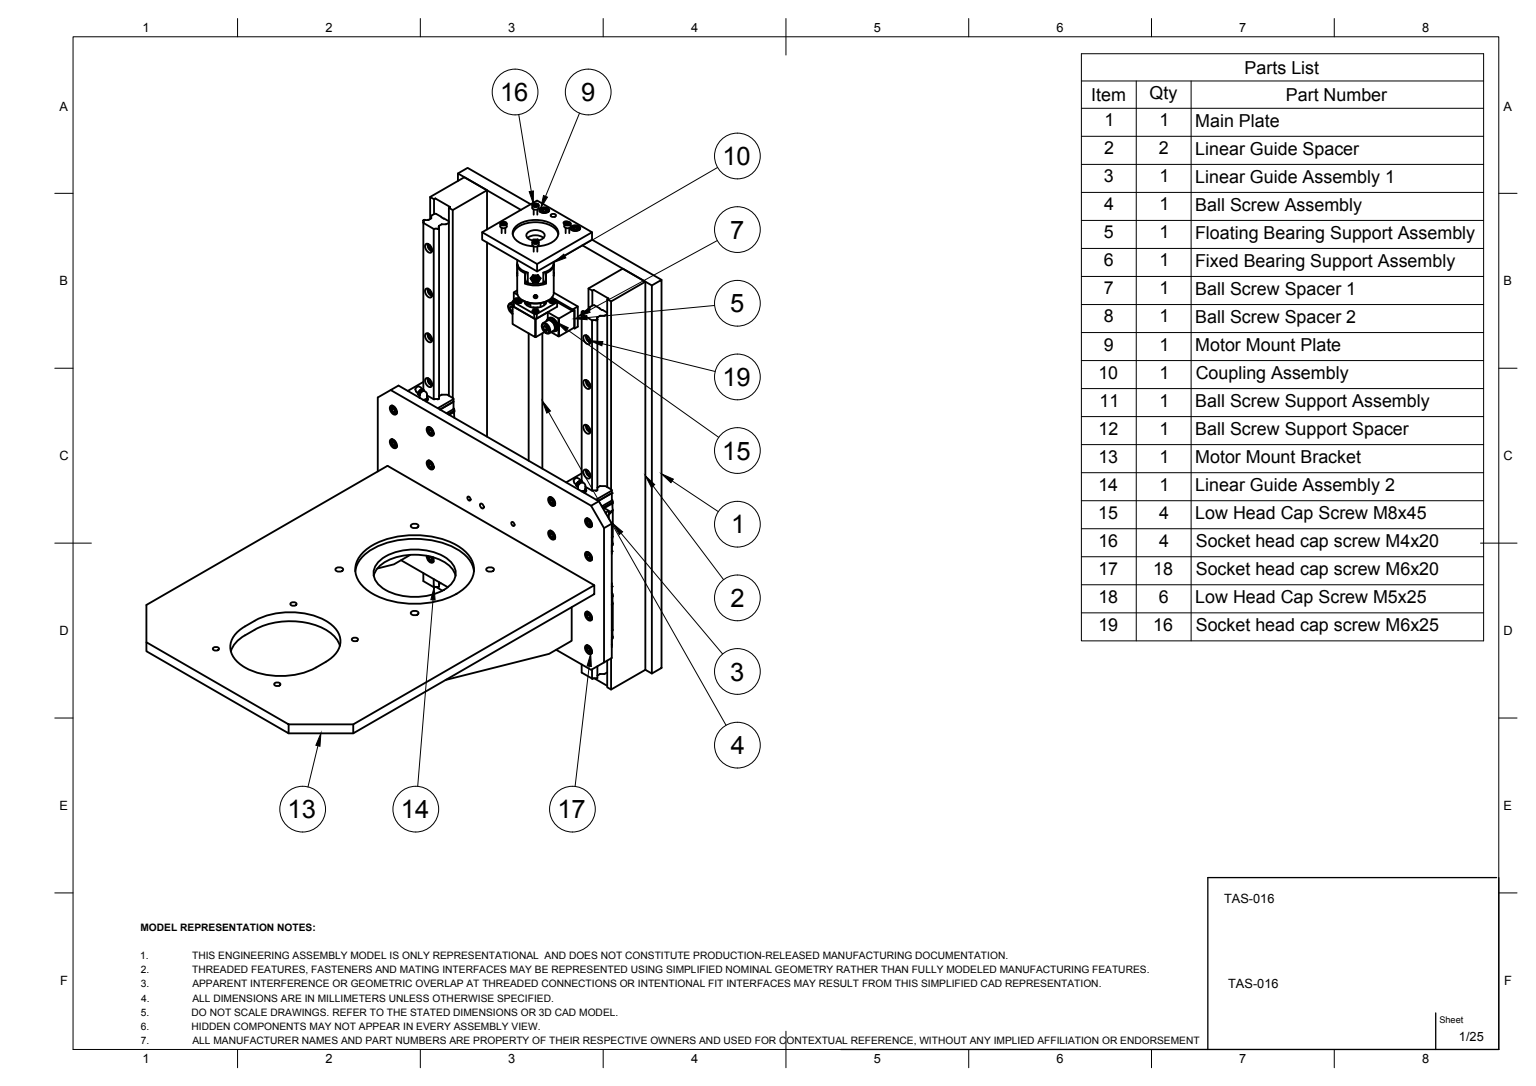
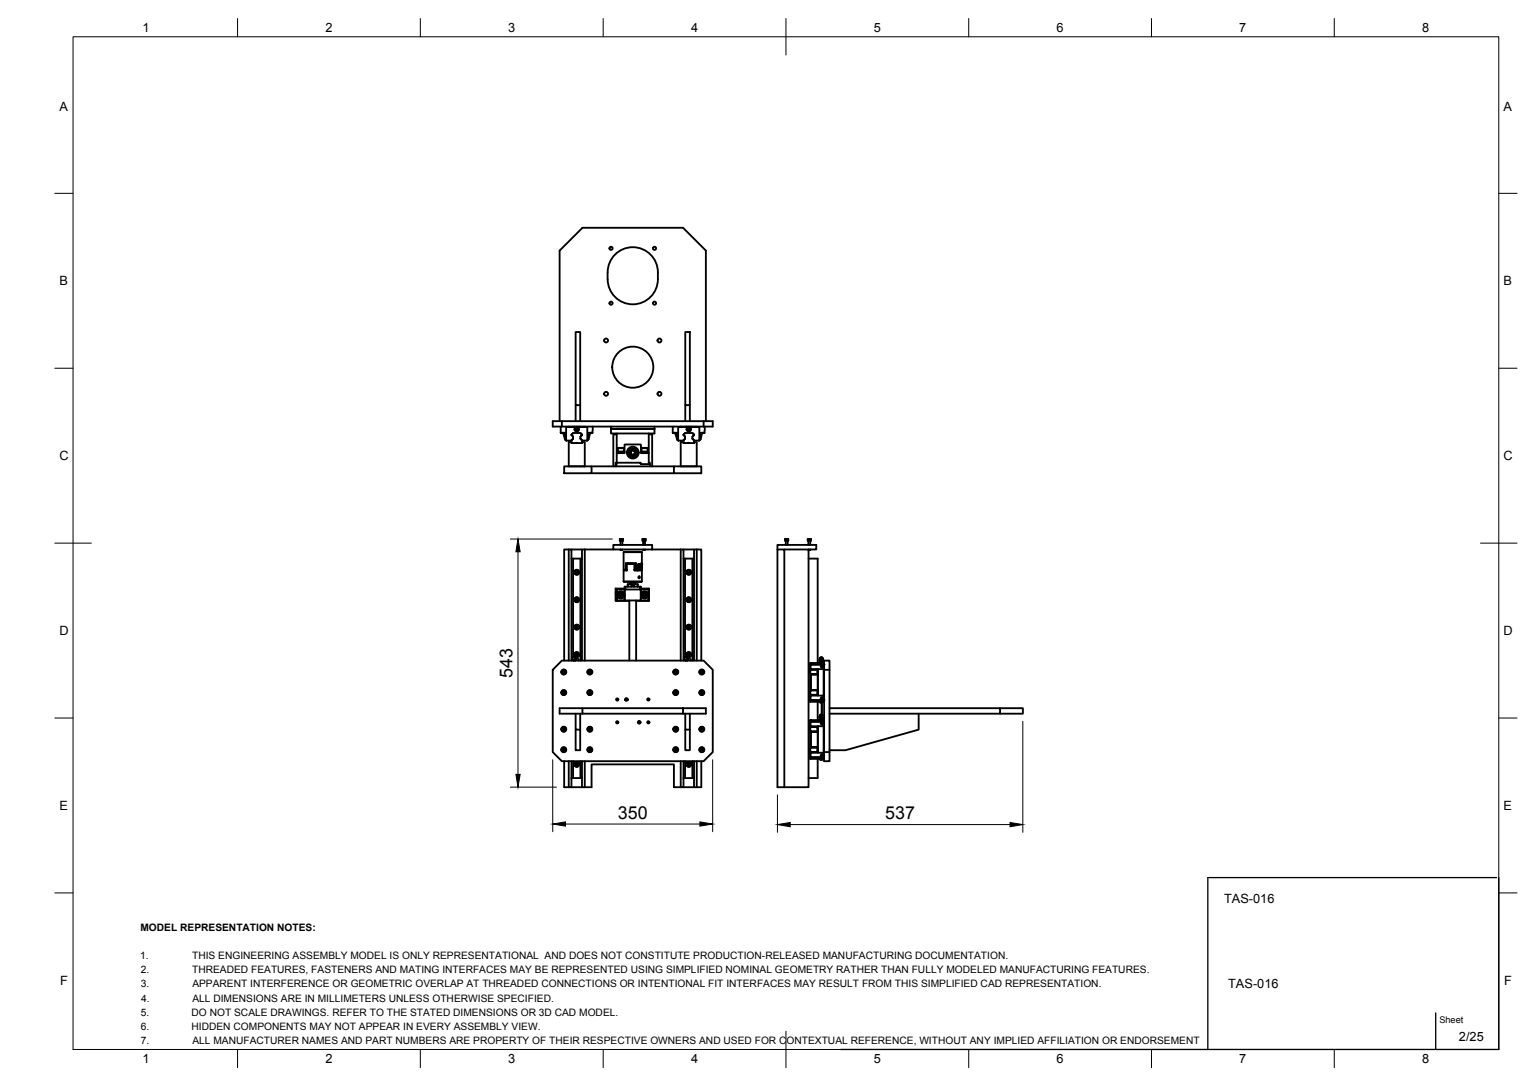
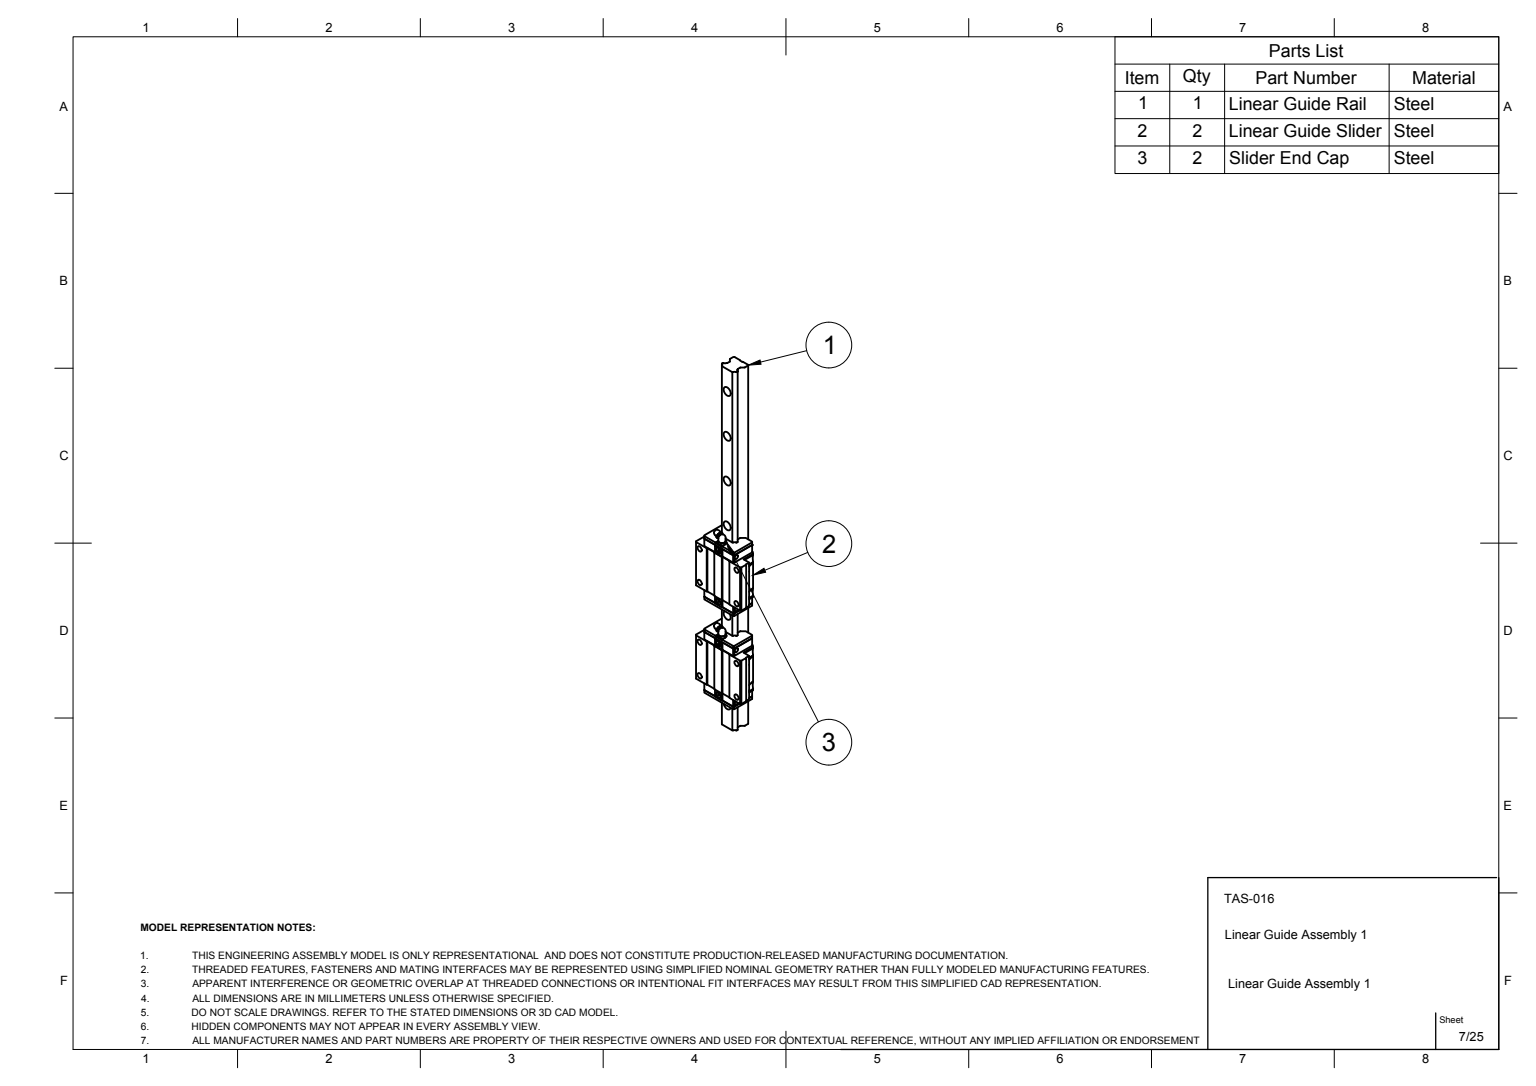
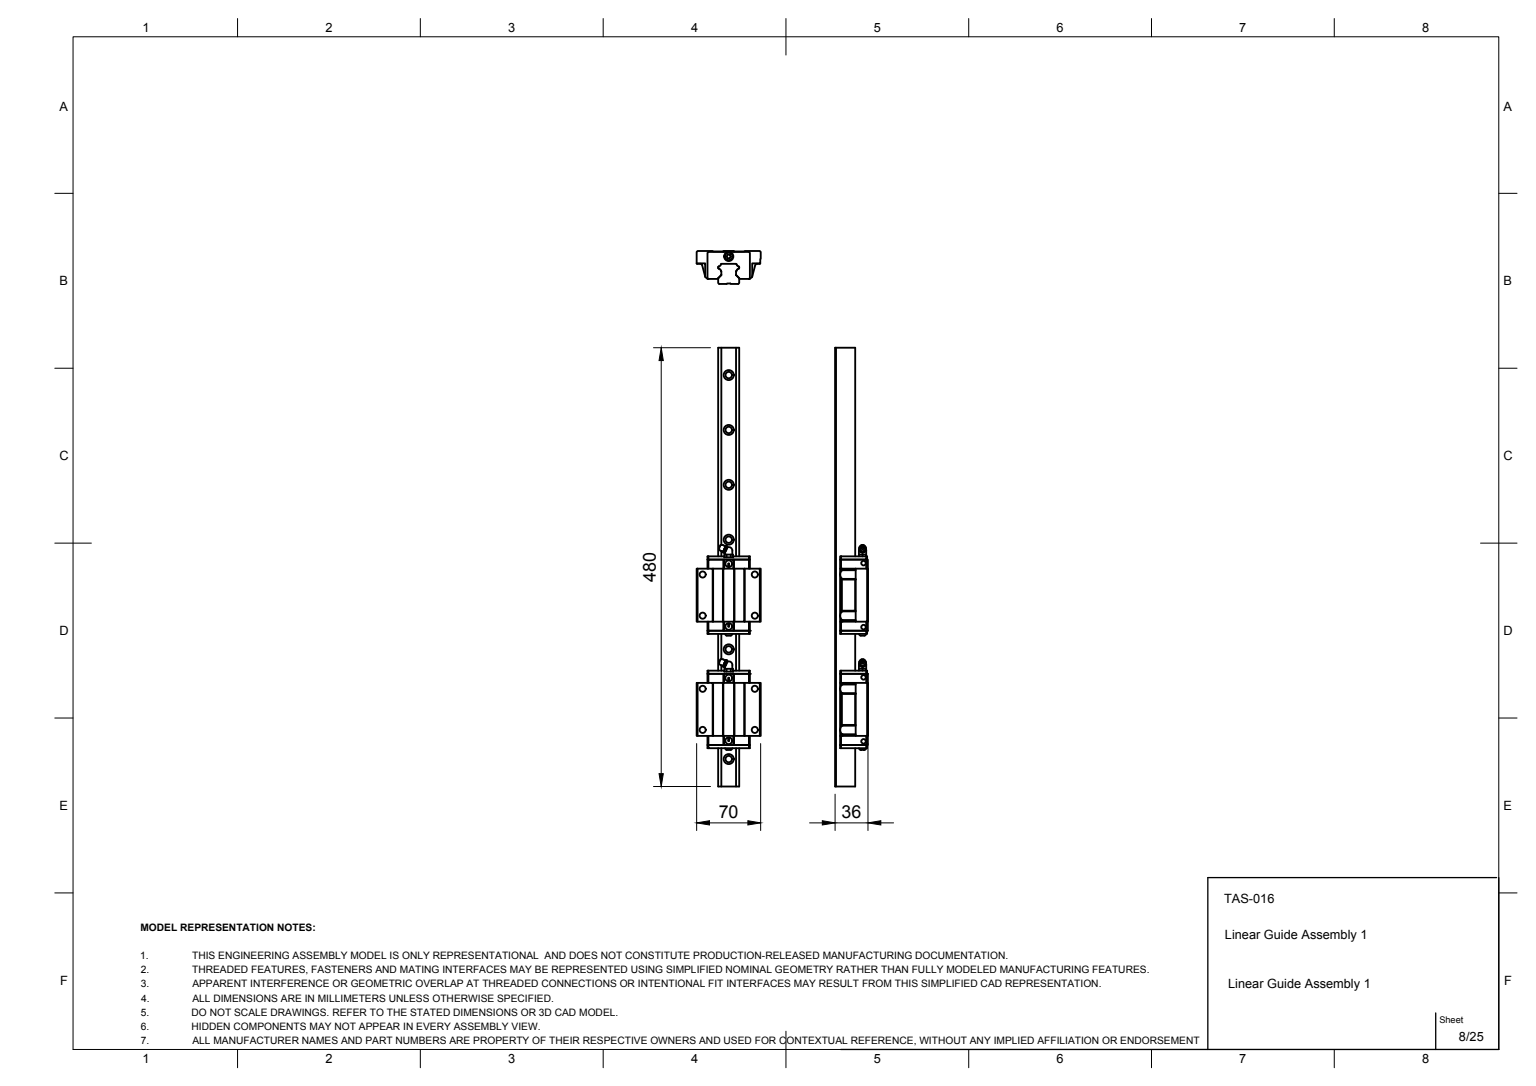
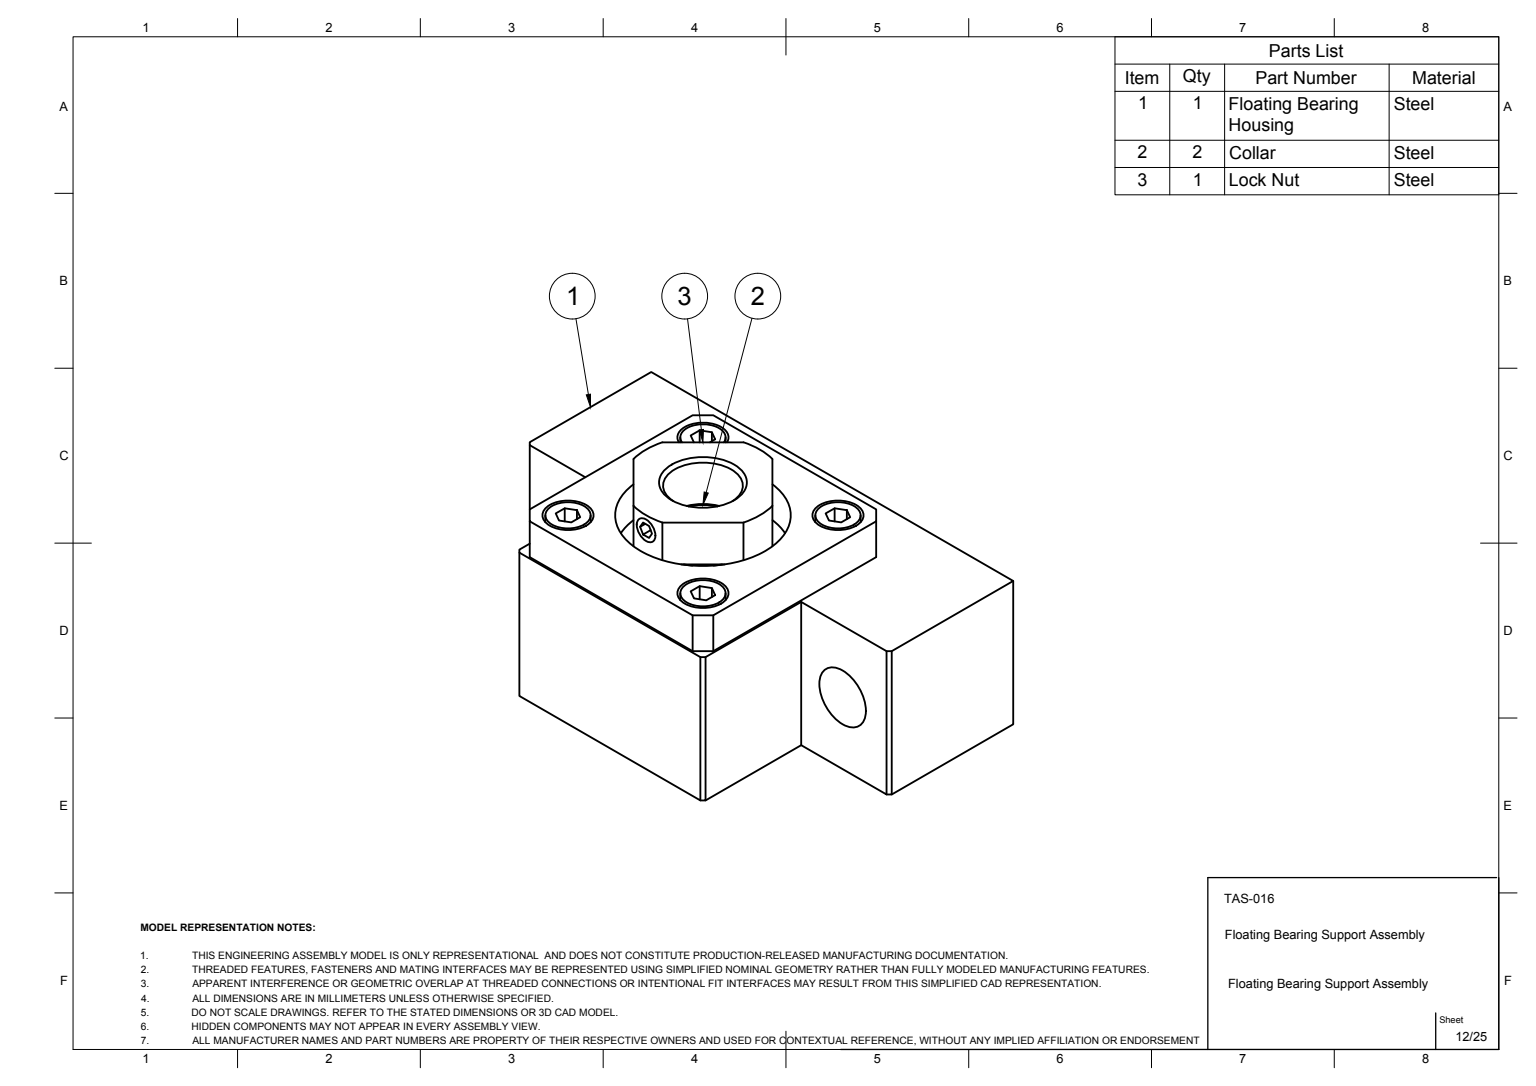
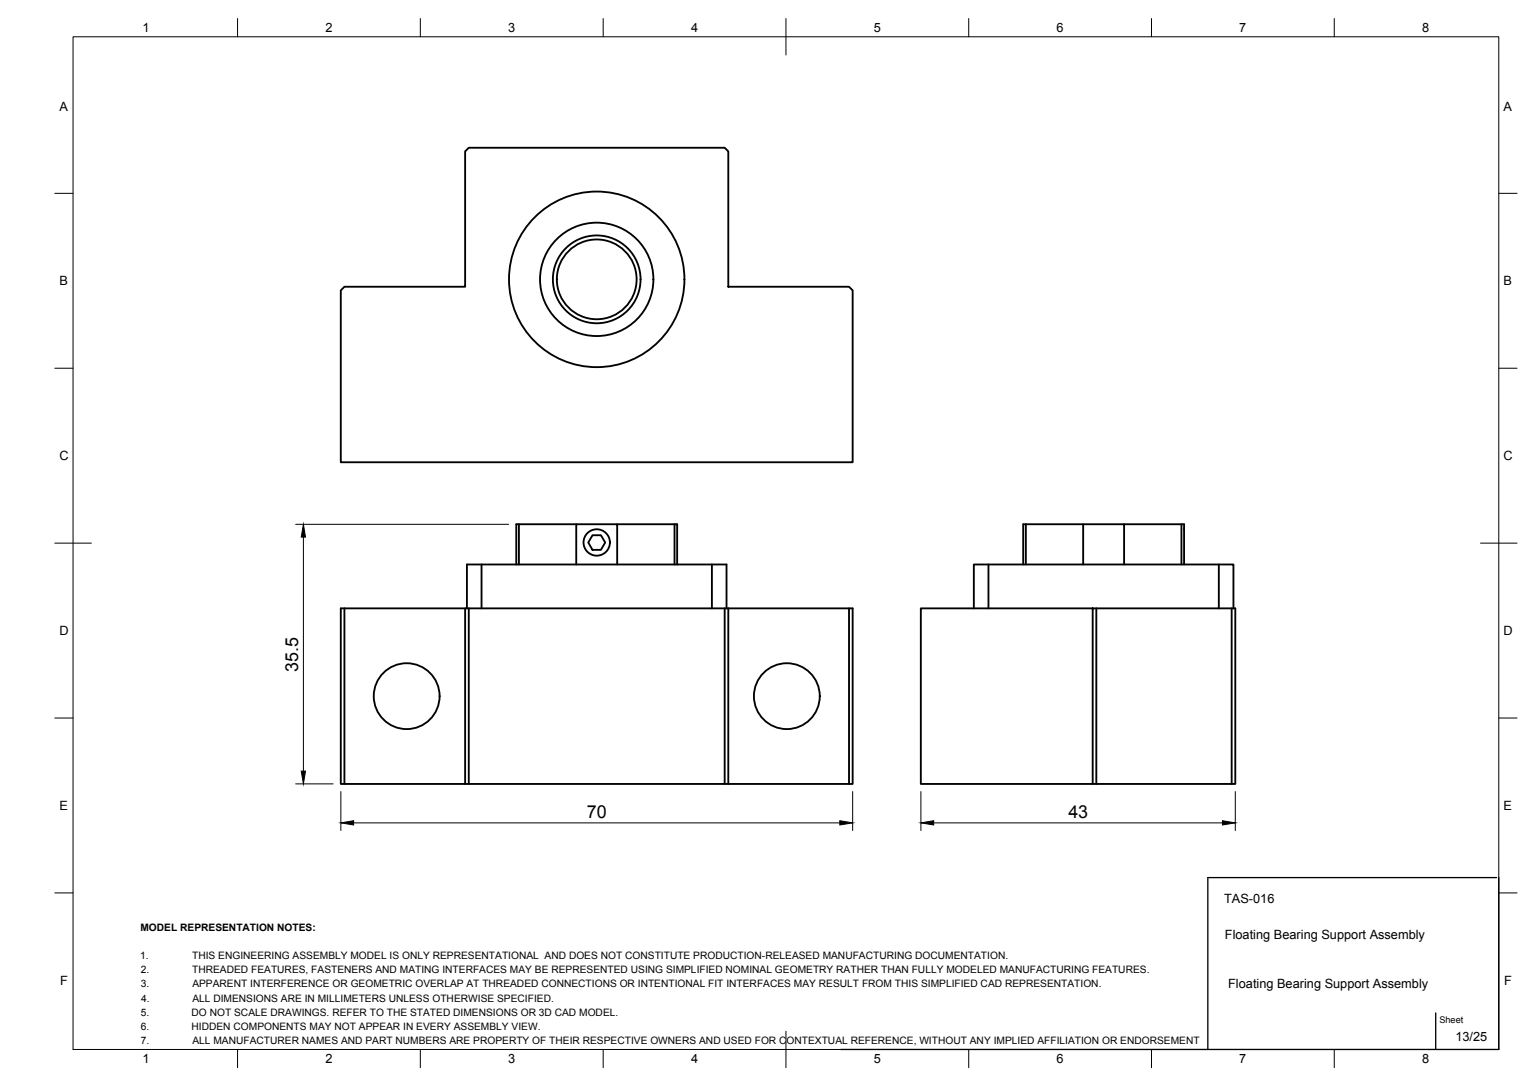
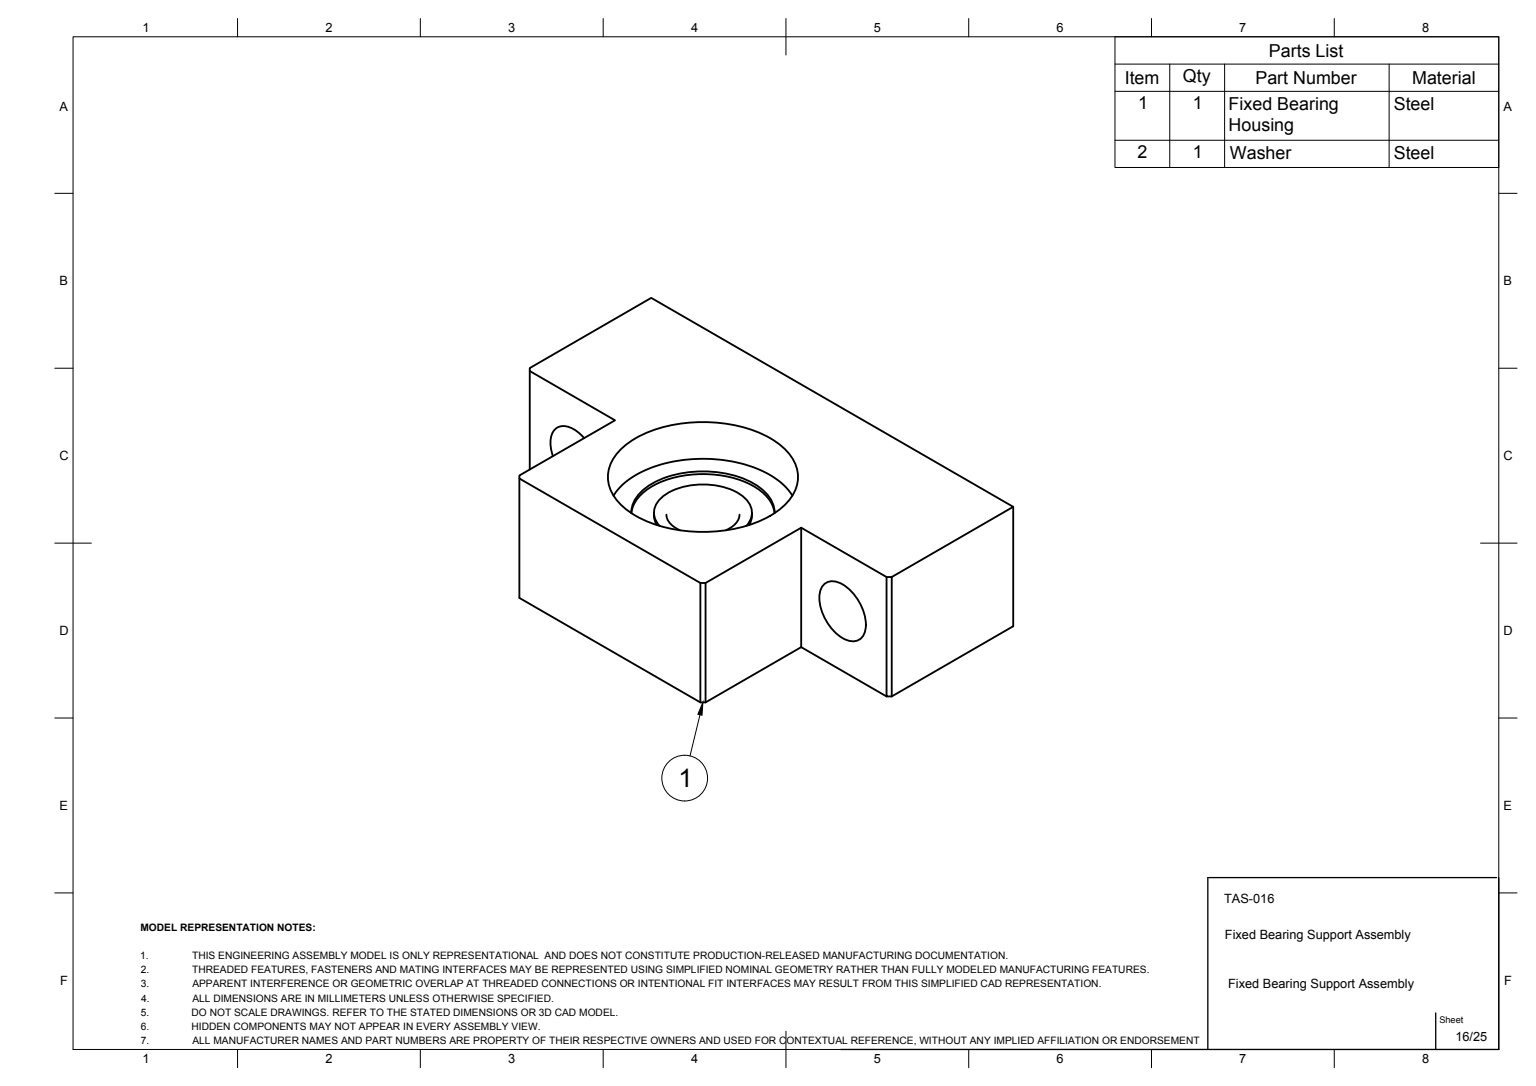
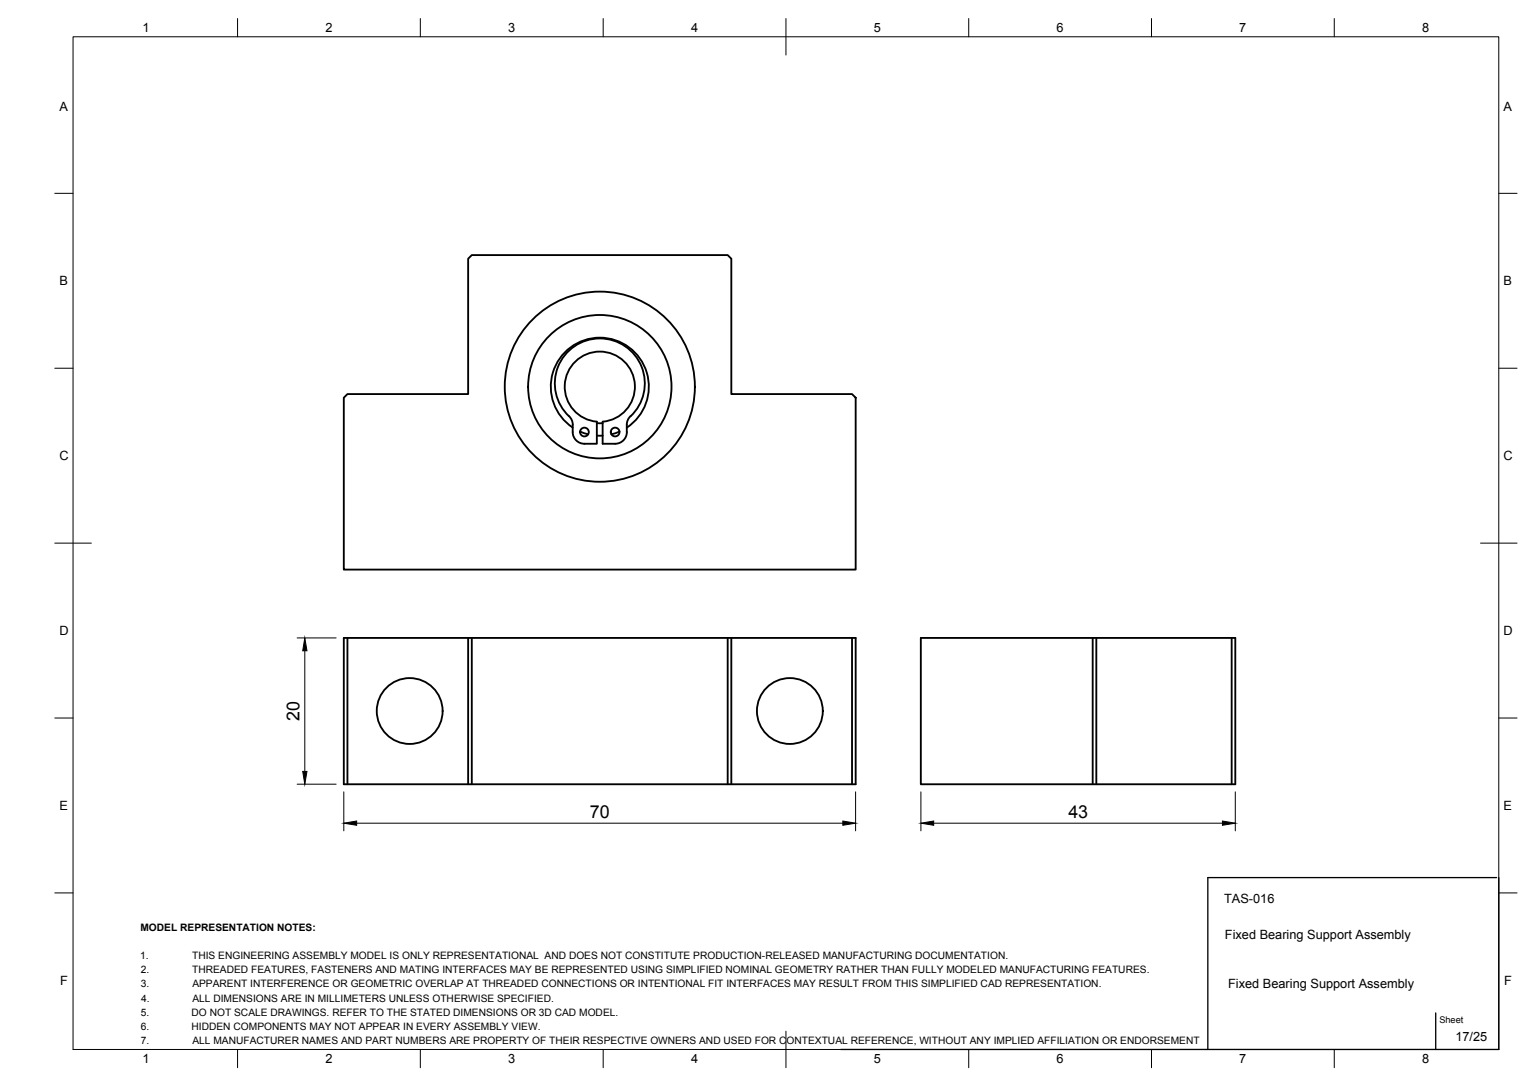
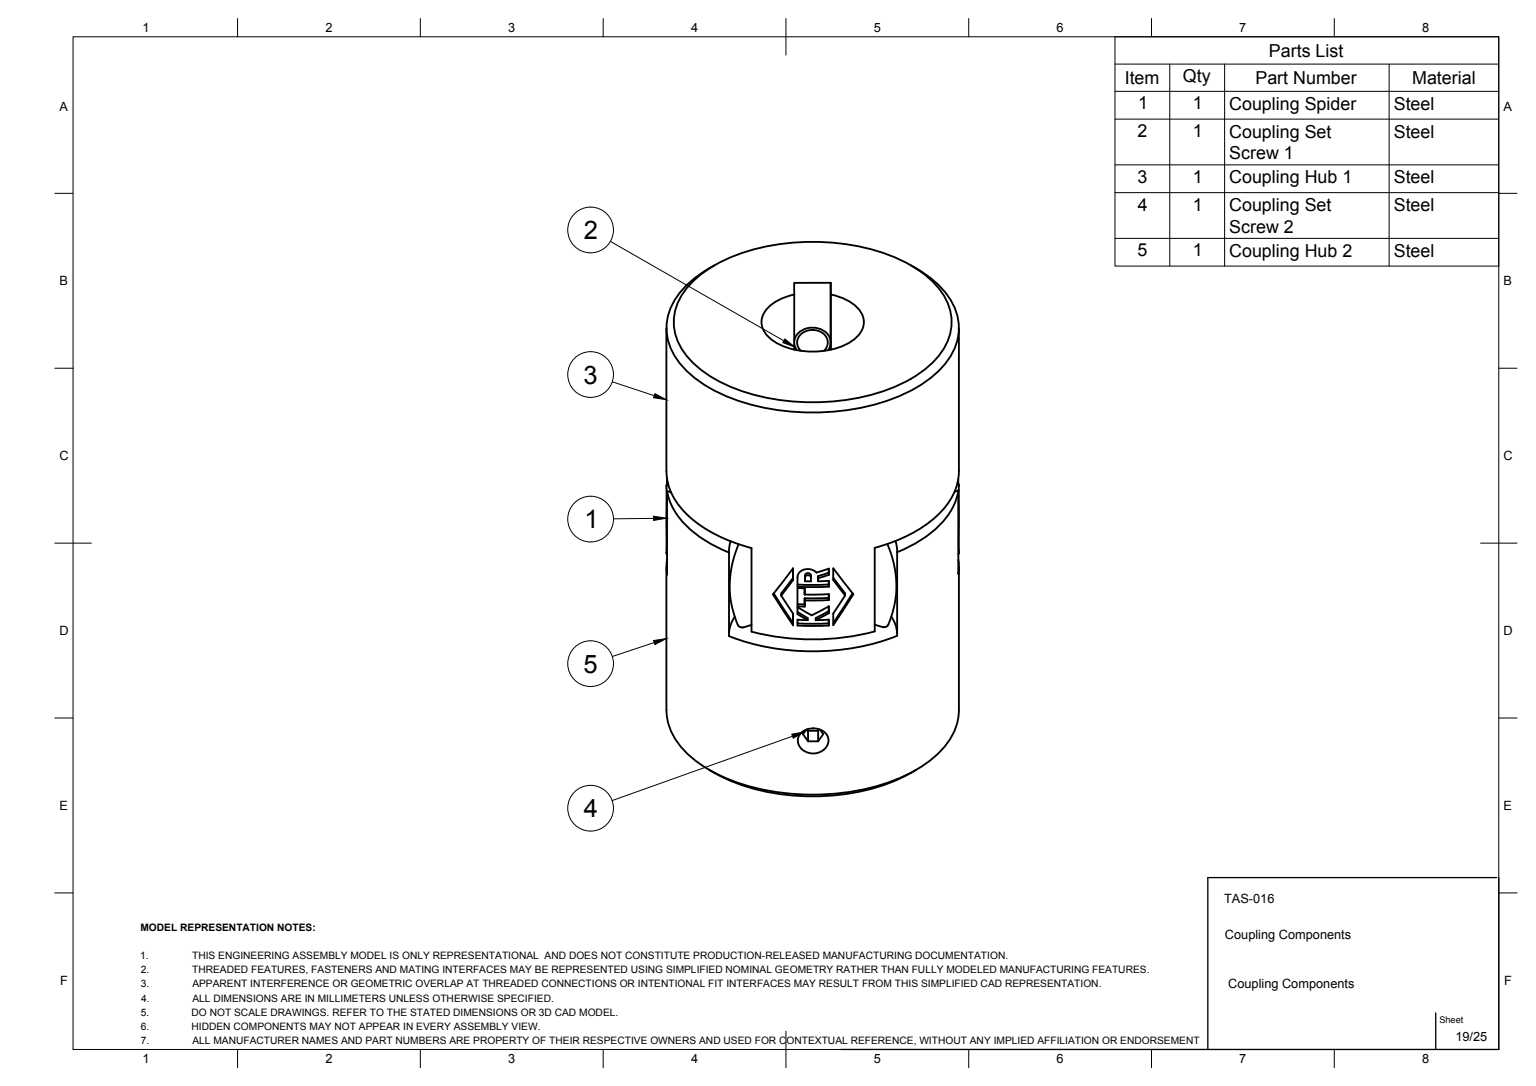
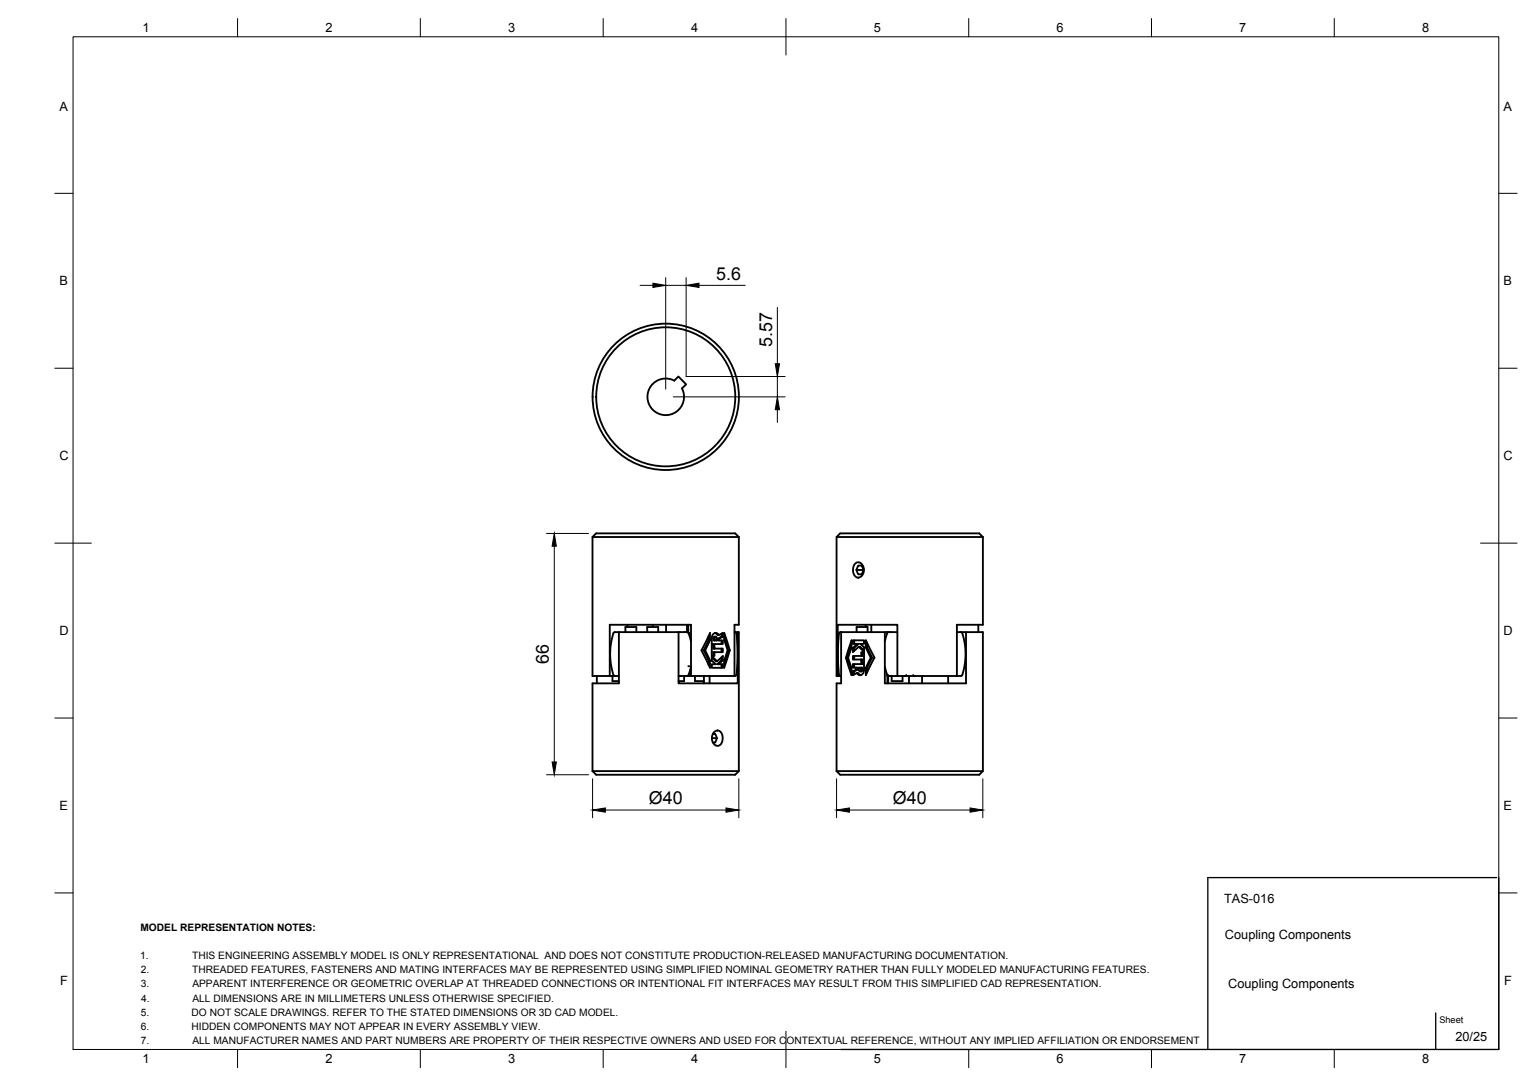
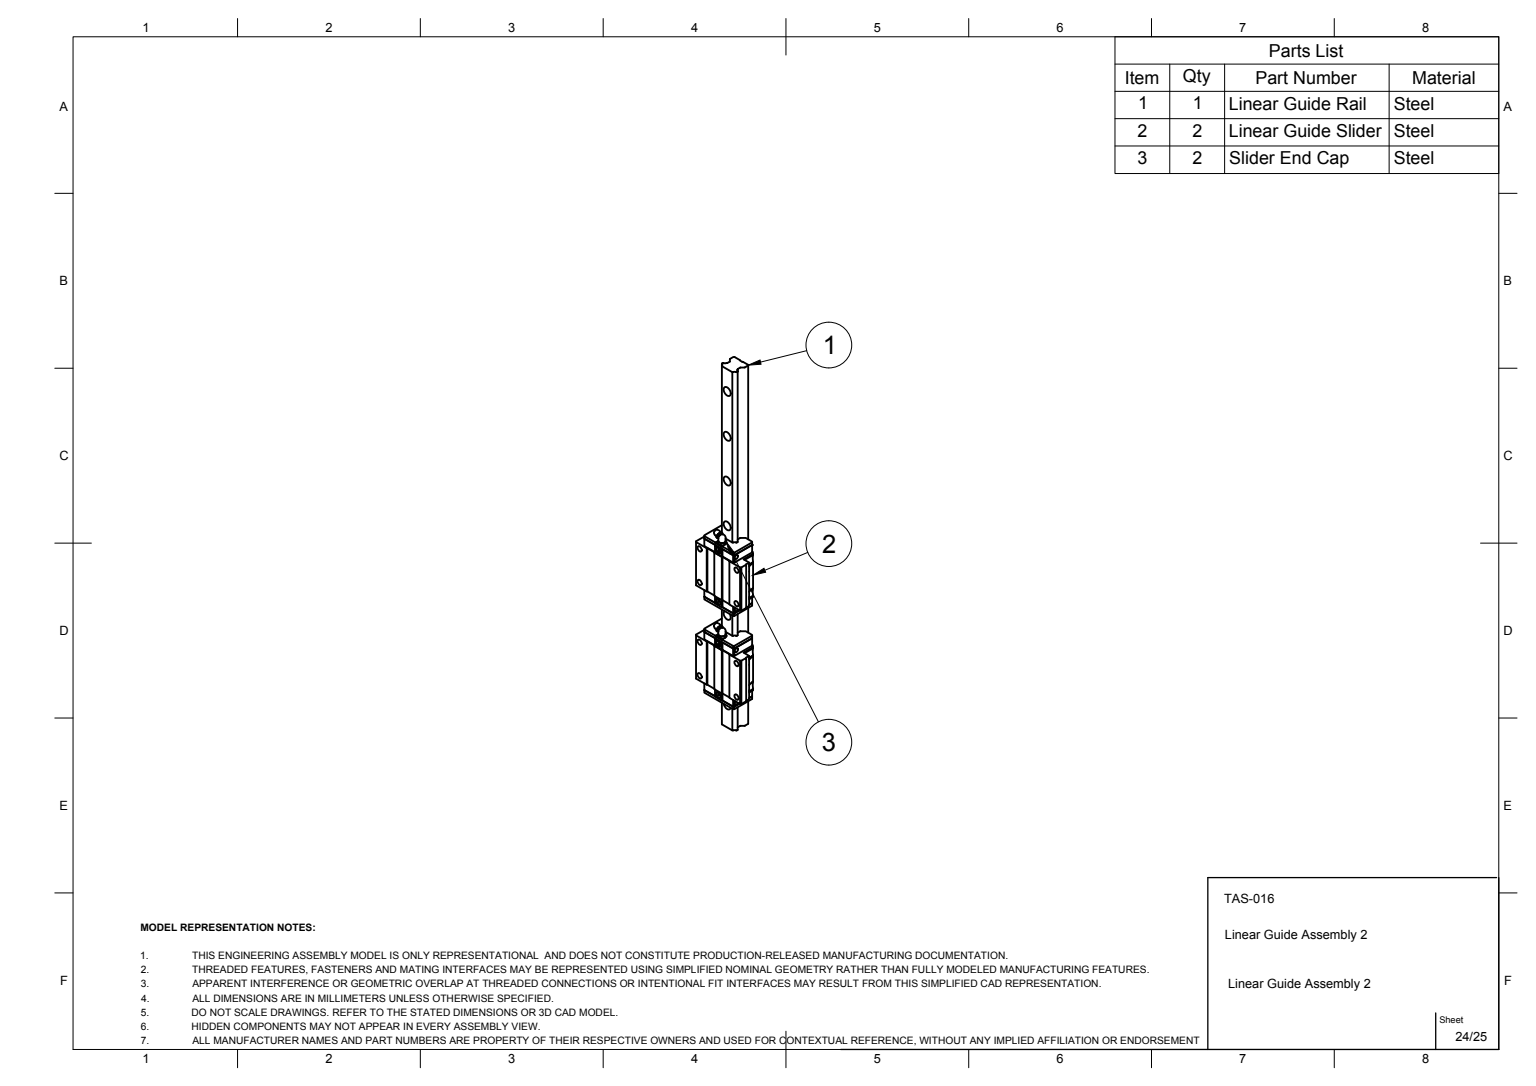
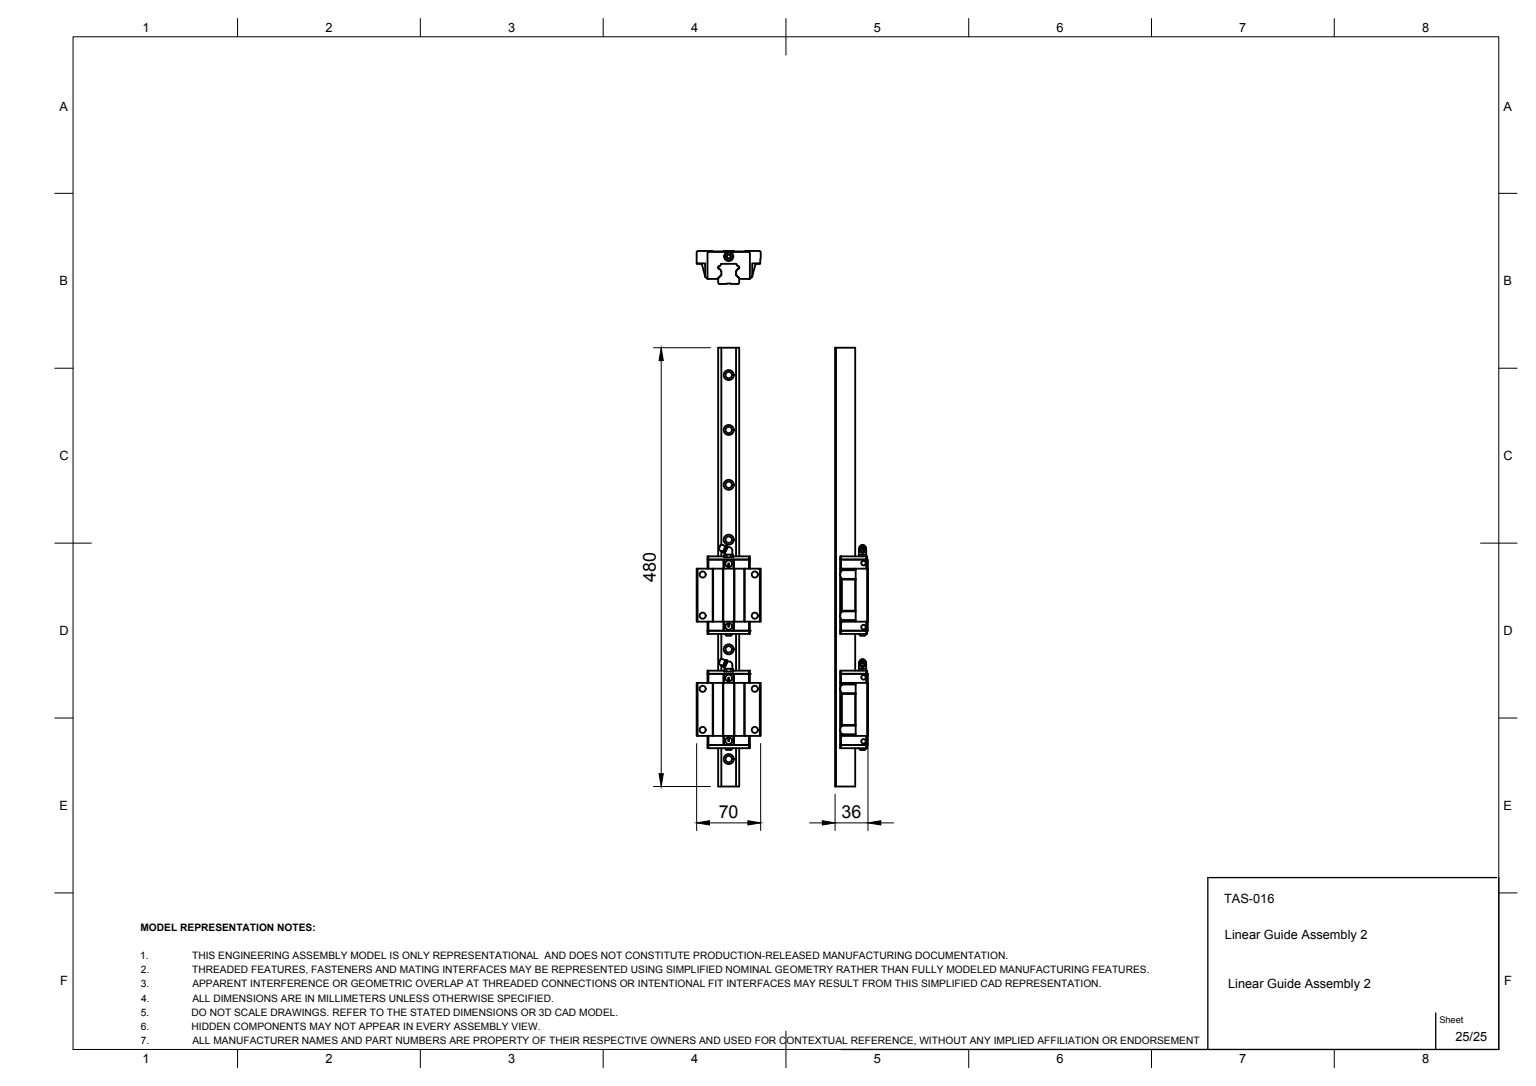
ISO-10303-21;
HEADER;
/* Generated by software containing ST-Developer
 * from STEP Tools, Inc. (www.steptools.com) 
 */

FILE_DESCRIPTION(
/* description */ ('STEP AP214'),
/* implementation_level */ '2;1');

FILE_NAME(
/* name */ 'TAS-016.step',
/* time_stamp */ '2026-11-15T14:55:55-08:00',
/* author */ (''),
/* organization */ (''),
/* preprocessor_version */ 'ST-DEVELOPER v20.2',
/* originating_system */ 'Autodesk Translation Framework v15.17.0.0',
/* authorisation */ '');

FILE_SCHEMA (('AUTOMOTIVE_DESIGN { 1 0 10303 214 3 1 1 }'));
ENDSEC;

DATA;
#10=MECHANICAL_DESIGN_GEOMETRIC_PRESENTATION_REPRESENTATION('',(#926,#927,
#928,#929,#930,#931,#932,#933,#934,#935,#936,#937,#938,#939,#940,#941,#942,
#943,#944,#945,#946,#947,#948,#949,#950,#951,#952,#953,#954,#955,#956,#957,
#958,#959,#960,#961,#962),#57079);
#11=(
BOUNDED_CURVE()
B_SPLINE_CURVE(2,(#54195,#54196,#54197),.UNSPECIFIED.,.F.,.F.)
B_SPLINE_CURVE_WITH_KNOTS((3,3),(-1.29356557390797,0.),.UNSPECIFIED.)
CURVE()
GEOMETRIC_REPRESENTATION_ITEM()
RATIONAL_B_SPLINE_CURVE((0.954658532851732,0.77704632554749,1.))
REPRESENTATION_ITEM('')
);
#12=(
BOUNDED_CURVE()
B_SPLINE_CURVE(2,(#56108,#56109,#56110),.UNSPECIFIED.,.F.,.F.)
B_SPLINE_CURVE_WITH_KNOTS((3,3),(-1.38994780338837,-1.00314154055664),
 .UNSPECIFIED.)
CURVE()
GEOMETRIC_REPRESENTATION_ITEM()
RATIONAL_B_SPLINE_CURVE((1.79495951130746,1.93380011269289,1.93380011269289))
REPRESENTATION_ITEM('')
);
#13=(
BOUNDED_CURVE()
B_SPLINE_CURVE(2,(#56111,#56112,#56113),.UNSPECIFIED.,.F.,.F.)
B_SPLINE_CURVE_WITH_KNOTS((3,3),(-1.00619430729118,-0.618602381117838),
 .UNSPECIFIED.)
CURVE()
GEOMETRIC_REPRESENTATION_ITEM()
RATIONAL_B_SPLINE_CURVE((1.93745653739061,1.93745653739061,1.7983534165231))
REPRESENTATION_ITEM('')
);
#14=(
BOUNDED_CURVE()
B_SPLINE_CURVE(2,(#56119,#56120,#56121),.UNSPECIFIED.,.F.,.F.)
B_SPLINE_CURVE_WITH_KNOTS((3,3),(-1.38994780338837,-1.00314154055664),
 .UNSPECIFIED.)
CURVE()
GEOMETRIC_REPRESENTATION_ITEM()
RATIONAL_B_SPLINE_CURVE((1.79495951130745,1.93380011269288,1.93380011269288))
REPRESENTATION_ITEM('')
);
#15=(
BOUNDED_CURVE()
B_SPLINE_CURVE(2,(#56122,#56123,#56124),.UNSPECIFIED.,.F.,.F.)
B_SPLINE_CURVE_WITH_KNOTS((3,3),(-1.00619430729117,-0.618602381117832),
 .UNSPECIFIED.)
CURVE()
GEOMETRIC_REPRESENTATION_ITEM()
RATIONAL_B_SPLINE_CURVE((1.9374565373906,1.9374565373906,1.79835341652309))
REPRESENTATION_ITEM('')
);
#16=(
BOUNDED_CURVE()
B_SPLINE_CURVE(2,(#56246,#56247,#56248),.UNSPECIFIED.,.F.,.F.)
B_SPLINE_CURVE_WITH_KNOTS((3,3),(-1.14357963809553,-0.720457873954785),
 .UNSPECIFIED.)
CURVE()
GEOMETRIC_REPRESENTATION_ITEM()
RATIONAL_B_SPLINE_CURVE((2.10284386262275,2.10284386262275,1.95186646604709))
REPRESENTATION_ITEM('')
);
#17=(
BOUNDED_CURVE()
B_SPLINE_CURVE(2,(#56249,#56250,#56251),.UNSPECIFIED.,.F.,.F.)
B_SPLINE_CURVE_WITH_KNOTS((3,3),(-1.51402948258723,-1.10175646251728),
 .UNSPECIFIED.)
CURVE()
GEOMETRIC_REPRESENTATION_ITEM()
RATIONAL_B_SPLINE_CURVE((1.90498640166842,2.0523376126434,2.0523376126434))
REPRESENTATION_ITEM('')
);
#18=(
BOUNDED_CURVE()
B_SPLINE_CURVE(2,(#56254,#56255,#56256),.UNSPECIFIED.,.F.,.F.)
B_SPLINE_CURVE_WITH_KNOTS((3,3),(-1.00619430729147,-0.618602381118052),
 .UNSPECIFIED.)
CURVE()
GEOMETRIC_REPRESENTATION_ITEM()
RATIONAL_B_SPLINE_CURVE((1.93745653739095,1.93745653739095,1.79835341652342))
REPRESENTATION_ITEM('')
);
#19=(
BOUNDED_CURVE()
B_SPLINE_CURVE(2,(#56257,#56258,#56259),.UNSPECIFIED.,.F.,.F.)
B_SPLINE_CURVE_WITH_KNOTS((3,3),(-1.59428966155348,-1.16547770853232),
 .UNSPECIFIED.)
CURVE()
GEOMETRIC_REPRESENTATION_ITEM()
RATIONAL_B_SPLINE_CURVE((1.97645710138757,2.12933659022722,2.12933659022723))
REPRESENTATION_ITEM('')
);
#20=(
BOUNDED_CURVE()
B_SPLINE_CURVE(2,(#56262,#56263,#56264),.UNSPECIFIED.,.F.,.F.)
B_SPLINE_CURVE_WITH_KNOTS((3,3),(-1.39378623346489,-1.00619430729147),
 .UNSPECIFIED.)
CURVE()
GEOMETRIC_REPRESENTATION_ITEM()
RATIONAL_B_SPLINE_CURVE((1.79835341652342,1.93745653739095,1.93745653739095))
REPRESENTATION_ITEM('')
);
#21=(
BOUNDED_CURVE()
B_SPLINE_CURVE(2,(#56265,#56266,#56267),.UNSPECIFIED.,.F.,.F.)
B_SPLINE_CURVE_WITH_KNOTS((3,3),(-1.00314154055692,-0.616335277725119),
 .UNSPECIFIED.)
CURVE()
GEOMETRIC_REPRESENTATION_ITEM()
RATIONAL_B_SPLINE_CURVE((1.93380011269323,1.93380011269323,1.79495951130777))
REPRESENTATION_ITEM('')
);
#22=(
BOUNDED_CURVE()
B_SPLINE_CURVE(2,(#56270,#56271,#56272),.UNSPECIFIED.,.F.,.F.)
B_SPLINE_CURVE_WITH_KNOTS((3,3),(-1.38994780338873,-1.00314154055692),
 .UNSPECIFIED.)
CURVE()
GEOMETRIC_REPRESENTATION_ITEM()
RATIONAL_B_SPLINE_CURVE((1.79495951130777,1.93380011269323,1.93380011269323))
REPRESENTATION_ITEM('')
);
#23=(
BOUNDED_CURVE()
B_SPLINE_CURVE(2,(#56273,#56274,#56275),.UNSPECIFIED.,.F.,.F.)
B_SPLINE_CURVE_WITH_KNOTS((3,3),(-1.16547770853232,-0.73666575551116),
 .UNSPECIFIED.)
CURVE()
GEOMETRIC_REPRESENTATION_ITEM()
RATIONAL_B_SPLINE_CURVE((2.12933659022723,2.12933659022723,1.97645710138758))
REPRESENTATION_ITEM('')
);
#24=(
BOUNDED_CURVE()
B_SPLINE_CURVE(2,(#56278,#56279,#56280),.UNSPECIFIED.,.F.,.F.)
B_SPLINE_CURVE_WITH_KNOTS((3,3),(-1.56670140223628,-1.14357963809553),
 .UNSPECIFIED.)
CURVE()
GEOMETRIC_REPRESENTATION_ITEM()
RATIONAL_B_SPLINE_CURVE((1.95186646604709,2.10284386262275,2.10284386262275))
REPRESENTATION_ITEM('')
);
#25=(
BOUNDED_CURVE()
B_SPLINE_CURVE(2,(#56281,#56282,#56283),.UNSPECIFIED.,.F.,.F.)
B_SPLINE_CURVE_WITH_KNOTS((3,3),(-1.09872453323964,-0.687236958819027),
 .UNSPECIFIED.)
CURVE()
GEOMETRIC_REPRESENTATION_ITEM()
RATIONAL_B_SPLINE_CURVE((2.04868118794568,2.04868118794568,1.90159249645282))
REPRESENTATION_ITEM('')
);
#26=(
BOUNDED_CURVE()
B_SPLINE_CURVE(2,(#56286,#56287,#56288),.UNSPECIFIED.,.F.,.F.)
B_SPLINE_CURVE_WITH_KNOTS((3,3),(-1.56670140224009,-1.14357963809856),
 .UNSPECIFIED.)
CURVE()
GEOMETRIC_REPRESENTATION_ITEM()
RATIONAL_B_SPLINE_CURVE((1.9518664660505,2.10284386262641,2.10284386262641))
REPRESENTATION_ITEM('')
);
#27=(
BOUNDED_CURVE()
B_SPLINE_CURVE(2,(#56289,#56290,#56291),.UNSPECIFIED.,.F.,.F.)
B_SPLINE_CURVE_WITH_KNOTS((3,3),(-1.10777980342349,-0.69394596557458),
 .UNSPECIFIED.)
CURVE()
GEOMETRIC_REPRESENTATION_ITEM()
RATIONAL_B_SPLINE_CURVE((2.05960365436383,2.05960365436383,1.91173076506448))
REPRESENTATION_ITEM('')
);
#28=(
BOUNDED_CURVE()
B_SPLINE_CURVE(2,(#56294,#56295,#56296),.UNSPECIFIED.,.F.,.F.)
B_SPLINE_CURVE_WITH_KNOTS((3,3),(-1.40141169651805,-1.01225852375907),
 .UNSPECIFIED.)
CURVE()
GEOMETRIC_REPRESENTATION_ITEM()
RATIONAL_B_SPLINE_CURVE((1.80509777991977,1.94472257911162,1.94472257911162))
REPRESENTATION_ITEM('')
);
#29=(
BOUNDED_CURVE()
B_SPLINE_CURVE(2,(#56297,#56298,#56299),.UNSPECIFIED.,.F.,.F.)
B_SPLINE_CURVE_WITH_KNOTS((3,3),(-1.16547770853319,-0.736665755511809),
 .UNSPECIFIED.)
CURVE()
GEOMETRIC_REPRESENTATION_ITEM()
RATIONAL_B_SPLINE_CURVE((2.12933659022829,2.12933659022829,1.97645710138856))
REPRESENTATION_ITEM('')
);
#30=(
BOUNDED_CURVE()
B_SPLINE_CURVE(2,(#56302,#56303,#56304),.UNSPECIFIED.,.F.,.F.)
B_SPLINE_CURVE_WITH_KNOTS((3,3),(-1.40141169651807,-1.01225852375909),
 .UNSPECIFIED.)
CURVE()
GEOMETRIC_REPRESENTATION_ITEM()
RATIONAL_B_SPLINE_CURVE((1.80509777991979,1.94472257911164,1.94472257911164))
REPRESENTATION_ITEM('')
);
#31=(
BOUNDED_CURVE()
B_SPLINE_CURVE(2,(#56305,#56306,#56307),.UNSPECIFIED.,.F.,.F.)
B_SPLINE_CURVE_WITH_KNOTS((3,3),(-1.01225852375907,-0.623105351000092),
 .UNSPECIFIED.)
CURVE()
GEOMETRIC_REPRESENTATION_ITEM()
RATIONAL_B_SPLINE_CURVE((1.94472257911162,1.94472257911162,1.80509777991977))
REPRESENTATION_ITEM('')
);
#32=(
BOUNDED_CURVE()
B_SPLINE_CURVE(2,(#56310,#56311,#56312),.UNSPECIFIED.,.F.,.F.)
B_SPLINE_CURVE_WITH_KNOTS((3,3),(-1.59428966155458,-1.16547770853319),
 .UNSPECIFIED.)
CURVE()
GEOMETRIC_REPRESENTATION_ITEM()
RATIONAL_B_SPLINE_CURVE((1.97645710138856,2.12933659022828,2.12933659022828))
REPRESENTATION_ITEM('')
);
#33=(
BOUNDED_CURVE()
B_SPLINE_CURVE(2,(#56313,#56314,#56315),.UNSPECIFIED.,.F.,.F.)
B_SPLINE_CURVE_WITH_KNOTS((3,3),(-1.01225852375909,-0.623105351000104),
 .UNSPECIFIED.)
CURVE()
GEOMETRIC_REPRESENTATION_ITEM()
RATIONAL_B_SPLINE_CURVE((1.94472257911164,1.94472257911164,1.80509777991979))
REPRESENTATION_ITEM('')
);
#34=(
BOUNDED_CURVE()
B_SPLINE_CURVE(2,(#56318,#56319,#56320),.UNSPECIFIED.,.F.,.F.)
B_SPLINE_CURVE_WITH_KNOTS((3,3),(-1.52161364127241,-1.1077798034235),
 .UNSPECIFIED.)
CURVE()
GEOMETRIC_REPRESENTATION_ITEM()
RATIONAL_B_SPLINE_CURVE((1.91173076506449,2.05960365436384,2.05960365436384))
REPRESENTATION_ITEM('')
);
#35=(
BOUNDED_CURVE()
B_SPLINE_CURVE(2,(#56321,#56322,#56323),.UNSPECIFIED.,.F.,.F.)
B_SPLINE_CURVE_WITH_KNOTS((3,3),(-1.14357963809856,-0.720457873957025),
 .UNSPECIFIED.)
CURVE()
GEOMETRIC_REPRESENTATION_ITEM()
RATIONAL_B_SPLINE_CURVE((2.10284386262641,2.10284386262641,1.95186646605049))
REPRESENTATION_ITEM('')
);
#36=B_SPLINE_SURFACE_WITH_KNOTS('',3,3,((#37392,#37393,#37394,#37395,#37396),
(#37397,#37398,#37399,#37400,#37401),(#37402,#37403,#37404,#37405,#37406),
(#37407,#37408,#37409,#37410,#37411),(#37412,#37413,#37414,#37415,#37416),
(#37417,#37418,#37419,#37420,#37421),(#37422,#37423,#37424,#37425,#37426)),
 .UNSPECIFIED.,.F.,.F.,.F.,(4,1,1,1,4),(4,1,4),(0.002628442342492,0.25,
0.5,0.75,0.9693574094799),(0.1621510896547,6.217857289747,12.27407139219),
 .UNSPECIFIED.);
#37=B_SPLINE_SURFACE_WITH_KNOTS('',3,3,((#38122,#38123,#38124,#38125,#38126),
(#38127,#38128,#38129,#38130,#38131),(#38132,#38133,#38134,#38135,#38136),
(#38137,#38138,#38139,#38140,#38141)),.UNSPECIFIED.,.F.,.F.,.F.,(4,4),(4,
1,4),(-0.024990257354348,0.982485330053312),(0.334063910607008,6.217857289747,
12.1016506682418),.UNSPECIFIED.);
#38=B_SPLINE_SURFACE_WITH_KNOTS('',3,3,((#38952,#38953,#38954,#38955,#38956),
(#38957,#38958,#38959,#38960,#38961),(#38962,#38963,#38964,#38965,#38966),
(#38967,#38968,#38969,#38970,#38971),(#38972,#38973,#38974,#38975,#38976),
(#38977,#38978,#38979,#38980,#38981),(#38982,#38983,#38984,#38985,#38986)),
 .UNSPECIFIED.,.F.,.F.,.F.,(4,1,1,1,4),(4,1,4),(0.0306420330999,0.25,0.5,
0.75,0.9973715693979),(0.1621509986241,6.217857289747,12.27408153313),
 .UNSPECIFIED.);
#39=B_SPLINE_SURFACE_WITH_KNOTS('',3,3,((#39922,#39923,#39924,#39925,#39926),
(#39927,#39928,#39929,#39930,#39931),(#39932,#39933,#39934,#39935,#39936),
(#39937,#39938,#39939,#39940,#39941),(#39942,#39943,#39944,#39945,#39946),
(#39947,#39948,#39949,#39950,#39951),(#39952,#39953,#39954,#39955,#39956)),
 .UNSPECIFIED.,.F.,.F.,.F.,(4,1,1,1,4),(4,1,4),(0.002628433572892,0.25,
0.5,0.75,0.9693578567347),(0.1621510896604,6.217857289747,12.27407139218),
 .UNSPECIFIED.);
#40=B_SPLINE_SURFACE_WITH_KNOTS('',3,3,((#40661,#40662,#40663,#40664,#40665),
(#40666,#40667,#40668,#40669,#40670),(#40671,#40672,#40673,#40674,#40675),
(#40676,#40677,#40678,#40679,#40680)),.UNSPECIFIED.,.F.,.F.,.F.,(4,4),(4,
1,4),(-0.0250566951233491,0.98252386483041),(0.33399816619982,6.217857289747,
12.1017164126489),.UNSPECIFIED.);
#41=B_SPLINE_SURFACE_WITH_KNOTS('',3,3,((#41491,#41492,#41493,#41494,#41495),
(#41496,#41497,#41498,#41499,#41500),(#41501,#41502,#41503,#41504,#41505),
(#41506,#41507,#41508,#41509,#41510),(#41511,#41512,#41513,#41514,#41515),
(#41516,#41517,#41518,#41519,#41520),(#41521,#41522,#41523,#41524,#41525)),
 .UNSPECIFIED.,.F.,.F.,.F.,(4,1,1,1,4),(4,1,4),(0.03064262133498,0.25,0.5,
0.75,0.9973715578641),(0.1621509986155,6.217857289747,12.27408153314),
 .UNSPECIFIED.);
#42=B_SPLINE_SURFACE_WITH_KNOTS('',3,3,((#42483,#42484,#42485,#42486,#42487),
(#42488,#42489,#42490,#42491,#42492),(#42493,#42494,#42495,#42496,#42497),
(#42498,#42499,#42500,#42501,#42502),(#42503,#42504,#42505,#42506,#42507),
(#42508,#42509,#42510,#42511,#42512),(#42513,#42514,#42515,#42516,#42517)),
 .UNSPECIFIED.,.F.,.F.,.F.,(4,1,1,1,4),(4,1,4),(0.002628427667201,0.25,
0.5,0.75,0.9693581579284),(0.1621510896466,6.217857289747,12.2740713922),
 .UNSPECIFIED.);
#43=B_SPLINE_SURFACE_WITH_KNOTS('',3,3,((#43199,#43200,#43201,#43202,#43203),
(#43204,#43205,#43206,#43207,#43208),(#43209,#43210,#43211,#43212,#43213),
(#43214,#43215,#43216,#43217,#43218)),.UNSPECIFIED.,.F.,.F.,.F.,(4,4),(4,
1,4),(-0.025111513161759,0.982555658087823),(0.333943919417255,6.217857289747,
12.1017706594305),.UNSPECIFIED.);
#44=B_SPLINE_SURFACE_WITH_KNOTS('',3,3,((#44029,#44030,#44031,#44032,#44033),
(#44034,#44035,#44036,#44037,#44038),(#44039,#44040,#44041,#44042,#44043),
(#44044,#44045,#44046,#44047,#44048),(#44049,#44050,#44051,#44052,#44053),
(#44054,#44055,#44056,#44057,#44058),(#44059,#44060,#44061,#44062,#44063)),
 .UNSPECIFIED.,.F.,.F.,.F.,(4,1,1,1,4),(4,1,4),(0.0306416740573,0.25,0.5,
0.75,0.9973715764379),(0.1621509986173,6.217857289747,12.27408153313),
 .UNSPECIFIED.);
#45=B_SPLINE_SURFACE_WITH_KNOTS('',3,3,((#45013,#45014,#45015,#45016,#45017),
(#45018,#45019,#45020,#45021,#45022),(#45023,#45024,#45025,#45026,#45027),
(#45028,#45029,#45030,#45031,#45032),(#45033,#45034,#45035,#45036,#45037),
(#45038,#45039,#45040,#45041,#45042),(#45043,#45044,#45045,#45046,#45047)),
 .UNSPECIFIED.,.F.,.F.,.F.,(4,1,1,1,4),(4,1,4),(0.002628398063673,0.25,
0.5,0.75,0.9693596677257),(0.1621510897017,6.217857289747,12.27407139231),
 .UNSPECIFIED.);
#46=B_SPLINE_SURFACE_WITH_KNOTS('',3,3,((#45733,#45734,#45735,#45736,#45737),
(#45738,#45739,#45740,#45741,#45742),(#45743,#45744,#45745,#45746,#45747),
(#45748,#45749,#45750,#45751,#45752)),.UNSPECIFIED.,.F.,.F.,.F.,(4,4),(4,
1,4),(-0.0251115131966662,0.982555658077179),(0.3339439193833,6.217857289747,
12.1017706594645),.UNSPECIFIED.);
#47=B_SPLINE_SURFACE_WITH_KNOTS('',3,3,((#46556,#46557,#46558,#46559,#46560),
(#46561,#46562,#46563,#46564,#46565),(#46566,#46567,#46568,#46569,#46570),
(#46571,#46572,#46573,#46574,#46575),(#46576,#46577,#46578,#46579,#46580),
(#46581,#46582,#46583,#46584,#46585),(#46586,#46587,#46588,#46589,#46590)),
 .UNSPECIFIED.,.F.,.F.,.F.,(4,1,1,1,4),(4,1,4),(0.03064220512297,0.25,0.5,
0.75,0.997371566025),(0.1621509986341,6.217857289747,12.27408153327),
 .UNSPECIFIED.);
#48=B_SPLINE_SURFACE_WITH_KNOTS('',3,3,((#47286,#47287,#47288,#47289,#47290),
(#47291,#47292,#47293,#47294,#47295),(#47296,#47297,#47298,#47299,#47300),
(#47301,#47302,#47303,#47304,#47305),(#47306,#47307,#47308,#47309,#47310),
(#47311,#47312,#47313,#47314,#47315),(#47316,#47317,#47318,#47319,#47320)),
 .UNSPECIFIED.,.F.,.F.,.F.,(4,1,1,1,4),(4,1,4),(0.002628430752027,0.25,
0.5,0.75,0.9693580006005),(0.1621510896555,6.217857289747,12.27407139218),
 .UNSPECIFIED.);
#49=B_SPLINE_SURFACE_WITH_KNOTS('',3,3,((#48651,#48652,#48653,#48654,#48655),
(#48656,#48657,#48658,#48659,#48660),(#48661,#48662,#48663,#48664,#48665),
(#48666,#48667,#48668,#48669,#48670),(#48671,#48672,#48673,#48674,#48675),
(#48676,#48677,#48678,#48679,#48680),(#48681,#48682,#48683,#48684,#48685)),
 .UNSPECIFIED.,.F.,.F.,.F.,(4,1,1,1,4),(4,1,4),(0.002629007110398,0.25,
0.5,0.75,0.9693286059854),(0.162151089685,6.217857289747,12.27407139234),
 .UNSPECIFIED.);
#50=B_SPLINE_SURFACE_WITH_KNOTS('',3,3,((#49402,#49403,#49404,#49405,#49406),
(#49407,#49408,#49409,#49410,#49411),(#49412,#49413,#49414,#49415,#49416),
(#49417,#49418,#49419,#49420,#49421)),.UNSPECIFIED.,.F.,.F.,.F.,(4,4),(4,
1,4),(-0.025177674866951,0.982594028216162),(0.333878446168046,6.217857289747,
12.1018361326796),.UNSPECIFIED.);
#51=B_SPLINE_SURFACE_WITH_KNOTS('',3,3,((#50226,#50227,#50228,#50229,#50230),
(#50231,#50232,#50233,#50234,#50235),(#50236,#50237,#50238,#50239,#50240),
(#50241,#50242,#50243,#50244,#50245),(#50246,#50247,#50248,#50249,#50250),
(#50251,#50252,#50253,#50254,#50255),(#50256,#50257,#50258,#50259,#50260)),
 .UNSPECIFIED.,.F.,.F.,.F.,(4,1,1,1,4),(4,1,4),(0.03067153885244,0.25,0.5,
0.75,0.9973709908605),(0.1621509986464,6.217857289747,12.27408153326),
 .UNSPECIFIED.);
#52=B_SPLINE_SURFACE_WITH_KNOTS('',3,3,((#50705,#50706,#50707,#50708,#50709),
(#50710,#50711,#50712,#50713,#50714),(#50715,#50716,#50717,#50718,#50719),
(#50720,#50721,#50722,#50723,#50724)),.UNSPECIFIED.,.F.,.F.,.F.,(4,4),(4,
1,4),(-0.0249902573400751,0.982485330102956),(0.334063910620545,6.217857289747,
12.1016506682281),.UNSPECIFIED.);
#53=B_SPLINE_SURFACE_WITH_KNOTS('',3,3,((#51211,#51212,#51213,#51214,#51215),
(#51216,#51217,#51218,#51219,#51220),(#51221,#51222,#51223,#51224,#51225),
(#51226,#51227,#51228,#51229,#51230),(#51231,#51232,#51233,#51234,#51235),
(#51236,#51237,#51238,#51239,#51240),(#51241,#51242,#51243,#51244,#51245)),
 .UNSPECIFIED.,.F.,.F.,.F.,(4,1,1,1,4),(4,1,4),(0.03064179013217,0.25,0.5,
0.75,0.997371574162),(0.1621509986021,6.217857289747,12.27408153315),
 .UNSPECIFIED.);
#54=ELLIPSE('',#25490,14.1459545202442,4.90175276915756);
#55=ELLIPSE('',#25504,38.974702057433,37.2141854840257);
#56=ELLIPSE('',#25512,14.1454026092901,4.90137019917901);
#57=ELLIPSE('',#25526,38.9778279365771,37.2201555784017);
#58=ELLIPSE('',#25534,14.1449420010391,4.90105113596068);
#59=ELLIPSE('',#25548,38.975599782719,37.215899615947);
#60=ELLIPSE('',#25556,14.1449570638359,4.90106151145033);
#61=ELLIPSE('',#25570,38.9740482939914,37.2129370257381);
#62=ELLIPSE('',#25579,14.14611930392,4.90186695347628);
#63=ELLIPSE('',#25593,14.1445653378396,4.90078996091196);
#64=ELLIPSE('',#25607,38.9767662731696,37.2181280215083);
#65=ELLIPSE('',#25633,38.97568443858,37.2160612851944);
#66=ELLIPSE('',#25719,40.0000000130718,20.0000000134373);
#67=ELLIPSE('',#25720,39.9999999264935,19.999999930827);
#68=ELLIPSE('',#25721,39.9999999974836,19.9999999977429);
#69=ELLIPSE('',#25722,40.0000000047116,20.0000000045204);
#70=ELLIPSE('',#25723,23.3867968076182,20.);
#71=ELLIPSE('',#25724,23.386796807644,20.);
#72=ELLIPSE('',#25728,24.1243589702644,20.);
#73=ELLIPSE('',#25729,24.124358970134,20.);
#74=ELLIPSE('',#25730,39.999999976902,19.9999999789991);
#75=ELLIPSE('',#25731,40.0000000049323,20.0000000047275);
#76=ELLIPSE('',#25732,39.9999999975502,19.999999997805);
#77=ELLIPSE('',#25733,39.9999999389236,19.9999999427079);
#78=ELLIPSE('',#25748,22.8021268874529,19.5);
#79=ELLIPSE('',#25751,22.8021268874277,19.5);
#80=ELLIPSE('',#25754,23.5212499960078,19.5);
#81=ELLIPSE('',#25764,23.5212499958807,19.5);
#82=ELLIPSE('',#25767,39.0000000024375,19.500000002367);
#83=ELLIPSE('',#25768,39.0000000667235,19.500000064201);
#84=ELLIPSE('',#25769,38.9999999995571,19.5000000004649);
#85=ELLIPSE('',#25770,38.999999996593,19.4999999968888);
#86=ELLIPSE('',#25779,38.9999999955418,19.4999999959037);
#87=ELLIPSE('',#25781,38.999999997527,19.4999999977637);
#88=ELLIPSE('',#25784,39.0000000253793,19.5000000249782);
#89=ELLIPSE('',#25786,39.0000000418424,19.5000000405918);
#90=ELLIPSE('',#25887,40.0000000130718,20.0000000134373);
#91=ELLIPSE('',#25888,39.9999999264935,19.999999930827);
#92=ELLIPSE('',#25889,39.9999999974836,19.9999999977429);
#93=ELLIPSE('',#25890,40.0000000047116,20.0000000045204);
#94=ELLIPSE('',#25891,23.3867968076182,20.);
#95=ELLIPSE('',#25892,23.386796807644,20.);
#96=ELLIPSE('',#25896,24.1243589702644,20.);
#97=ELLIPSE('',#25897,24.124358970134,20.);
#98=ELLIPSE('',#25898,39.999999976902,19.9999999789991);
#99=ELLIPSE('',#25899,40.0000000049323,20.0000000047275);
#100=ELLIPSE('',#25900,39.9999999975502,19.999999997805);
#101=ELLIPSE('',#25901,39.9999999389236,19.9999999427079);
#102=ELLIPSE('',#25916,22.8021268874529,19.5);
#103=ELLIPSE('',#25919,22.8021268874277,19.5);
#104=ELLIPSE('',#25922,23.5212499960078,19.5);
#105=ELLIPSE('',#25932,23.5212499958807,19.5);
#106=ELLIPSE('',#25935,39.0000000024375,19.500000002367);
#107=ELLIPSE('',#25936,39.0000000667235,19.500000064201);
#108=ELLIPSE('',#25937,38.9999999995571,19.5000000004649);
#109=ELLIPSE('',#25938,38.999999996593,19.4999999968888);
#110=ELLIPSE('',#25947,38.9999999955418,19.4999999959037);
#111=ELLIPSE('',#25949,38.999999997527,19.4999999977637);
#112=ELLIPSE('',#25952,39.0000000253793,19.5000000249782);
#113=ELLIPSE('',#25954,39.0000000418424,19.5000000405918);
#114=ELLIPSE('',#26276,4.9497474883957,3.50000001766466);
#115=ELLIPSE('',#26278,4.94974741758553,3.49999995496242);
#116=ELLIPSE('',#26282,4.94974750818554,3.50000003555096);
#117=ELLIPSE('',#26284,4.94974744933131,3.49999998268176);
#118=ELLIPSE('',#26290,4.94974743847195,3.49999997330407);
#119=ELLIPSE('',#26292,4.94974746764793,3.49999999946363);
#120=ELLIPSE('',#26296,4.94974747154346,3.5000000033075);
#121=ELLIPSE('',#26298,4.94974753359465,3.50000005774664);
#122=ELLIPSE('',#26304,4.94974746728535,3.49999999928767);
#123=ELLIPSE('',#26306,4.94974746000982,3.49999999272862);
#124=ELLIPSE('',#26310,4.94974744948699,3.49999998336686);
#125=ELLIPSE('',#26312,4.9497474011199,3.49999994011925);
#126=ELLIPSE('',#26318,4.94974750261449,3.50000003056212);
#127=ELLIPSE('',#26320,4.94974746233448,3.49999999488305);
#128=ELLIPSE('',#26324,4.94974747444535,3.50000000488897);
#129=ELLIPSE('',#26326,4.94974745285853,3.49999998629991);
#130=ELLIPSE('',#26332,4.94974749221039,3.50000002143459);
#131=ELLIPSE('',#26334,4.9497474654289,3.49999999744574);
#132=ELLIPSE('',#26338,4.94974747038,3.50000000169763);
#133=ELLIPSE('',#26340,4.94974743335947,3.49999996885897);
#134=ELLIPSE('',#26346,4.94974746422059,3.499999996325);
#135=ELLIPSE('',#26348,4.94974747922217,3.50000000966916);
#136=ELLIPSE('',#26352,4.94974747015525,3.50000000157014);
#137=ELLIPSE('',#26354,4.94974745455791,3.49999998774097);
#138=ELLIPSE('',#26360,4.94974745967519,3.49999999228821);
#139=ELLIPSE('',#26362,4.94974747586437,3.5000000067607);
#140=ELLIPSE('',#26366,4.94974746928504,3.50000000078832);
#141=ELLIPSE('',#26368,4.94974746799383,3.4999999996985);
#142=ELLIPSE('',#26374,4.94974746841778,3.50000000010074);
#143=ELLIPSE('',#26376,4.94974746853704,3.50000000020677);
#144=ELLIPSE('',#26380,4.94974746848257,3.50000000010871);
#145=ELLIPSE('',#26382,4.94974746829098,3.50000000002092);
#146=ELLIPSE('',#26558,6.97960018289555,5.49999999999817);
#147=ELLIPSE('',#26560,6.97960018289945,5.50000000000025);
#148=ELLIPSE('',#26561,6.97960018289465,5.49999999999756);
#149=ELLIPSE('',#26563,6.97960018289959,5.50000000000032);
#150=ELLIPSE('',#26564,6.97960018289765,5.49999999999922);
#151=ELLIPSE('',#26566,6.9796001828989,5.49999999999987);
#152=ELLIPSE('',#26887,21.2503681783598,5.50000000000001);
#153=ELLIPSE('',#26888,21.2503681783597,5.5);
#154=ELLIPSE('',#26893,21.2503681783597,5.5);
#155=ELLIPSE('',#26898,21.2503681783597,5.5);
#156=ELLIPSE('',#26900,21.2503681783597,5.49999999999999);
#157=ELLIPSE('',#26901,21.2503681783597,5.5);
#158=ELLIPSE('',#26994,21.2503681783598,5.50000000000001);
#159=ELLIPSE('',#26996,21.2503681783597,5.49999999999999);
#160=ELLIPSE('',#27001,6.97960018290351,5.50000000000224);
#161=ELLIPSE('',#27006,6.97960018290198,5.50000000000146);
#162=(
BOUNDED_SURFACE()
B_SPLINE_SURFACE(3,3,((#36423,#36424,#36425,#36426,#36427,#36428,#36429,
#36430,#36431,#36432),(#36433,#36434,#36435,#36436,#36437,#36438,#36439,
#36440,#36441,#36442),(#36443,#36444,#36445,#36446,#36447,#36448,#36449,
#36450,#36451,#36452),(#36453,#36454,#36455,#36456,#36457,#36458,#36459,
#36460,#36461,#36462)),.UNSPECIFIED.,.F.,.F.,.F.)
B_SPLINE_SURFACE_WITH_KNOTS((4,4),(4,1,1,1,1,1,1,4),(0.0902477597713112,
0.904395368827396),(0.02358777781772,0.1427066556452,0.2856868894759,0.4285070295258,
0.571316470583,0.7141880571253,0.8571205016359,0.9886565450754),
 .UNSPECIFIED.)
GEOMETRIC_REPRESENTATION_ITEM()
RATIONAL_B_SPLINE_SURFACE(((1.11546174586943,1.11546174586943,1.11546174586943,
1.11546174586943,1.11546174586943,1.11546174586943,1.11546174586943,1.11546174586943,
1.11546174586943,1.11546174586943),(0.962519072862034,0.962519072862034,
0.962519072862034,0.962519072862034,0.962519072862034,0.962519072862034,
0.962519072862034,0.962519072862034,0.962519072862034,0.962519072862034),
(0.96151932941876,0.96151932941876,0.96151932941876,0.96151932941876,0.96151932941876,
0.96151932941876,0.96151932941876,0.96151932941876,0.96151932941876,0.96151932941876),
(1.1124625155396,1.1124625155396,1.1124625155396,1.1124625155396,1.1124625155396,
1.1124625155396,1.1124625155396,1.1124625155396,1.1124625155396,1.1124625155396)))
REPRESENTATION_ITEM('')
SURFACE()
);
#163=(
BOUNDED_SURFACE()
B_SPLINE_SURFACE(3,3,((#36555,#36556,#36557,#36558,#36559,#36560,#36561,
#36562,#36563),(#36564,#36565,#36566,#36567,#36568,#36569,#36570,#36571,
#36572),(#36573,#36574,#36575,#36576,#36577,#36578,#36579,#36580,#36581),
(#36582,#36583,#36584,#36585,#36586,#36587,#36588,#36589,#36590)),
 .UNSPECIFIED.,.F.,.F.,.F.)
B_SPLINE_SURFACE_WITH_KNOTS((4,4),(4,1,1,1,1,1,4),(0.0546212561079652,0.945380228523745),
(0.228750194394892,0.3042889925712,0.4133392424319,0.5264696341084,0.6424947869233,
0.7601009691825,0.774320140471063),.UNSPECIFIED.)
GEOMETRIC_REPRESENTATION_ITEM()
RATIONAL_B_SPLINE_SURFACE(((1.19596662858113,1.19596662858113,1.19596662858113,
1.19596662858113,1.19596662858113,1.19596662858113,1.19596662858113,1.19596662858113,
1.19596662858113),(0.934677354980995,0.934677354980995,0.934677354980995,
0.934677354980995,0.934677354980995,0.934677354980995,0.934677354980995,
0.934677354980995,0.934677354980995),(0.934677790473648,0.934677790473648,
0.934677790473648,0.934677790473648,0.934677790473648,0.934677790473648,
0.934677790473648,0.934677790473648,0.934677790473648),(1.19596793505909,
1.19596793505909,1.19596793505909,1.19596793505909,1.19596793505909,1.19596793505909,
1.19596793505909,1.19596793505909,1.19596793505909)))
REPRESENTATION_ITEM('')
SURFACE()
);
#164=(
BOUNDED_SURFACE()
B_SPLINE_SURFACE(3,3,((#36641,#36642,#36643,#36644,#36645,#36646,#36647,
#36648,#36649),(#36650,#36651,#36652,#36653,#36654,#36655,#36656,#36657,
#36658),(#36659,#36660,#36661,#36662,#36663,#36664,#36665,#36666,#36667),
(#36668,#36669,#36670,#36671,#36672,#36673,#36674,#36675,#36676)),
 .UNSPECIFIED.,.F.,.F.,.F.)
B_SPLINE_SURFACE_WITH_KNOTS((4,4),(4,1,1,1,1,1,4),(0.0545959214790058,0.945405071292651),
(0.226579922118566,0.3006458185639,0.4098657082077,0.5233967602133,0.640305105005,
0.7591301880899,0.772969164981535),.UNSPECIFIED.)
GEOMETRIC_REPRESENTATION_ITEM()
RATIONAL_B_SPLINE_SURFACE(((1.19598782351354,1.19598782351354,1.19598782351354,
1.19598782351354,1.19598782351354,1.19598782351354,1.19598782351354,1.19598782351354,
1.19598782351354),(0.934670434267463,0.934670434267463,0.934670434267463,
0.934670434267463,0.934670434267463,0.934670434267463,0.934670434267463,
0.934670434267463,0.934670434267463),(0.93467072549571,0.93467072549571,
0.93467072549571,0.93467072549571,0.93467072549571,0.93467072549571,0.93467072549571,
0.93467072549571,0.93467072549571),(1.19598869719828,1.19598869719828,1.19598869719828,
1.19598869719828,1.19598869719828,1.19598869719828,1.19598869719828,1.19598869719828,
1.19598869719828)))
REPRESENTATION_ITEM('')
SURFACE()
);
#165=(
BOUNDED_SURFACE()
B_SPLINE_SURFACE(3,3,((#36787,#36788,#36789,#36790,#36791,#36792,#36793,
#36794,#36795,#36796,#36797),(#36798,#36799,#36800,#36801,#36802,#36803,
#36804,#36805,#36806,#36807,#36808),(#36809,#36810,#36811,#36812,#36813,
#36814,#36815,#36816,#36817,#36818,#36819),(#36820,#36821,#36822,#36823,
#36824,#36825,#36826,#36827,#36828,#36829,#36830)),.UNSPECIFIED.,.F.,.F.,
 .F.)
B_SPLINE_SURFACE_WITH_KNOTS((4,4),(4,1,1,1,1,1,1,1,4),(0.0753633924341077,
0.903558847349357),(-0.009670337421386,0.,0.1430991485311,0.2858285059199,
0.4284781713031,0.5715215149008,0.7145472299923,0.8573672624017,0.9759160460961),
 .UNSPECIFIED.)
GEOMETRIC_REPRESENTATION_ITEM()
RATIONAL_B_SPLINE_SURFACE(((1.12354604895393,1.12354604895393,1.12354604895393,
1.12354604895393,1.12354604895393,1.12354604895393,1.12354604895393,1.12354604895393,
1.12354604895393,1.12354604895393,1.12354604895393),(0.962906301315212,
0.962906301315212,0.962906301315212,0.962906301315212,0.962906301315212,
0.962906301315212,0.962906301315212,0.962906301315212,0.962906301315212,
0.962906301315212,0.962906301315212),(0.958919449944363,0.958919449944363,
0.958919449944363,0.958919449944363,0.958919449944363,0.958919449944363,
0.958919449944363,0.958919449944363,0.958919449944363,0.958919449944363,
0.958919449944363),(1.11158549484138,1.11158549484138,1.11158549484138,
1.11158549484138,1.11158549484138,1.11158549484138,1.11158549484138,1.11158549484138,
1.11158549484138,1.11158549484138,1.11158549484138)))
REPRESENTATION_ITEM('')
SURFACE()
);
#166=(
BOUNDED_SURFACE()
B_SPLINE_SURFACE(3,3,((#36947,#36948,#36949,#36950),(#36951,#36952,#36953,
#36954),(#36955,#36956,#36957,#36958),(#36959,#36960,#36961,#36962)),
 .UNSPECIFIED.,.F.,.F.,.F.)
B_SPLINE_SURFACE_WITH_KNOTS((4,4),(4,4),(0.0986320320063612,0.901362552769513),
(-0.975145040413366,-0.0991746183846591),.UNSPECIFIED.)
GEOMETRIC_REPRESENTATION_ITEM()
RATIONAL_B_SPLINE_SURFACE(((1.17563600435392,1.17563600435392,1.17563600435392,
1.17563600435392),(0.941456244993259,0.941456244993259,0.941456244993259,
0.941456244993259),(0.941454665226083,0.941454665226083,0.941454665226083,
0.941454665226083),(1.17563126505239,1.17563126505239,1.17563126505239,
1.17563126505239)))
REPRESENTATION_ITEM('')
SURFACE()
);
#167=(
BOUNDED_SURFACE()
B_SPLINE_SURFACE(3,3,((#36981,#36982,#36983,#36984,#36985,#36986,#36987,
#36988,#36989,#36990,#36991,#36992,#36993,#36994,#36995,#36996,#36997,#36998,
#36999,#37000,#37001,#37002,#37003,#37004,#37005,#37006,#37007,#37008,#37009,
#37010,#37011,#37012,#37013),(#37014,#37015,#37016,#37017,#37018,#37019,
#37020,#37021,#37022,#37023,#37024,#37025,#37026,#37027,#37028,#37029,#37030,
#37031,#37032,#37033,#37034,#37035,#37036,#37037,#37038,#37039,#37040,#37041,
#37042,#37043,#37044,#37045,#37046),(#37047,#37048,#37049,#37050,#37051,
#37052,#37053,#37054,#37055,#37056,#37057,#37058,#37059,#37060,#37061,#37062,
#37063,#37064,#37065,#37066,#37067,#37068,#37069,#37070,#37071,#37072,#37073,
#37074,#37075,#37076,#37077,#37078,#37079),(#37080,#37081,#37082,#37083,
#37084,#37085,#37086,#37087,#37088,#37089,#37090,#37091,#37092,#37093,#37094,
#37095,#37096,#37097,#37098,#37099,#37100,#37101,#37102,#37103,#37104,#37105,
#37106,#37107,#37108,#37109,#37110,#37111,#37112)),.UNSPECIFIED.,.F.,.F.,
 .F.)
B_SPLINE_SURFACE_WITH_KNOTS((4,4),(4,1,1,1,1,1,1,1,1,1,1,1,1,1,1,1,1,1,
1,1,1,1,1,1,1,1,1,1,1,1,4),(0.10838765227344,0.903585982727356),(-0.009736901738826,
0.,0.02218340749156,0.04656850383685,0.07320121634793,0.1023238311649,0.1343066238742,
0.1695984990871,0.2086121558937,0.2515303853623,0.2985746389689,0.3503366286804,
0.4076785718738,0.4682255700465,0.5282360307704,0.5849839255388,0.6367806003914,
0.6825368401892,0.7235074075059,0.7605068126506,0.7940285468273,0.8241776680761,
0.851065051828,0.8750212083666,0.8964625051056,0.9157946807006,0.9333731860455,
0.9493575699015,0.9638584550806,0.977054470158,0.9857155005173),
 .UNSPECIFIED.)
GEOMETRIC_REPRESENTATION_ITEM()
RATIONAL_B_SPLINE_SURFACE(((1.07414161106601,1.07414161106601,1.07414161106601,
1.07414161106601,1.07414161106601,1.07414161106601,1.07414161106601,1.07414161106601,
1.07414161106601,1.07414161106601,1.07414161106601,1.07414161106601,1.07414161106601,
1.07414161106601,1.07414161106601,1.07414161106601,1.07414161106601,1.07414161106601,
1.07414161106601,1.07414161106601,1.07414161106601,1.07414161106601,1.07414161106601,
1.07414161106601,1.07414161106601,1.07414161106601,1.07414161106601,1.07414161106601,
1.07414161106601,1.07414161106601,1.07414161106601,1.07414161106601,1.07414161106601),
(0.973774865432272,0.973774865432272,0.973774865432272,0.973774865432272,
0.973774865432272,0.973774865432272,0.973774865432272,0.973774865432272,
0.973774865432272,0.973774865432272,0.973774865432272,0.973774865432272,
0.973774865432272,0.973774865432272,0.973774865432272,0.973774865432272,
0.973774865432272,0.973774865432272,0.973774865432272,0.973774865432272,
0.973774865432272,0.973774865432272,0.973774865432272,0.973774865432272,
0.973774865432272,0.973774865432272,0.973774865432272,0.973774865432272,
0.973774865432272,0.973774865432272,0.973774865432272,0.973774865432272,
0.973774865432272),(0.975309233264917,0.975309233264917,0.975309233264917,
0.975309233264917,0.975309233264917,0.975309233264917,0.975309233264917,
0.975309233264917,0.975309233264917,0.975309233264917,0.975309233264917,
0.975309233264917,0.975309233264917,0.975309233264917,0.975309233264917,
0.975309233264917,0.975309233264917,0.975309233264917,0.975309233264917,
0.975309233264917,0.975309233264917,0.975309233264917,0.975309233264917,
0.975309233264917,0.975309233264917,0.975309233264917,0.975309233264917,
0.975309233264917,0.975309233264917,0.975309233264917,0.975309233264917,
0.975309233264917,0.975309233264917),(1.07874471456394,1.07874471456394,
1.07874471456394,1.07874471456394,1.07874471456394,1.07874471456394,1.07874471456394,
1.07874471456394,1.07874471456394,1.07874471456394,1.07874471456394,1.07874471456394,
1.07874471456394,1.07874471456394,1.07874471456394,1.07874471456394,1.07874471456394,
1.07874471456394,1.07874471456394,1.07874471456394,1.07874471456394,1.07874471456394,
1.07874471456394,1.07874471456394,1.07874471456394,1.07874471456394,1.07874471456394,
1.07874471456394,1.07874471456394,1.07874471456394,1.07874471456394,1.07874471456394,
1.07874471456394)))
REPRESENTATION_ITEM('')
SURFACE()
);
#168=(
BOUNDED_SURFACE()
B_SPLINE_SURFACE(3,3,((#37499,#37500,#37501,#37502,#37503,#37504,#37505,
#37506,#37507,#37508),(#37509,#37510,#37511,#37512,#37513,#37514,#37515,
#37516,#37517,#37518),(#37519,#37520,#37521,#37522,#37523,#37524,#37525,
#37526,#37527,#37528),(#37529,#37530,#37531,#37532,#37533,#37534,#37535,
#37536,#37537,#37538)),.UNSPECIFIED.,.F.,.F.,.F.)
B_SPLINE_SURFACE_WITH_KNOTS((4,4),(4,1,1,1,1,1,1,4),(0.0573940888734465,
0.942594572239928),(0.2949017622243,0.3477745082592,0.410039088065,0.4702670303195,
0.5296668592001,0.589892029113,0.6521532381952,0.7051388515263),
 .UNSPECIFIED.)
GEOMETRIC_REPRESENTATION_ITEM()
RATIONAL_B_SPLINE_SURFACE(((1.19352947582456,1.19352947582456,1.19352947582456,
1.19352947582456,1.19352947582456,1.19352947582456,1.19352947582456,1.19352947582456,
1.19352947582456,1.19352947582456),(0.935493480011236,0.935493480011236,
0.935493480011236,0.935493480011236,0.935493480011236,0.935493480011236,
0.935493480011236,0.935493480011236,0.935493480011236,0.935493480011236),
(0.935490174767419,0.935490174767419,0.935490174767419,0.935490174767419,
0.935490174767419,0.935490174767419,0.935490174767419,0.935490174767419,
0.935490174767419,0.935490174767419),(1.19351956009311,1.19351956009311,
1.19351956009311,1.19351956009311,1.19351956009311,1.19351956009311,1.19351956009311,
1.19351956009311,1.19351956009311,1.19351956009311)))
REPRESENTATION_ITEM('')
SURFACE()
);
#169=(
BOUNDED_SURFACE()
B_SPLINE_SURFACE(3,3,((#37638,#37639,#37640,#37641,#37642,#37643,#37644,
#37645,#37646),(#37647,#37648,#37649,#37650,#37651,#37652,#37653,#37654,
#37655),(#37656,#37657,#37658,#37659,#37660,#37661,#37662,#37663,#37664),
(#37665,#37666,#37667,#37668,#37669,#37670,#37671,#37672,#37673)),
 .UNSPECIFIED.,.F.,.F.,.F.)
B_SPLINE_SURFACE_WITH_KNOTS((4,4),(4,1,1,1,1,1,4),(0.0546805339304302,0.945320968231971),
(0.225741042054691,0.2411747389776,0.3599582619163,0.4768206617319,0.5903023688695,
0.6994747309877,0.773101800008629),.UNSPECIFIED.)
GEOMETRIC_REPRESENTATION_ITEM()
RATIONAL_B_SPLINE_SURFACE(((1.19591424064832,1.19591424064832,1.19591424064832,
1.19591424064832,1.19591424064832,1.19591424064832,1.19591424064832,1.19591424064832,
1.19591424064832),(0.934694812542253,0.934694812542253,0.934694812542253,
0.934694812542253,0.934694812542253,0.934694812542253,0.934694812542253,
0.934694812542253,0.934694812542253),(0.934695253118102,0.934695253118102,
0.934695253118102,0.934695253118102,0.934695253118102,0.934695253118102,
0.934695253118102,0.934695253118102,0.934695253118102),(1.19591556237587,
1.19591556237587,1.19591556237587,1.19591556237587,1.19591556237587,1.19591556237587,
1.19591556237587,1.19591556237587,1.19591556237587)))
REPRESENTATION_ITEM('')
SURFACE()
);
#170=(
BOUNDED_SURFACE()
B_SPLINE_SURFACE(3,3,((#37790,#37791,#37792,#37793,#37794,#37795,#37796,
#37797,#37798,#37799),(#37800,#37801,#37802,#37803,#37804,#37805,#37806,
#37807,#37808,#37809),(#37810,#37811,#37812,#37813,#37814,#37815,#37816,
#37817,#37818,#37819),(#37820,#37821,#37822,#37823,#37824,#37825,#37826,
#37827,#37828,#37829)),.UNSPECIFIED.,.F.,.F.,.F.)
B_SPLINE_SURFACE_WITH_KNOTS((4,4),(4,1,1,1,1,1,1,4),(0.0902148383069544,
0.903852967096121),(0.01134228752749,0.1428795013597,0.2858119516079,0.4286835332756,
0.5714929665995,0.7143131101565,0.8572933444563,0.9764111906646),
 .UNSPECIFIED.)
GEOMETRIC_REPRESENTATION_ITEM()
RATIONAL_B_SPLINE_SURFACE(((1.11548029903383,1.11548029903383,1.11548029903383,
1.11548029903383,1.11548029903383,1.11548029903383,1.11548029903383,1.11548029903383,
1.11548029903383,1.11548029903383),(0.962621056026685,0.962621056026685,
0.962621056026685,0.962621056026685,0.962621056026685,0.962621056026685,
0.962621056026685,0.962621056026685,0.962621056026685,0.962621056026685),
(0.961514633856943,0.961514633856943,0.961514633856943,0.961514633856943,
0.961514633856943,0.961514633856943,0.961514633856943,0.961514633856943,
0.961514633856943,0.961514633856943),(1.1121610325246,1.1121610325246,1.1121610325246,
1.1121610325246,1.1121610325246,1.1121610325246,1.1121610325246,1.1121610325246,
1.1121610325246,1.1121610325246)))
REPRESENTATION_ITEM('')
SURFACE()
);
#171=(
BOUNDED_SURFACE()
B_SPLINE_SURFACE(3,3,((#37856,#37857,#37858,#37859,#37860,#37861,#37862,
#37863,#37864),(#37865,#37866,#37867,#37868,#37869,#37870,#37871,#37872,
#37873),(#37874,#37875,#37876,#37877,#37878,#37879,#37880,#37881,#37882),
(#37883,#37884,#37885,#37886,#37887,#37888,#37889,#37890,#37891)),
 .UNSPECIFIED.,.F.,.F.,.F.)
B_SPLINE_SURFACE_WITH_KNOTS((4,4),(4,1,1,1,1,1,4),(0.0546950340476835,0.945306466434247),
(0.226871363787984,0.3005222549961,0.4096933649143,0.5231718563143,0.6400288266084,
0.7588043312261,0.774243594722914),.UNSPECIFIED.)
GEOMETRIC_REPRESENTATION_ITEM()
RATIONAL_B_SPLINE_SURFACE(((1.19590147953157,1.19590147953157,1.19590147953157,
1.19590147953157,1.19590147953157,1.19590147953157,1.19590147953157,1.19590147953157,
1.19590147953157),(0.934699066754979,0.934699066754979,0.934699066754979,
0.934699066754979,0.934699066754979,0.934699066754979,0.934699066754979,
0.934699066754979,0.934699066754979),(0.934699506823618,0.934699506823618,
0.934699506823618,0.934699506823618,0.934699506823618,0.934699506823618,
0.934699506823618,0.934699506823618,0.934699506823618),(1.19590279973749,
1.19590279973749,1.19590279973749,1.19590279973749,1.19590279973749,1.19590279973749,
1.19590279973749,1.19590279973749,1.19590279973749)))
REPRESENTATION_ITEM('')
SURFACE()
);
#172=(
BOUNDED_SURFACE()
B_SPLINE_SURFACE(3,3,((#38005,#38006,#38007,#38008,#38009,#38010,#38011,
#38012,#38013,#38014),(#38015,#38016,#38017,#38018,#38019,#38020,#38021,
#38022,#38023,#38024),(#38025,#38026,#38027,#38028,#38029,#38030,#38031,
#38032,#38033,#38034),(#38035,#38036,#38037,#38038,#38039,#38040,#38041,
#38042,#38043,#38044)),.UNSPECIFIED.,.F.,.F.,.F.)
B_SPLINE_SURFACE_WITH_KNOTS((4,4),(4,1,1,1,1,1,1,4),(0.0902464241409013,
0.90385943340213),(0.02358777781733,0.1427066555246,0.2856868899129,0.4285070341315,
0.5713164659964,0.7141880467444,0.8571204980751,0.9886565450756),
 .UNSPECIFIED.)
GEOMETRIC_REPRESENTATION_ITEM()
RATIONAL_B_SPLINE_SURFACE(((1.115462498594,1.115462498594,1.115462498594,
1.115462498594,1.115462498594,1.115462498594,1.115462498594,1.115462498594,
1.115462498594,1.115462498594),(0.962619755259846,0.962619755259846,0.962619755259846,
0.962619755259846,0.962619755259846,0.962619755259846,0.962619755259846,
0.962619755259846,0.962619755259846,0.962619755259846),(0.961520464178815,
0.961520464178815,0.961520464178815,0.961520464178815,0.961520464178815,
0.961520464178815,0.961520464178815,0.961520464178815,0.961520464178815,
0.961520464178815),(1.11216462535091,1.11216462535091,1.11216462535091,
1.11216462535091,1.11216462535091,1.11216462535091,1.11216462535091,1.11216462535091,
1.11216462535091,1.11216462535091)))
REPRESENTATION_ITEM('')
SURFACE()
);
#173=(
BOUNDED_SURFACE()
B_SPLINE_SURFACE(3,3,((#38084,#38085,#38086,#38087,#38088,#38089),(#38090,
#38091,#38092,#38093,#38094,#38095),(#38096,#38097,#38098,#38099,#38100,
#38101),(#38102,#38103,#38104,#38105,#38106,#38107)),.UNSPECIFIED.,.F.,
 .F.,.F.)
B_SPLINE_SURFACE_WITH_KNOTS((4,4),(4,1,1,4),(0.098634219138839,0.901369959992847),
(0.317543733196422,0.3333147448851,0.6666852551146,0.682456266811579),
 .UNSPECIFIED.)
GEOMETRIC_REPRESENTATION_ITEM()
RATIONAL_B_SPLINE_SURFACE(((1.17563408853202,1.17563408853202,1.17563408853202,
1.17563408853202,1.17563408853202,1.17563408853202),(0.941454084655573,
0.941454084655573,0.941454084655573,0.941454084655573,0.941454084655573,
0.941454084655573),(0.941455303829106,0.941455303829106,0.941455303829106,
0.941455303829106,0.941455303829106,0.941455303829106),(1.17563774605262,
1.17563774605262,1.17563774605262,1.17563774605262,1.17563774605262,1.17563774605262)))
REPRESENTATION_ITEM('')
SURFACE()
);
#174=(
BOUNDED_SURFACE()
B_SPLINE_SURFACE(3,3,((#38347,#38348,#38349,#38350,#38351,#38352,#38353,
#38354,#38355,#38356,#38357,#38358,#38359,#38360,#38361,#38362,#38363,#38364,
#38365,#38366,#38367,#38368,#38369,#38370,#38371,#38372,#38373,#38374,#38375,
#38376,#38377,#38378,#38379,#38380,#38381,#38382,#38383,#38384,#38385,#38386),
(#38387,#38388,#38389,#38390,#38391,#38392,#38393,#38394,#38395,#38396,
#38397,#38398,#38399,#38400,#38401,#38402,#38403,#38404,#38405,#38406,#38407,
#38408,#38409,#38410,#38411,#38412,#38413,#38414,#38415,#38416,#38417,#38418,
#38419,#38420,#38421,#38422,#38423,#38424,#38425,#38426),(#38427,#38428,
#38429,#38430,#38431,#38432,#38433,#38434,#38435,#38436,#38437,#38438,#38439,
#38440,#38441,#38442,#38443,#38444,#38445,#38446,#38447,#38448,#38449,#38450,
#38451,#38452,#38453,#38454,#38455,#38456,#38457,#38458,#38459,#38460,#38461,
#38462,#38463,#38464,#38465,#38466),(#38467,#38468,#38469,#38470,#38471,
#38472,#38473,#38474,#38475,#38476,#38477,#38478,#38479,#38480,#38481,#38482,
#38483,#38484,#38485,#38486,#38487,#38488,#38489,#38490,#38491,#38492,#38493,
#38494,#38495,#38496,#38497,#38498,#38499,#38500,#38501,#38502,#38503,#38504,
#38505,#38506)),.UNSPECIFIED.,.F.,.F.,.F.)
B_SPLINE_SURFACE_WITH_KNOTS((4,4),(4,1,1,1,1,1,1,1,1,1,1,1,1,1,1,1,1,1,
1,1,1,1,1,1,1,1,1,1,1,1,1,1,1,1,1,1,1,4),(0.109557825387019,0.885251264327289),
(-0.009601789265351,0.,0.02232759876063,0.04690438428766,0.07379256313496,
0.1032821525101,0.1358145488914,0.1719130282251,0.2120212567552,0.2562571680377,
0.3048298949267,0.3584023231075,0.4161460884584,0.4734208057337,0.5265860543835,
0.5739192804757,0.6155188222739,0.652989783064,0.6871354795262,0.7180181889022,
0.7460302867732,0.7715243416789,0.7947371788944,0.8158355553748,0.8349846338442,
0.8523571535156,0.8681359777146,0.8825006466305,0.8956281837459,0.9076945427556,
0.918845104806,0.9291452127897,0.9386434680723,0.9473863882152,0.9554261628486,
0.9628162067307,0.9696068473728,0.972066289545),.UNSPECIFIED.)
GEOMETRIC_REPRESENTATION_ITEM()
RATIONAL_B_SPLINE_SURFACE(((1.07369782396742,1.07369782396742,1.07369782396742,
1.07369782396742,1.07369782396742,1.07369782396742,1.07369782396742,1.07369782396742,
1.07369782396742,1.07369782396742,1.07369782396742,1.07369782396742,1.07369782396742,
1.07369782396742,1.07369782396742,1.07369782396742,1.07369782396742,1.07369782396742,
1.07369782396742,1.07369782396742,1.07369782396742,1.07369782396742,1.07369782396742,
1.07369782396742,1.07369782396742,1.07369782396742,1.07369782396742,1.07369782396742,
1.07369782396742,1.07369782396742,1.07369782396742,1.07369782396742,1.07369782396742,
1.07369782396742,1.07369782396742,1.07369782396742,1.07369782396742,1.07369782396742,
1.07369782396742,1.07369782396742),(0.976087264738623,0.976087264738623,
0.976087264738623,0.976087264738623,0.976087264738623,0.976087264738623,
0.976087264738623,0.976087264738623,0.976087264738623,0.976087264738623,
0.976087264738623,0.976087264738623,0.976087264738623,0.976087264738623,
0.976087264738623,0.976087264738623,0.976087264738623,0.976087264738623,
0.976087264738623,0.976087264738623,0.976087264738623,0.976087264738623,
0.976087264738623,0.976087264738623,0.976087264738623,0.976087264738623,
0.976087264738623,0.976087264738623,0.976087264738623,0.976087264738623,
0.976087264738623,0.976087264738623,0.976087264738623,0.976087264738623,
0.976087264738623,0.976087264738623,0.976087264738623,0.976087264738623,
0.976087264738623,0.976087264738623),(0.975438400849373,0.975438400849373,
0.975438400849373,0.975438400849373,0.975438400849373,0.975438400849373,
0.975438400849373,0.975438400849373,0.975438400849373,0.975438400849373,
0.975438400849373,0.975438400849373,0.975438400849373,0.975438400849373,
0.975438400849373,0.975438400849373,0.975438400849373,0.975438400849373,
0.975438400849373,0.975438400849373,0.975438400849373,0.975438400849373,
0.975438400849373,0.975438400849373,0.975438400849373,0.975438400849373,
0.975438400849373,0.975438400849373,0.975438400849373,0.975438400849373,
0.975438400849373,0.975438400849373,0.975438400849373,0.975438400849373,
0.975438400849373,0.975438400849373,0.975438400849373,0.975438400849373,
0.975438400849373,0.975438400849373),(1.07175123229967,1.07175123229967,
1.07175123229967,1.07175123229967,1.07175123229967,1.07175123229967,1.07175123229967,
1.07175123229967,1.07175123229967,1.07175123229967,1.07175123229967,1.07175123229967,
1.07175123229967,1.07175123229967,1.07175123229967,1.07175123229967,1.07175123229967,
1.07175123229967,1.07175123229967,1.07175123229967,1.07175123229967,1.07175123229967,
1.07175123229967,1.07175123229967,1.07175123229967,1.07175123229967,1.07175123229967,
1.07175123229967,1.07175123229967,1.07175123229967,1.07175123229967,1.07175123229967,
1.07175123229967,1.07175123229967,1.07175123229967,1.07175123229967,1.07175123229967,
1.07175123229967,1.07175123229967,1.07175123229967)))
REPRESENTATION_ITEM('')
SURFACE()
);
#175=(
BOUNDED_SURFACE()
B_SPLINE_SURFACE(3,3,((#38632,#38633,#38634,#38635,#38636,#38637,#38638,
#38639,#38640),(#38641,#38642,#38643,#38644,#38645,#38646,#38647,#38648,
#38649),(#38650,#38651,#38652,#38653,#38654,#38655,#38656,#38657,#38658),
(#38659,#38660,#38661,#38662,#38663,#38664,#38665,#38666,#38667)),
 .UNSPECIFIED.,.F.,.F.,.F.)
B_SPLINE_SURFACE_WITH_KNOTS((4,4),(4,1,1,1,1,1,4),(0.0545575351232763,0.945444284135705),
(0.226990618484223,0.2408830109944,0.3597029788422,0.4766081773209,0.5901375306023,
0.6993568121791,0.773423227451189),.UNSPECIFIED.)
GEOMETRIC_REPRESENTATION_ITEM()
RATIONAL_B_SPLINE_SURFACE(((1.1960229215533,1.1960229215533,1.1960229215533,
1.1960229215533,1.1960229215533,1.1960229215533,1.1960229215533,1.1960229215533,
1.1960229215533),(0.934658492422782,0.934658492422782,0.934658492422782,
0.934658492422782,0.934658492422782,0.934658492422782,0.934658492422782,
0.934658492422782,0.934658492422782),(0.934659026150056,0.934659026150056,
0.934659026150056,0.934659026150056,0.934659026150056,0.934659026150056,
0.934659026150056,0.934659026150056,0.934659026150056),(1.19602452273512,
1.19602452273512,1.19602452273512,1.19602452273512,1.19602452273512,1.19602452273512,
1.19602452273512,1.19602452273512,1.19602452273512)))
REPRESENTATION_ITEM('')
SURFACE()
);
#176=(
BOUNDED_SURFACE()
B_SPLINE_SURFACE(3,3,((#38790,#38791,#38792,#38793,#38794,#38795,#38796,
#38797,#38798,#38799),(#38800,#38801,#38802,#38803,#38804,#38805,#38806,
#38807,#38808,#38809),(#38810,#38811,#38812,#38813,#38814,#38815,#38816,
#38817,#38818,#38819),(#38820,#38821,#38822,#38823,#38824,#38825,#38826,
#38827,#38828,#38829)),.UNSPECIFIED.,.F.,.F.,.F.)
B_SPLINE_SURFACE_WITH_KNOTS((4,4),(4,1,1,1,1,1,1,4),(0.089702696705292,
0.903562227825136),(0.02295305876099,0.1427319370604,0.2857219203474,0.4285792797614,
0.5713515650105,0.7142098207389,0.8572808214069,0.9622634165798),
 .UNSPECIFIED.)
GEOMETRIC_REPRESENTATION_ITEM()
RATIONAL_B_SPLINE_SURFACE(((1.11534309462385,1.11534309462385,1.11534309462385,
1.11534309462385,1.11534309462385,1.11534309462385,1.11534309462385,1.11534309462385,
1.11534309462385,1.11534309462385),(0.96281454820187,0.96281454820187,0.96281454820187,
0.96281454820187,0.96281454820187,0.96281454820187,0.96281454820187,0.96281454820187,
0.96281454820187,0.96281454820187),(0.961562661748843,0.961562661748843,
0.961562661748843,0.961562661748843,0.961562661748843,0.961562661748843,
0.961562661748843,0.961562661748843,0.961562661748843,0.961562661748843),
(1.11158743526477,1.11158743526477,1.11158743526477,1.11158743526477,1.11158743526477,
1.11158743526477,1.11158743526477,1.11158743526477,1.11158743526477,1.11158743526477)))
REPRESENTATION_ITEM('')
SURFACE()
);
#177=(
BOUNDED_SURFACE()
B_SPLINE_SURFACE(3,3,((#39048,#39049,#39050,#39051,#39052,#39053,#39054,
#39055,#39056,#39057),(#39058,#39059,#39060,#39061,#39062,#39063,#39064,
#39065,#39066,#39067),(#39068,#39069,#39070,#39071,#39072,#39073,#39074,
#39075,#39076,#39077),(#39078,#39079,#39080,#39081,#39082,#39083,#39084,
#39085,#39086,#39087)),.UNSPECIFIED.,.F.,.F.,.F.)
B_SPLINE_SURFACE_WITH_KNOTS((4,4),(4,1,1,1,1,1,1,4),(0.057320173478123,
0.942665361817278),(0.2948675792044,0.3465037559324,0.4092144664244,0.4700480650883,
0.529946403199,0.5907794942564,0.6534941325732,0.7051005237738),
 .UNSPECIFIED.)
GEOMETRIC_REPRESENTATION_ITEM()
RATIONAL_B_SPLINE_SURFACE(((1.19359440570704,1.19359440570704,1.19359440570704,
1.19359440570704,1.19359440570704,1.19359440570704,1.19359440570704,1.19359440570704,
1.19359440570704,1.19359440570704),(0.935472748603642,0.935472748603642,
0.935472748603642,0.935472748603642,0.935472748603642,0.935472748603642,
0.935472748603642,0.935472748603642,0.935472748603642,0.935472748603642),
(0.935468531499884,0.935468531499884,0.935468531499884,0.935468531499884,
0.935468531499884,0.935468531499884,0.935468531499884,0.935468531499884,
0.935468531499884,0.935468531499884),(1.19358175439577,1.19358175439577,
1.19358175439577,1.19358175439577,1.19358175439577,1.19358175439577,1.19358175439577,
1.19358175439577,1.19358175439577,1.19358175439577)))
REPRESENTATION_ITEM('')
SURFACE()
);
#178=(
BOUNDED_SURFACE()
B_SPLINE_SURFACE(3,3,((#39173,#39174,#39175,#39176,#39177,#39178,#39179,
#39180,#39181),(#39182,#39183,#39184,#39185,#39186,#39187,#39188,#39189,
#39190),(#39191,#39192,#39193,#39194,#39195,#39196,#39197,#39198,#39199),
(#39200,#39201,#39202,#39203,#39204,#39205,#39206,#39207,#39208)),
 .UNSPECIFIED.,.F.,.F.,.F.)
B_SPLINE_SURFACE_WITH_KNOTS((4,4),(4,1,1,1,1,1,4),(0.0545718989489667,0.945429093825032),
(0.226579922118891,0.300645818564,0.4098657082078,0.5233967602134,0.6403051050052,
0.7591301880902,0.77299234439195),.UNSPECIFIED.)
GEOMETRIC_REPRESENTATION_ITEM()
RATIONAL_B_SPLINE_SURFACE(((1.19600896499511,1.19600896499511,1.19600896499511,
1.19600896499511,1.19600896499511,1.19600896499511,1.19600896499511,1.19600896499511,
1.19600896499511),(0.934663387090781,0.934663387090781,0.934663387090781,
0.934663387090781,0.934663387090781,0.934663387090781,0.934663387090781,
0.934663387090781,0.934663387090781),(0.934663678335422,0.934663678335422,
0.934663678335422,0.934663678335422,0.934663678335422,0.934663678335422,
0.934663678335422,0.934663678335422,0.934663678335422),(1.19600983872903,
1.19600983872903,1.19600983872903,1.19600983872903,1.19600983872903,1.19600983872903,
1.19600983872903,1.19600983872903,1.19600983872903)))
REPRESENTATION_ITEM('')
SURFACE()
);
#179=(
BOUNDED_SURFACE()
B_SPLINE_SURFACE(3,3,((#39319,#39320,#39321,#39322,#39323,#39324,#39325,
#39326,#39327,#39328,#39329),(#39330,#39331,#39332,#39333,#39334,#39335,
#39336,#39337,#39338,#39339,#39340),(#39341,#39342,#39343,#39344,#39345,
#39346,#39347,#39348,#39349,#39350,#39351),(#39352,#39353,#39354,#39355,
#39356,#39357,#39358,#39359,#39360,#39361,#39362)),.UNSPECIFIED.,.F.,.F.,
 .F.)
B_SPLINE_SURFACE_WITH_KNOTS((4,4),(4,1,1,1,1,1,1,1,4),(0.0753633923116561,
0.903558734772718),(-0.009670337421385,0.,0.1430991485311,0.2858285059199,
0.4284781713031,0.5715215149008,0.7145472299923,0.8573672624017,0.9759160460961),
 .UNSPECIFIED.)
GEOMETRIC_REPRESENTATION_ITEM()
RATIONAL_B_SPLINE_SURFACE(((1.12354604900567,1.12354604900567,1.12354604900567,
1.12354604900567,1.12354604900567,1.12354604900567,1.12354604900567,1.12354604900567,
1.12354604900567,1.12354604900567,1.12354604900567),(0.962906323157822,
0.962906323157822,0.962906323157822,0.962906323157822,0.962906323157822,
0.962906323157822,0.962906323157822,0.962906323157822,0.962906323157822,
0.962906323157822,0.962906323157822),(0.958919451011949,0.958919451011949,
0.958919451011949,0.958919451011949,0.958919451011949,0.958919451011949,
0.958919451011949,0.958919451011949,0.958919451011949,0.958919451011949,
0.958919451011949),(1.11158543256805,1.11158543256805,1.11158543256805,
1.11158543256805,1.11158543256805,1.11158543256805,1.11158543256805,1.11158543256805,
1.11158543256805,1.11158543256805,1.11158543256805)))
REPRESENTATION_ITEM('')
SURFACE()
);
#180=(
BOUNDED_SURFACE()
B_SPLINE_SURFACE(3,3,((#39479,#39480,#39481,#39482),(#39483,#39484,#39485,
#39486),(#39487,#39488,#39489,#39490),(#39491,#39492,#39493,#39494)),
 .UNSPECIFIED.,.F.,.F.,.F.)
B_SPLINE_SURFACE_WITH_KNOTS((4,4),(4,4),(0.0986320319987802,0.901362552767005),
(-0.975145040400083,-0.0991746183717141),.UNSPECIFIED.)
GEOMETRIC_REPRESENTATION_ITEM()
RATIONAL_B_SPLINE_SURFACE(((1.17563600436181,1.17563600436181,1.17563600436181,
1.17563600436181),(0.94145624499344,0.94145624499344,0.94145624499344,0.94145624499344),
(0.94145466522332,0.941454665223321,0.941454665223321,0.941454665223321),
(1.17563126505145,1.17563126505145,1.17563126505145,1.17563126505145)))
REPRESENTATION_ITEM('')
SURFACE()
);
#181=(
BOUNDED_SURFACE()
B_SPLINE_SURFACE(3,3,((#39513,#39514,#39515,#39516,#39517,#39518,#39519,
#39520,#39521,#39522,#39523,#39524,#39525,#39526,#39527,#39528,#39529,#39530,
#39531,#39532,#39533,#39534,#39535,#39536,#39537,#39538,#39539,#39540,#39541,
#39542,#39543,#39544,#39545),(#39546,#39547,#39548,#39549,#39550,#39551,
#39552,#39553,#39554,#39555,#39556,#39557,#39558,#39559,#39560,#39561,#39562,
#39563,#39564,#39565,#39566,#39567,#39568,#39569,#39570,#39571,#39572,#39573,
#39574,#39575,#39576,#39577,#39578),(#39579,#39580,#39581,#39582,#39583,
#39584,#39585,#39586,#39587,#39588,#39589,#39590,#39591,#39592,#39593,#39594,
#39595,#39596,#39597,#39598,#39599,#39600,#39601,#39602,#39603,#39604,#39605,
#39606,#39607,#39608,#39609,#39610,#39611),(#39612,#39613,#39614,#39615,
#39616,#39617,#39618,#39619,#39620,#39621,#39622,#39623,#39624,#39625,#39626,
#39627,#39628,#39629,#39630,#39631,#39632,#39633,#39634,#39635,#39636,#39637,
#39638,#39639,#39640,#39641,#39642,#39643,#39644)),.UNSPECIFIED.,.F.,.F.,
 .F.)
B_SPLINE_SURFACE_WITH_KNOTS((4,4),(4,1,1,1,1,1,1,1,1,1,1,1,1,1,1,1,1,1,
1,1,1,1,1,1,1,1,1,1,1,1,4),(0.108382715709703,0.903586121555296),(-0.009736901741271,
0.,0.02218380445754,0.04656911069387,0.07320179425856,0.1023242565949,0.134306834044,
0.1695984355629,0.2086117112192,0.2515292087379,0.2985721062314,0.3503319196398,
0.4076720811719,0.4682188084844,0.5282303398,0.5849800412443,0.6367784970474,
0.6825358730223,0.7235071660675,0.760507022248,0.7940289957981,0.8241782115926,
0.8510656102853,0.8750217369476,0.8964629740695,0.915795075343,0.9333734980491,
0.949357773524,0.9638585157197,0.9770543997027,0.9857155005215),
 .UNSPECIFIED.)
GEOMETRIC_REPRESENTATION_ITEM()
RATIONAL_B_SPLINE_SURFACE(((1.07414347861564,1.07414347861564,1.07414347861564,
1.07414347861564,1.07414347861564,1.07414347861564,1.07414347861564,1.07414347861564,
1.07414347861564,1.07414347861564,1.07414347861564,1.07414347861564,1.07414347861564,
1.07414347861564,1.07414347861564,1.07414347861564,1.07414347861564,1.07414347861564,
1.07414347861564,1.07414347861564,1.07414347861564,1.07414347861564,1.07414347861564,
1.07414347861564,1.07414347861564,1.07414347861564,1.07414347861564,1.07414347861564,
1.07414347861564,1.07414347861564,1.07414347861564,1.07414347861564,1.07414347861564),
(0.973774829458314,0.973774829458314,0.973774829458314,0.973774829458314,
0.973774829458314,0.973774829458314,0.973774829458314,0.973774829458314,
0.973774829458314,0.973774829458314,0.973774829458314,0.973774829458314,
0.973774829458314,0.973774829458314,0.973774829458314,0.973774829458314,
0.973774829458314,0.973774829458314,0.973774829458314,0.973774829458314,
0.973774829458314,0.973774829458314,0.973774829458314,0.973774829458314,
0.973774829458314,0.973774829458314,0.973774829458314,0.973774829458314,
0.973774829458314,0.973774829458314,0.973774829458314,0.973774829458314,
0.973774829458314),(0.975308592237003,0.975308592237003,0.975308592237003,
0.975308592237003,0.975308592237003,0.975308592237003,0.975308592237003,
0.975308592237003,0.975308592237003,0.975308592237003,0.975308592237003,
0.975308592237003,0.975308592237003,0.975308592237003,0.975308592237003,
0.975308592237003,0.975308592237003,0.975308592237003,0.975308592237003,
0.975308592237003,0.975308592237003,0.975308592237003,0.975308592237003,
0.975308592237003,0.975308592237003,0.975308592237003,0.975308592237003,
0.975308592237003,0.975308592237003,0.975308592237003,0.975308592237003,
0.975308592237003,0.975308592237003),(1.07874476695171,1.07874476695171,
1.07874476695171,1.07874476695171,1.07874476695171,1.07874476695171,1.07874476695171,
1.07874476695171,1.07874476695171,1.07874476695171,1.07874476695171,1.07874476695171,
1.07874476695171,1.07874476695171,1.07874476695171,1.07874476695171,1.07874476695171,
1.07874476695171,1.07874476695171,1.07874476695171,1.07874476695171,1.07874476695171,
1.07874476695171,1.07874476695171,1.07874476695171,1.07874476695171,1.07874476695171,
1.07874476695171,1.07874476695171,1.07874476695171,1.07874476695171,1.07874476695171,
1.07874476695171)))
REPRESENTATION_ITEM('')
SURFACE()
);
#182=(
BOUNDED_SURFACE()
B_SPLINE_SURFACE(3,3,((#40029,#40030,#40031,#40032,#40033,#40034,#40035,
#40036,#40037,#40038),(#40039,#40040,#40041,#40042,#40043,#40044,#40045,
#40046,#40047,#40048),(#40049,#40050,#40051,#40052,#40053,#40054,#40055,
#40056,#40057,#40058),(#40059,#40060,#40061,#40062,#40063,#40064,#40065,
#40066,#40067,#40068)),.UNSPECIFIED.,.F.,.F.,.F.)
B_SPLINE_SURFACE_WITH_KNOTS((4,4),(4,1,1,1,1,1,1,4),(0.0573683470670303,
0.942619239203189),(0.2949033483364,0.3467756743286,0.4093838918203,0.4700724725555,
0.5298509963668,0.5905363232075,0.6531416885286,0.7051372589503),
 .UNSPECIFIED.)
GEOMETRIC_REPRESENTATION_ITEM()
RATIONAL_B_SPLINE_SURFACE(((1.19355202165888,1.19355202165888,1.19355202165888,
1.19355202165888,1.19355202165888,1.19355202165888,1.19355202165888,1.19355202165888,
1.19355202165888,1.19355202165888),(0.935486278261233,0.935486278261233,
0.935486278261233,0.935486278261233,0.935486278261233,0.935486278261233,
0.935486278261233,0.935486278261233,0.935486278261233,0.935486278261233),
(0.935482659497885,0.935482659497885,0.935482659497885,0.935482659497885,
0.935482659497885,0.935482659497885,0.935482659497885,0.935482659497885,
0.935482659497885,0.935482659497885),(1.19354116536884,1.19354116536884,
1.19354116536884,1.19354116536884,1.19354116536884,1.19354116536884,1.19354116536884,
1.19354116536884,1.19354116536884,1.19354116536884)))
REPRESENTATION_ITEM('')
SURFACE()
);
#183=(
BOUNDED_SURFACE()
B_SPLINE_SURFACE(3,3,((#40177,#40178,#40179,#40180,#40181,#40182,#40183,
#40184,#40185),(#40186,#40187,#40188,#40189,#40190,#40191,#40192,#40193,
#40194),(#40195,#40196,#40197,#40198,#40199,#40200,#40201,#40202,#40203),
(#40204,#40205,#40206,#40207,#40208,#40209,#40210,#40211,#40212)),
 .UNSPECIFIED.,.F.,.F.,.F.)
B_SPLINE_SURFACE_WITH_KNOTS((4,4),(4,1,1,1,1,1,4),(0.054657385317252,0.945344116841943),
(0.225718740397496,0.2411747389778,0.3599582619165,0.4768206617321,0.5903023688696,
0.6994747309877,0.773103852050118),.UNSPECIFIED.)
GEOMETRIC_REPRESENTATION_ITEM()
RATIONAL_B_SPLINE_SURFACE(((1.19593460922364,1.19593460922364,1.19593460922364,
1.19593460922364,1.19593460922364,1.19593460922364,1.19593460922364,1.19593460922364,
1.19593460922364),(0.934688022994918,0.934688022994918,0.934688022994918,
0.934688022994918,0.934688022994918,0.934688022994918,0.934688022994918,
0.934688022994918,0.934688022994918),(0.934688463592728,0.934688463592728,
0.934688463592728,0.934688463592728,0.934688463592728,0.934688463592728,
0.934688463592728,0.934688463592728,0.934688463592728),(1.19593593101708,
1.19593593101708,1.19593593101708,1.19593593101708,1.19593593101708,1.19593593101708,
1.19593593101708,1.19593593101708,1.19593593101708)))
REPRESENTATION_ITEM('')
SURFACE()
);
#184=(
BOUNDED_SURFACE()
B_SPLINE_SURFACE(3,3,((#40329,#40330,#40331,#40332,#40333,#40334,#40335,
#40336,#40337,#40338),(#40339,#40340,#40341,#40342,#40343,#40344,#40345,
#40346,#40347,#40348),(#40349,#40350,#40351,#40352,#40353,#40354,#40355,
#40356,#40357,#40358),(#40359,#40360,#40361,#40362,#40363,#40364,#40365,
#40366,#40367,#40368)),.UNSPECIFIED.,.F.,.F.,.F.)
B_SPLINE_SURFACE_WITH_KNOTS((4,4),(4,1,1,1,1,1,1,4),(0.090214820579119,
0.903852852741469),(0.0113422875274,0.1428795028973,0.2858119560905,0.4286835352561,
0.5714929646109,0.7143131099677,0.8572933445083,0.9764111906646),
 .UNSPECIFIED.)
GEOMETRIC_REPRESENTATION_ITEM()
RATIONAL_B_SPLINE_SURFACE(((1.11548030902687,1.11548030902687,1.11548030902687,
1.11548030902687,1.11548030902687,1.11548030902687,1.11548030902687,1.11548030902687,
1.11548030902687,1.11548030902687),(0.962621077558573,0.962621077558573,
0.962621077558573,0.962621077558573,0.962621077558573,0.962621077558573,
0.962621077558573,0.962621077558573,0.962621077558573,0.962621077558573),
(0.961514630885325,0.961514630885325,0.961514630885325,0.961514630885325,
0.961514630885325,0.961514630885325,0.961514630885325,0.961514630885325,
0.961514630885325,0.961514630885325),(1.11216096900712,1.11216096900712,
1.11216096900712,1.11216096900712,1.11216096900712,1.11216096900712,1.11216096900712,
1.11216096900712,1.11216096900712,1.11216096900712)))
REPRESENTATION_ITEM('')
SURFACE()
);
#185=(
BOUNDED_SURFACE()
B_SPLINE_SURFACE(3,3,((#40395,#40396,#40397,#40398,#40399,#40400,#40401,
#40402,#40403),(#40404,#40405,#40406,#40407,#40408,#40409,#40410,#40411,
#40412),(#40413,#40414,#40415,#40416,#40417,#40418,#40419,#40420,#40421),
(#40422,#40423,#40424,#40425,#40426,#40427,#40428,#40429,#40430)),
 .UNSPECIFIED.,.F.,.F.,.F.)
B_SPLINE_SURFACE_WITH_KNOTS((4,4),(4,1,1,1,1,1,4),(0.054728297573913,0.945273202908356),
(0.226874247895751,0.300522254996,0.4096933649142,0.5231718563142,0.6400288266082,
0.7588043312258,0.774211492154076),.UNSPECIFIED.)
GEOMETRIC_REPRESENTATION_ITEM()
RATIONAL_B_SPLINE_SURFACE(((1.19587221360212,1.19587221360212,1.19587221360212,
1.19587221360212,1.19587221360212,1.19587221360212,1.19587221360212,1.19587221360212,
1.19587221360212),(0.934708822097536,0.934708822097536,0.934708822097536,
0.934708822097536,0.934708822097536,0.934708822097536,0.934708822097536,
0.934708822097536,0.934708822097536),(0.934709262133402,0.934709262133402,
0.934709262133402,0.934709262133402,0.934709262133402,0.934709262133402,
0.934709262133402,0.934709262133402,0.934709262133402),(1.19587353370972,
1.19587353370972,1.19587353370972,1.19587353370972,1.19587353370972,1.19587353370972,
1.19587353370972,1.19587353370972,1.19587353370972)))
REPRESENTATION_ITEM('')
SURFACE()
);
#186=(
BOUNDED_SURFACE()
B_SPLINE_SURFACE(3,3,((#40544,#40545,#40546,#40547,#40548,#40549,#40550,
#40551,#40552,#40553),(#40554,#40555,#40556,#40557,#40558,#40559,#40560,
#40561,#40562,#40563),(#40564,#40565,#40566,#40567,#40568,#40569,#40570,
#40571,#40572,#40573),(#40574,#40575,#40576,#40577,#40578,#40579,#40580,
#40581,#40582,#40583)),.UNSPECIFIED.,.F.,.F.,.F.)
B_SPLINE_SURFACE_WITH_KNOTS((4,4),(4,1,1,1,1,1,1,4),(0.0902463740384735,
0.903859594390682),(0.02358777781734,0.1427066554906,0.2856868900361,0.4285070354297,
0.5713164647035,0.7141880438182,0.8571204970713,0.9886565450757),
 .UNSPECIFIED.)
GEOMETRIC_REPRESENTATION_ITEM()
RATIONAL_B_SPLINE_SURFACE(((1.11546252682894,1.11546252682894,1.11546252682894,
1.11546252682894,1.11546252682894,1.11546252682894,1.11546252682894,1.11546252682894,
1.11546252682894,1.11546252682894),(0.962619725152993,0.962619725152993,
0.962619725152993,0.962619725152993,0.962619725152993,0.962619725152993,
0.962619725152993,0.962619725152993,0.962619725152993,0.962619725152993),
(0.961520454467663,0.961520454467663,0.961520454467663,0.961520454467663,
0.961520454467663,0.961520454467663,0.961520454467663,0.961520454467663,
0.961520454467663,0.961520454467663),(1.11216471477295,1.11216471477295,
1.11216471477295,1.11216471477295,1.11216471477295,1.11216471477295,1.11216471477295,
1.11216471477295,1.11216471477295,1.11216471477295)))
REPRESENTATION_ITEM('')
SURFACE()
);
#187=(
BOUNDED_SURFACE()
B_SPLINE_SURFACE(3,3,((#40623,#40624,#40625,#40626,#40627,#40628),(#40629,
#40630,#40631,#40632,#40633,#40634),(#40635,#40636,#40637,#40638,#40639,
#40640),(#40641,#40642,#40643,#40644,#40645,#40646)),.UNSPECIFIED.,.F.,
 .F.,.F.)
B_SPLINE_SURFACE_WITH_KNOTS((4,4),(4,1,1,4),(0.0986342191388958,0.901369959996773),
(0.317543733191685,0.3333147448852,0.6666852551147,0.682456266808859),
 .UNSPECIFIED.)
GEOMETRIC_REPRESENTATION_ITEM()
RATIONAL_B_SPLINE_SURFACE(((1.17563408853197,1.17563408853197,1.17563408853197,
1.17563408853197,1.17563408853197,1.17563408853197),(0.941454084654427,
0.941454084654427,0.941454084654428,0.941454084654428,0.941454084654428,
0.941454084654428),(0.941455303829123,0.941455303829123,0.941455303829123,
0.941455303829123,0.941455303829123,0.941455303829123),(1.17563774605606,
1.17563774605606,1.17563774605606,1.17563774605606,1.17563774605606,1.17563774605606)))
REPRESENTATION_ITEM('')
SURFACE()
);
#188=(
BOUNDED_SURFACE()
B_SPLINE_SURFACE(3,3,((#40886,#40887,#40888,#40889,#40890,#40891,#40892,
#40893,#40894,#40895,#40896,#40897,#40898,#40899,#40900,#40901,#40902,#40903,
#40904,#40905,#40906,#40907,#40908,#40909,#40910,#40911,#40912,#40913,#40914,
#40915,#40916,#40917,#40918,#40919,#40920,#40921,#40922,#40923,#40924,#40925),
(#40926,#40927,#40928,#40929,#40930,#40931,#40932,#40933,#40934,#40935,
#40936,#40937,#40938,#40939,#40940,#40941,#40942,#40943,#40944,#40945,#40946,
#40947,#40948,#40949,#40950,#40951,#40952,#40953,#40954,#40955,#40956,#40957,
#40958,#40959,#40960,#40961,#40962,#40963,#40964,#40965),(#40966,#40967,
#40968,#40969,#40970,#40971,#40972,#40973,#40974,#40975,#40976,#40977,#40978,
#40979,#40980,#40981,#40982,#40983,#40984,#40985,#40986,#40987,#40988,#40989,
#40990,#40991,#40992,#40993,#40994,#40995,#40996,#40997,#40998,#40999,#41000,
#41001,#41002,#41003,#41004,#41005),(#41006,#41007,#41008,#41009,#41010,
#41011,#41012,#41013,#41014,#41015,#41016,#41017,#41018,#41019,#41020,#41021,
#41022,#41023,#41024,#41025,#41026,#41027,#41028,#41029,#41030,#41031,#41032,
#41033,#41034,#41035,#41036,#41037,#41038,#41039,#41040,#41041,#41042,#41043,
#41044,#41045)),.UNSPECIFIED.,.F.,.F.,.F.)
B_SPLINE_SURFACE_WITH_KNOTS((4,4),(4,1,1,1,1,1,1,1,1,1,1,1,1,1,1,1,1,1,
1,1,1,1,1,1,1,1,1,1,1,1,1,1,1,1,1,1,1,4),(0.109557713609705,0.885247213323687),
(-0.009601789269793,0.,0.02232800254047,0.04690499692097,0.07379314494475,
0.1032825879248,0.1358147775015,0.1719129911135,0.2120208291974,0.2562559556703,
0.3048272129563,0.3583973876345,0.4161404010308,0.4734162974592,0.526583520073,
0.5739184110835,0.6155189332402,0.6529905554197,0.6871367384821,0.7180197388927,
0.7460319790749,0.7715260585384,0.7947388244259,0.8158370649057,0.8349859745155,
0.852358315218,0.8681369543747,0.882501434184,0.895628780335,0.9076949488169,
0.9188453219145,0.9291452487614,0.9386433394322,0.9473861202751,0.9554257888082,
0.9628157674929,0.9696063892784,0.9720662895839),.UNSPECIFIED.)
GEOMETRIC_REPRESENTATION_ITEM()
RATIONAL_B_SPLINE_SURFACE(((1.07369786616139,1.07369786616139,1.07369786616139,
1.07369786616139,1.07369786616139,1.07369786616139,1.07369786616139,1.07369786616139,
1.07369786616139,1.07369786616139,1.07369786616139,1.07369786616139,1.07369786616139,
1.07369786616139,1.07369786616139,1.07369786616139,1.07369786616139,1.07369786616139,
1.07369786616139,1.07369786616139,1.07369786616139,1.07369786616139,1.07369786616139,
1.07369786616139,1.07369786616139,1.07369786616139,1.07369786616139,1.07369786616139,
1.07369786616139,1.07369786616139,1.07369786616139,1.07369786616139,1.07369786616139,
1.07369786616139,1.07369786616139,1.07369786616139,1.07369786616139,1.07369786616139,
1.07369786616139,1.07369786616139),(0.976087774690969,0.976087774690969,
0.976087774690969,0.976087774690969,0.976087774690969,0.976087774690969,
0.976087774690969,0.976087774690969,0.976087774690969,0.976087774690969,
0.976087774690969,0.976087774690969,0.976087774690969,0.976087774690969,
0.976087774690969,0.976087774690969,0.976087774690969,0.976087774690969,
0.976087774690969,0.976087774690969,0.976087774690969,0.976087774690969,
0.976087774690969,0.976087774690969,0.976087774690969,0.976087774690969,
0.976087774690969,0.976087774690969,0.976087774690969,0.976087774690969,
0.976087774690969,0.976087774690969,0.976087774690969,0.976087774690969,
0.976087774690969,0.976087774690969,0.976087774690969,0.976087774690969,
0.976087774690969,0.976087774690969),(0.975438393751835,0.975438393751835,
0.975438393751835,0.975438393751835,0.975438393751835,0.975438393751835,
0.975438393751835,0.975438393751835,0.975438393751835,0.975438393751835,
0.975438393751835,0.975438393751835,0.975438393751835,0.975438393751835,
0.975438393751835,0.975438393751835,0.975438393751835,0.975438393751835,
0.975438393751835,0.975438393751835,0.975438393751835,0.975438393751835,
0.975438393751835,0.975438393751835,0.975438393751835,0.975438393751835,
0.975438393751835,0.975438393751835,0.975438393751835,0.975438393751835,
0.975438393751835,0.975438393751835,0.975438393751835,0.975438393751835,
0.975438393751835,0.975438393751835,0.975438393751835,0.975438393751835,
0.975438393751835,0.975438393751835),(1.07174972334399,1.07174972334399,
1.07174972334399,1.07174972334399,1.07174972334399,1.07174972334399,1.07174972334399,
1.07174972334399,1.07174972334399,1.07174972334399,1.07174972334399,1.07174972334399,
1.07174972334399,1.07174972334399,1.07174972334399,1.07174972334399,1.07174972334399,
1.07174972334399,1.07174972334399,1.07174972334399,1.07174972334399,1.07174972334399,
1.07174972334399,1.07174972334399,1.07174972334399,1.07174972334399,1.07174972334399,
1.07174972334399,1.07174972334399,1.07174972334399,1.07174972334399,1.07174972334399,
1.07174972334399,1.07174972334399,1.07174972334399,1.07174972334399,1.07174972334399,
1.07174972334399,1.07174972334399,1.07174972334399)))
REPRESENTATION_ITEM('')
SURFACE()
);
#189=(
BOUNDED_SURFACE()
B_SPLINE_SURFACE(3,3,((#41171,#41172,#41173,#41174,#41175,#41176,#41177,
#41178,#41179),(#41180,#41181,#41182,#41183,#41184,#41185,#41186,#41187,
#41188),(#41189,#41190,#41191,#41192,#41193,#41194,#41195,#41196,#41197),
(#41198,#41199,#41200,#41201,#41202,#41203,#41204,#41205,#41206)),
 .UNSPECIFIED.,.F.,.F.,.F.)
B_SPLINE_SURFACE_WITH_KNOTS((4,4),(4,1,1,1,1,1,4),(0.0545876560709944,0.945414163178399),
(0.227019637278718,0.2408830109945,0.3597029788423,0.4766081773209,0.5901375306023,
0.6993568121791,0.77342322572),.UNSPECIFIED.)
GEOMETRIC_REPRESENTATION_ITEM()
RATIONAL_B_SPLINE_SURFACE(((1.19599641219284,1.19599641219284,1.19599641219284,
1.19599641219284,1.19599641219284,1.19599641219284,1.19599641219284,1.19599641219284,
1.19599641219284),(0.934667328915005,0.934667328915005,0.934667328915005,
0.934667328915005,0.934667328915005,0.934667328915005,0.934667328915005,
0.934667328915005,0.934667328915006),(0.934667862603376,0.934667862603376,
0.934667862603376,0.934667862603376,0.934667862603376,0.934667862603376,
0.934667862603376,0.934667862603376,0.934667862603376),(1.19599801325795,
1.19599801325795,1.19599801325795,1.19599801325795,1.19599801325795,1.19599801325795,
1.19599801325795,1.19599801325795,1.19599801325795)))
REPRESENTATION_ITEM('')
SURFACE()
);
#190=(
BOUNDED_SURFACE()
B_SPLINE_SURFACE(3,3,((#41329,#41330,#41331,#41332,#41333,#41334,#41335,
#41336,#41337,#41338),(#41339,#41340,#41341,#41342,#41343,#41344,#41345,
#41346,#41347,#41348),(#41349,#41350,#41351,#41352,#41353,#41354,#41355,
#41356,#41357,#41358),(#41359,#41360,#41361,#41362,#41363,#41364,#41365,
#41366,#41367,#41368)),.UNSPECIFIED.,.F.,.F.,.F.)
B_SPLINE_SURFACE_WITH_KNOTS((4,4),(4,1,1,1,1,1,1,4),(0.0897026986543284,
0.903562378195111),(0.02295305876099,0.1427319370604,0.2857219203474,0.4285792797614,
0.5713515650105,0.7142098207389,0.8572808214069,0.9622634165798),
 .UNSPECIFIED.)
GEOMETRIC_REPRESENTATION_ITEM()
RATIONAL_B_SPLINE_SURFACE(((1.11534309355231,1.11534309355231,1.11534309355231,
1.11534309355231,1.11534309355231,1.11534309355231,1.11534309355231,1.11534309355231,
1.11534309355231,1.11534309355231),(0.962814520006825,0.962814520006825,
0.962814520006825,0.962814520006825,0.962814520006825,0.962814520006825,
0.962814520006825,0.962814520006825,0.962814520006825,0.962814520006825),
(0.961562661637633,0.961562661637633,0.961562661637633,0.961562661637633,
0.961562661637633,0.961562661637633,0.961562661637633,0.961562661637633,
0.961562661637633,0.961562661637633),(1.11158751844473,1.11158751844473,
1.11158751844473,1.11158751844473,1.11158751844473,1.11158751844473,1.11158751844473,
1.11158751844473,1.11158751844473,1.11158751844473)))
REPRESENTATION_ITEM('')
SURFACE()
);
#191=(
BOUNDED_SURFACE()
B_SPLINE_SURFACE(3,3,((#41587,#41588,#41589,#41590,#41591,#41592,#41593,
#41594,#41595,#41596),(#41597,#41598,#41599,#41600,#41601,#41602,#41603,
#41604,#41605,#41606),(#41607,#41608,#41609,#41610,#41611,#41612,#41613,
#41614,#41615,#41616),(#41617,#41618,#41619,#41620,#41621,#41622,#41623,
#41624,#41625,#41626)),.UNSPECIFIED.,.F.,.F.,.F.)
B_SPLINE_SURFACE_WITH_KNOTS((4,4),(4,1,1,1,1,1,1,4),(0.0573528854689029,
0.942634096168851),(0.2948654053633,0.3479036645395,0.4101463286025,0.4703448613228,
0.5297234926217,0.5899248652657,0.6521709850243,0.7051026564205),
 .UNSPECIFIED.)
GEOMETRIC_REPRESENTATION_ITEM()
RATIONAL_B_SPLINE_SURFACE(((1.19356575363168,1.19356575363168,1.19356575363168,
1.19356575363168,1.19356575363168,1.19356575363168,1.19356575363168,1.19356575363168,
1.19356575363168,1.19356575363168),(0.935481877334427,0.935481877334427,
0.935481877334427,0.935481877334427,0.935481877334427,0.935481877334427,
0.935481877334427,0.935481877334427,0.935481877334427,0.935481877334427),
(0.935478082178781,0.935478082178781,0.935478082178781,0.935478082178781,
0.935478082178781,0.935478082178781,0.935478082178781,0.935478082178781,
0.935478082178781,0.935478082178781),(1.19355436816475,1.19355436816475,
1.19355436816475,1.19355436816475,1.19355436816475,1.19355436816475,1.19355436816475,
1.19355436816475,1.19355436816475,1.19355436816475)))
REPRESENTATION_ITEM('')
SURFACE()
);
#192=(
BOUNDED_SURFACE()
B_SPLINE_SURFACE(3,3,((#41733,#41734,#41735,#41736,#41737,#41738,#41739,
#41740,#41741),(#41742,#41743,#41744,#41745,#41746,#41747,#41748,#41749,
#41750),(#41751,#41752,#41753,#41754,#41755,#41756,#41757,#41758,#41759),
(#41760,#41761,#41762,#41763,#41764,#41765,#41766,#41767,#41768)),
 .UNSPECIFIED.,.F.,.F.,.F.)
B_SPLINE_SURFACE_WITH_KNOTS((4,4),(4,1,1,1,1,1,4),(0.0545525345384962,0.945448460040463),
(0.226579630138955,0.3004022999601,0.4096207676398,0.5231927024745,0.6401765809238,
0.7590171413674,0.773021471035039),.UNSPECIFIED.)
GEOMETRIC_REPRESENTATION_ITEM()
RATIONAL_B_SPLINE_SURFACE(((1.19602600408056,1.19602600408056,1.19602600408056,
1.19602600408056,1.19602600408056,1.19602600408056,1.19602600408056,1.19602600408056,
1.19602600408056),(0.934657706853242,0.934657706853242,0.934657706853242,
0.934657706853242,0.934657706853242,0.934657706853242,0.934657706853242,
0.934657706853242,0.934657706853242),(0.934657998640073,0.934657998640073,
0.934657998640073,0.934657998640073,0.934657998640073,0.934657998640073,
0.934657998640073,0.934657998640073,0.934657998640073),(1.19602687944105,
1.19602687944105,1.19602687944105,1.19602687944105,1.19602687944105,1.19602687944105,
1.19602687944105,1.19602687944105,1.19602687944105)))
REPRESENTATION_ITEM('')
SURFACE()
);
#193=(
BOUNDED_SURFACE()
B_SPLINE_SURFACE(3,3,((#41879,#41880,#41881,#41882,#41883,#41884,#41885,
#41886,#41887,#41888,#41889),(#41890,#41891,#41892,#41893,#41894,#41895,
#41896,#41897,#41898,#41899,#41900),(#41901,#41902,#41903,#41904,#41905,
#41906,#41907,#41908,#41909,#41910,#41911),(#41912,#41913,#41914,#41915,
#41916,#41917,#41918,#41919,#41920,#41921,#41922)),.UNSPECIFIED.,.F.,.F.,
 .F.)
B_SPLINE_SURFACE_WITH_KNOTS((4,4),(4,1,1,1,1,1,1,1,4),(0.0753633925526522,
0.903551965100841),(-0.009670337421388,0.,0.1430991485311,0.2858285059199,
0.4284781713031,0.5715215149008,0.7145472299923,0.8573672624017,0.9759160460961),
 .UNSPECIFIED.)
GEOMETRIC_REPRESENTATION_ITEM()
RATIONAL_B_SPLINE_SURFACE(((1.12354604891087,1.12354604891087,1.12354604891087,
1.12354604891087,1.12354604891087,1.12354604891087,1.12354604891087,1.12354604891087,
1.12354604891087,1.12354604891087,1.12354604891087),(0.962907636211588,
0.962907636211588,0.962907636211588,0.962907636211588,0.962907636211588,
0.962907636211588,0.962907636211588,0.962907636211588,0.962907636211588,
0.962907636211588,0.962907636211588),(0.958919516229146,0.958919516229146,
0.958919516229146,0.958919516229146,0.958919516229146,0.958919516229146,
0.958919516229146,0.958919516229146,0.958919516229146,0.958919516229146,
0.958919516229146),(1.11158168896355,1.11158168896355,1.11158168896355,
1.11158168896355,1.11158168896355,1.11158168896355,1.11158168896355,1.11158168896355,
1.11158168896355,1.11158168896355,1.11158168896355)))
REPRESENTATION_ITEM('')
SURFACE()
);
#194=(
BOUNDED_SURFACE()
B_SPLINE_SURFACE(3,3,((#42039,#42040,#42041,#42042),(#42043,#42044,#42045,
#42046),(#42047,#42048,#42049,#42050),(#42051,#42052,#42053,#42054)),
 .UNSPECIFIED.,.F.,.F.,.F.)
B_SPLINE_SURFACE_WITH_KNOTS((4,4),(4,4),(0.0986320320018917,0.901362552765544),
(-0.975145040392605,-0.0991746183702489),.UNSPECIFIED.)
GEOMETRIC_REPRESENTATION_ITEM()
RATIONAL_B_SPLINE_SURFACE(((1.17563600436037,1.17563600436037,1.17563600436037,
1.17563600436037),(0.941456244993406,0.941456244993406,0.941456244993406,
0.941456244993406),(0.941454665223768,0.941454665223768,0.941454665223768,
0.941454665223768),(1.17563126505145,1.17563126505145,1.17563126505145,
1.17563126505145)))
REPRESENTATION_ITEM('')
SURFACE()
);
#195=(
BOUNDED_SURFACE()
B_SPLINE_SURFACE(3,3,((#42073,#42074,#42075,#42076,#42077,#42078,#42079,
#42080,#42081,#42082,#42083,#42084,#42085,#42086,#42087,#42088,#42089,#42090,
#42091,#42092,#42093,#42094,#42095,#42096,#42097,#42098,#42099,#42100,#42101,
#42102,#42103,#42104,#42105),(#42106,#42107,#42108,#42109,#42110,#42111,
#42112,#42113,#42114,#42115,#42116,#42117,#42118,#42119,#42120,#42121,#42122,
#42123,#42124,#42125,#42126,#42127,#42128,#42129,#42130,#42131,#42132,#42133,
#42134,#42135,#42136,#42137,#42138),(#42139,#42140,#42141,#42142,#42143,
#42144,#42145,#42146,#42147,#42148,#42149,#42150,#42151,#42152,#42153,#42154,
#42155,#42156,#42157,#42158,#42159,#42160,#42161,#42162,#42163,#42164,#42165,
#42166,#42167,#42168,#42169,#42170,#42171),(#42172,#42173,#42174,#42175,
#42176,#42177,#42178,#42179,#42180,#42181,#42182,#42183,#42184,#42185,#42186,
#42187,#42188,#42189,#42190,#42191,#42192,#42193,#42194,#42195,#42196,#42197,
#42198,#42199,#42200,#42201,#42202,#42203,#42204)),.UNSPECIFIED.,.F.,.F.,
 .F.)
B_SPLINE_SURFACE_WITH_KNOTS((4,4),(4,1,1,1,1,1,1,1,1,1,1,1,1,1,1,1,1,1,
1,1,1,1,1,1,1,1,1,1,1,1,4),(0.108378650171574,0.903586235863032),(-0.009736901743296,
0.,0.02218413179576,0.04656961109638,0.07320227077888,0.1023246073713,0.1343070073107,
0.1695983831343,0.2086113444874,0.2515282384527,0.2985700177486,0.350328036692,
0.4076667288658,0.4682132326039,0.528225646619,0.5849768379219,0.6367767624475,
0.6825350754174,0.7235069669497,0.7605071950811,0.7940293660298,0.8241786597893,
0.8510660708028,0.8750221728291,0.8964633607905,0.9157954007781,0.9333737553394,
0.9493579414419,0.963858565732,0.9770543416123,0.985715500525),
 .UNSPECIFIED.)
GEOMETRIC_REPRESENTATION_ITEM()
RATIONAL_B_SPLINE_SURFACE(((1.07414501665385,1.07414501665385,1.07414501665385,
1.07414501665385,1.07414501665385,1.07414501665385,1.07414501665385,1.07414501665385,
1.07414501665385,1.07414501665385,1.07414501665385,1.07414501665385,1.07414501665385,
1.07414501665385,1.07414501665385,1.07414501665385,1.07414501665385,1.07414501665385,
1.07414501665385,1.07414501665385,1.07414501665385,1.07414501665385,1.07414501665385,
1.07414501665385,1.07414501665385,1.07414501665385,1.07414501665385,1.07414501665385,
1.07414501665385,1.07414501665385,1.07414501665385,1.07414501665385,1.07414501665385),
(0.973774799844115,0.973774799844115,0.973774799844115,0.973774799844115,
0.973774799844115,0.973774799844115,0.973774799844115,0.973774799844115,
0.973774799844115,0.973774799844115,0.973774799844115,0.973774799844115,
0.973774799844115,0.973774799844115,0.973774799844115,0.973774799844115,
0.973774799844115,0.973774799844115,0.973774799844115,0.973774799844115,
0.973774799844115,0.973774799844115,0.973774799844115,0.973774799844115,
0.973774799844115,0.973774799844115,0.973774799844115,0.973774799844115,
0.973774799844115,0.973774799844115,0.973774799844115,0.973774799844115,
0.973774799844115),(0.975308064317468,0.975308064317468,0.975308064317468,
0.975308064317468,0.975308064317468,0.975308064317468,0.975308064317468,
0.975308064317468,0.975308064317468,0.975308064317468,0.975308064317468,
0.975308064317468,0.975308064317468,0.975308064317468,0.975308064317468,
0.975308064317468,0.975308064317468,0.975308064317468,0.975308064317468,
0.975308064317468,0.975308064317468,0.975308064317468,0.975308064317468,
0.975308064317468,0.975308064317468,0.975308064317468,0.975308064317468,
0.975308064317468,0.975308064317468,0.975308064317468,0.975308064317468,
0.975308064317468,0.975308064317468),(1.07874481007391,1.07874481007391,
1.07874481007391,1.07874481007391,1.07874481007391,1.07874481007391,1.07874481007391,
1.07874481007391,1.07874481007391,1.07874481007391,1.07874481007391,1.07874481007391,
1.07874481007391,1.07874481007391,1.07874481007391,1.07874481007391,1.07874481007391,
1.07874481007391,1.07874481007391,1.07874481007391,1.07874481007391,1.07874481007391,
1.07874481007391,1.07874481007391,1.07874481007391,1.07874481007391,1.07874481007391,
1.07874481007391,1.07874481007391,1.07874481007391,1.07874481007391,1.07874481007391,
1.07874481007391)))
REPRESENTATION_ITEM('')
SURFACE()
);
#196=(
BOUNDED_SURFACE()
B_SPLINE_SURFACE(3,3,((#42590,#42591,#42592,#42593,#42594,#42595,#42596,
#42597,#42598,#42599,#42600),(#42601,#42602,#42603,#42604,#42605,#42606,
#42607,#42608,#42609,#42610,#42611),(#42612,#42613,#42614,#42615,#42616,
#42617,#42618,#42619,#42620,#42621,#42622),(#42623,#42624,#42625,#42626,
#42627,#42628,#42629,#42630,#42631,#42632,#42633)),.UNSPECIFIED.,.F.,.F.,
 .F.)
B_SPLINE_SURFACE_WITH_KNOTS((4,4),(4,1,1,1,1,1,1,1,4),(0.0573248939826349,
0.942652782085426),(0.294899609167,0.3228689298849,0.3831046509521,0.4422669195799,
0.4999589566113,0.5576491953134,0.6168076022616,0.6770470459264,0.7051410016013),
 .UNSPECIFIED.)
GEOMETRIC_REPRESENTATION_ITEM()
RATIONAL_B_SPLINE_SURFACE(((1.19358809665843,1.19358809665843,1.19358809665843,
1.19358809665843,1.19358809665843,1.19358809665843,1.19358809665843,1.19358809665843,
1.19358809665843,1.19358809665843,1.19358809665843),(0.935477142828405,
0.935477142828405,0.935477142828405,0.935477142828405,0.935477142828405,
0.935477142828405,0.935477142828405,0.935477142828405,0.935477142828405,
0.935477142828405,0.935477142828405),(0.935470634611331,0.935470634611331,
0.935470634611331,0.935470634611331,0.935470634611331,0.935470634611331,
0.935470634611331,0.935470634611331,0.935470634611331,0.935470634611331,
0.935470634611331),(1.19356857200721,1.19356857200721,1.19356857200721,
1.19356857200721,1.19356857200721,1.19356857200721,1.19356857200721,1.19356857200721,
1.19356857200721,1.19356857200721,1.19356857200721)))
REPRESENTATION_ITEM('')
SURFACE()
);
#197=(
BOUNDED_SURFACE()
B_SPLINE_SURFACE(3,3,((#42718,#42719,#42720,#42721,#42722,#42723,#42724,
#42725,#42726),(#42727,#42728,#42729,#42730,#42731,#42732,#42733,#42734,
#42735),(#42736,#42737,#42738,#42739,#42740,#42741,#42742,#42743,#42744),
(#42745,#42746,#42747,#42748,#42749,#42750,#42751,#42752,#42753)),
 .UNSPECIFIED.,.F.,.F.,.F.)
B_SPLINE_SURFACE_WITH_KNOTS((4,4),(4,1,1,1,1,1,4),(0.0546312169533823,0.945370286804514),
(0.225683109986944,0.2412765766488,0.3600743765287,0.4770048853175,0.5905230256156,
0.6996938806735,0.773232633815288),.UNSPECIFIED.)
GEOMETRIC_REPRESENTATION_ITEM()
RATIONAL_B_SPLINE_SURFACE(((1.19595763086821,1.19595763086821,1.19595763086821,
1.19595763086821,1.19595763086821,1.19595763086821,1.19595763086821,1.19595763086821,
1.19595763086821),(0.934680348618612,0.934680348618612,0.934680348618612,
0.934680348618612,0.934680348618612,0.934680348618612,0.934680348618612,
0.934680348618612,0.934680348618612),(0.934680789711243,0.934680789711243,
0.934680789711243,0.934680789711243,0.934680789711243,0.934680789711243,
0.934680789711243,0.934680789711243,0.934680789711243),(1.1959589541461,
1.1959589541461,1.1959589541461,1.1959589541461,1.1959589541461,1.1959589541461,
1.1959589541461,1.1959589541461,1.1959589541461)))
REPRESENTATION_ITEM('')
SURFACE()
);
#198=(
BOUNDED_SURFACE()
B_SPLINE_SURFACE(3,3,((#42867,#42868,#42869,#42870,#42871,#42872,#42873,
#42874,#42875,#42876),(#42877,#42878,#42879,#42880,#42881,#42882,#42883,
#42884,#42885,#42886),(#42887,#42888,#42889,#42890,#42891,#42892,#42893,
#42894,#42895,#42896),(#42897,#42898,#42899,#42900,#42901,#42902,#42903,
#42904,#42905,#42906)),.UNSPECIFIED.,.F.,.F.,.F.)
B_SPLINE_SURFACE_WITH_KNOTS((4,4),(4,1,1,1,1,1,1,4),(0.0902162146474901,
0.90384766932744),(0.01134228752741,0.1428795028254,0.2858119558808,0.4286835351635,
0.5714929647039,0.7143131099766,0.8572933445059,0.9764111906646),
 .UNSPECIFIED.)
GEOMETRIC_REPRESENTATION_ITEM()
RATIONAL_B_SPLINE_SURFACE(((1.11547952330921,1.11547952330921,1.11547952330921,
1.11547952330921,1.11547952330921,1.11547952330921,1.11547952330921,1.11547952330921,
1.11547952330921,1.11547952330921),(0.962622047579736,0.962622047579736,
0.962622047579736,0.962622047579736,0.962622047579736,0.962622047579736,
0.962622047579736,0.962622047579736,0.962622047579736,0.962622047579736),
(0.961514903100546,0.961514903100546,0.961514903100546,0.961514903100546,
0.961514903100546,0.961514903100546,0.961514903100546,0.961514903100546,
0.961514903100546,0.961514903100546),(1.11215808987164,1.11215808987164,
1.11215808987164,1.11215808987164,1.11215808987164,1.11215808987164,1.11215808987164,
1.11215808987164,1.11215808987164,1.11215808987164)))
REPRESENTATION_ITEM('')
SURFACE()
);
#199=(
BOUNDED_SURFACE()
B_SPLINE_SURFACE(3,3,((#42933,#42934,#42935,#42936,#42937,#42938,#42939,
#42940,#42941),(#42942,#42943,#42944,#42945,#42946,#42947,#42948,#42949,
#42950),(#42951,#42952,#42953,#42954,#42955,#42956,#42957,#42958,#42959),
(#42960,#42961,#42962,#42963,#42964,#42965,#42966,#42967,#42968)),
 .UNSPECIFIED.,.F.,.F.,.F.)
B_SPLINE_SURFACE_WITH_KNOTS((4,4),(4,1,1,1,1,1,4),(0.0547193706907307,0.94528212979141),
(0.226873519265384,0.300522254996,0.4096933649141,0.5231718563141,0.6400288266082,
0.7588043312258,0.774220135722599),.UNSPECIFIED.)
GEOMETRIC_REPRESENTATION_ITEM()
RATIONAL_B_SPLINE_SURFACE(((1.19588006744166,1.19588006744166,1.19588006744166,
1.19588006744166,1.19588006744166,1.19588006744166,1.19588006744166,1.19588006744166,
1.19588006744166),(0.934706204142303,0.934706204142303,0.934706204142303,
0.934706204142303,0.934706204142303,0.934706204142303,0.934706204142303,
0.934706204142303,0.934706204142303),(0.934706644186953,0.934706644186953,
0.934706644186953,0.934706644186953,0.934706644186953,0.934706644186953,
0.934706644186953,0.934706644186953,0.934706644186953),(1.19588138757561,
1.19588138757561,1.19588138757561,1.19588138757561,1.19588138757561,1.19588138757561,
1.19588138757561,1.19588138757561,1.19588138757561)))
REPRESENTATION_ITEM('')
SURFACE()
);
#200=(
BOUNDED_SURFACE()
B_SPLINE_SURFACE(3,3,((#43082,#43083,#43084,#43085,#43086,#43087,#43088,
#43089,#43090,#43091),(#43092,#43093,#43094,#43095,#43096,#43097,#43098,
#43099,#43100,#43101),(#43102,#43103,#43104,#43105,#43106,#43107,#43108,
#43109,#43110,#43111),(#43112,#43113,#43114,#43115,#43116,#43117,#43118,
#43119,#43120,#43121)),.UNSPECIFIED.,.F.,.F.,.F.)
B_SPLINE_SURFACE_WITH_KNOTS((4,4),(4,1,1,1,1,1,1,4),(0.0902477372797298,
0.903859553668012),(0.02358777781735,0.1427066554932,0.2856868900266,0.4285070353299,
0.5713164648028,0.714188044043,0.8571204971484,0.9886565450757),
 .UNSPECIFIED.)
GEOMETRIC_REPRESENTATION_ITEM()
RATIONAL_B_SPLINE_SURFACE(((1.11546175854762,1.11546175854762,1.11546175854762,
1.11546175854762,1.11546175854762,1.11546175854762,1.11546175854762,1.11546175854762,
1.11546175854762,1.11546175854762),(0.962619729119499,0.962619729119499,
0.962619729119499,0.962619729119499,0.962619729119499,0.962619729119499,
0.962619729119499,0.962619729119499,0.962619729119499,0.962619729119499),
(0.961520706987935,0.961520706987935,0.961520706987935,0.961520706987935,
0.961520706987935,0.961520706987935,0.961520706987935,0.961520706987935,
0.961520706987935,0.961520706987935),(1.11216469215293,1.11216469215293,
1.11216469215293,1.11216469215293,1.11216469215293,1.11216469215293,1.11216469215293,
1.11216469215293,1.11216469215293,1.11216469215293)))
REPRESENTATION_ITEM('')
SURFACE()
);
#201=(
BOUNDED_SURFACE()
B_SPLINE_SURFACE(3,3,((#43161,#43162,#43163,#43164,#43165,#43166),(#43167,
#43168,#43169,#43170,#43171,#43172),(#43173,#43174,#43175,#43176,#43177,
#43178),(#43179,#43180,#43181,#43182,#43183,#43184)),.UNSPECIFIED.,.F.,
 .F.,.F.)
B_SPLINE_SURFACE_WITH_KNOTS((4,4),(4,1,1,4),(0.0986342191388437,0.901369960096874),
(0.317543733191054,0.3333147448853,0.6666852551148,0.682456266810123),
 .UNSPECIFIED.)
GEOMETRIC_REPRESENTATION_ITEM()
RATIONAL_B_SPLINE_SURFACE(((1.17563408853202,1.17563408853202,1.17563408853202,
1.17563408853202,1.17563408853202,1.17563408853202),(0.941454084625226,
0.941454084625226,0.941454084625226,0.941454084625226,0.941454084625226,
0.941454084625226),(0.941455303829108,0.941455303829108,0.941455303829108,
0.941455303829108,0.941455303829108,0.941455303829108),(1.17563774614367,
1.17563774614367,1.17563774614367,1.17563774614367,1.17563774614367,1.17563774614367)))
REPRESENTATION_ITEM('')
SURFACE()
);
#202=(
BOUNDED_SURFACE()
B_SPLINE_SURFACE(3,3,((#43424,#43425,#43426,#43427,#43428,#43429,#43430,
#43431,#43432,#43433,#43434,#43435,#43436,#43437,#43438,#43439,#43440,#43441,
#43442,#43443,#43444,#43445,#43446,#43447,#43448,#43449,#43450,#43451,#43452,
#43453,#43454,#43455,#43456,#43457,#43458,#43459,#43460,#43461,#43462,#43463),
(#43464,#43465,#43466,#43467,#43468,#43469,#43470,#43471,#43472,#43473,
#43474,#43475,#43476,#43477,#43478,#43479,#43480,#43481,#43482,#43483,#43484,
#43485,#43486,#43487,#43488,#43489,#43490,#43491,#43492,#43493,#43494,#43495,
#43496,#43497,#43498,#43499,#43500,#43501,#43502,#43503),(#43504,#43505,
#43506,#43507,#43508,#43509,#43510,#43511,#43512,#43513,#43514,#43515,#43516,
#43517,#43518,#43519,#43520,#43521,#43522,#43523,#43524,#43525,#43526,#43527,
#43528,#43529,#43530,#43531,#43532,#43533,#43534,#43535,#43536,#43537,#43538,
#43539,#43540,#43541,#43542,#43543),(#43544,#43545,#43546,#43547,#43548,
#43549,#43550,#43551,#43552,#43553,#43554,#43555,#43556,#43557,#43558,#43559,
#43560,#43561,#43562,#43563,#43564,#43565,#43566,#43567,#43568,#43569,#43570,
#43571,#43572,#43573,#43574,#43575,#43576,#43577,#43578,#43579,#43580,#43581,
#43582,#43583)),.UNSPECIFIED.,.F.,.F.,.F.)
B_SPLINE_SURFACE_WITH_KNOTS((4,4),(4,1,1,1,1,1,1,1,1,1,1,1,1,1,1,1,1,1,
1,1,1,1,1,1,1,1,1,1,1,1,1,1,1,1,1,1,1,4),(0.109557623003378,0.885243870225913),
(-0.009601789273473,0.,0.02232833549656,0.04690550208439,0.07379362467687,
0.1032829469298,0.1358149659673,0.1719129604547,0.2120204765667,0.2562549558966,
0.3048250014041,0.3583933178769,0.4161357109095,0.4734125795377,0.5265814299997,
0.5739176940639,0.6155190247053,0.6529911923141,0.6871377766586,0.7180210170724,
0.7460333746103,0.7715274743231,0.7947401813888,0.8158383097167,0.8349870800806,
0.8523592732021,0.86813775977,0.8825020836395,0.8956292723195,0.9076952836912,
0.9188455009779,0.9291452784589,0.9386432333899,0.9473858993638,0.9554254804025,
0.9628154053197,0.9696060115487,0.972066289616),.UNSPECIFIED.)
GEOMETRIC_REPRESENTATION_ITEM()
RATIONAL_B_SPLINE_SURFACE(((1.07369790036373,1.07369790036373,1.07369790036373,
1.07369790036373,1.07369790036373,1.07369790036373,1.07369790036373,1.07369790036373,
1.07369790036373,1.07369790036373,1.07369790036373,1.07369790036373,1.07369790036373,
1.07369790036373,1.07369790036373,1.07369790036373,1.07369790036373,1.07369790036373,
1.07369790036373,1.07369790036373,1.07369790036373,1.07369790036373,1.07369790036373,
1.07369790036373,1.07369790036373,1.07369790036373,1.07369790036373,1.07369790036373,
1.07369790036373,1.07369790036373,1.07369790036373,1.07369790036373,1.07369790036373,
1.07369790036373,1.07369790036373,1.07369790036373,1.07369790036373,1.07369790036373,
1.07369790036373,1.07369790036373),(0.976088195527518,0.976088195527518,
0.976088195527518,0.976088195527518,0.976088195527518,0.976088195527518,
0.976088195527518,0.976088195527518,0.976088195527518,0.976088195527518,
0.976088195527518,0.976088195527518,0.976088195527518,0.976088195527518,
0.976088195527518,0.976088195527518,0.976088195527518,0.976088195527518,
0.976088195527518,0.976088195527518,0.976088195527518,0.976088195527518,
0.976088195527518,0.976088195527518,0.976088195527518,0.976088195527518,
0.976088195527518,0.976088195527518,0.976088195527518,0.976088195527518,
0.976088195527518,0.976088195527518,0.976088195527518,0.976088195527518,
0.976088195527518,0.976088195527518,0.976088195527518,0.976088195527518,
0.976088195527518,0.976088195527518),(0.97543838810218,0.97543838810218,
0.97543838810218,0.97543838810218,0.97543838810218,0.97543838810218,0.97543838810218,
0.97543838810218,0.97543838810218,0.97543838810218,0.97543838810218,0.97543838810218,
0.97543838810218,0.97543838810218,0.97543838810218,0.97543838810218,0.97543838810218,
0.97543838810218,0.97543838810218,0.97543838810218,0.97543838810218,0.97543838810218,
0.97543838810218,0.97543838810218,0.97543838810218,0.97543838810218,0.97543838810218,
0.97543838810218,0.97543838810218,0.97543838810218,0.97543838810218,0.97543838810218,
0.97543838810218,0.97543838810218,0.97543838810218,0.97543838810218,0.97543838810218,
0.97543838810218,0.97543838810218,0.97543838810218),(1.07174847808772,1.07174847808772,
1.07174847808772,1.07174847808772,1.07174847808772,1.07174847808772,1.07174847808772,
1.07174847808772,1.07174847808772,1.07174847808772,1.07174847808772,1.07174847808772,
1.07174847808772,1.07174847808772,1.07174847808772,1.07174847808772,1.07174847808772,
1.07174847808772,1.07174847808772,1.07174847808772,1.07174847808772,1.07174847808772,
1.07174847808772,1.07174847808772,1.07174847808772,1.07174847808772,1.07174847808772,
1.07174847808772,1.07174847808772,1.07174847808772,1.07174847808772,1.07174847808772,
1.07174847808772,1.07174847808772,1.07174847808772,1.07174847808772,1.07174847808772,
1.07174847808772,1.07174847808772,1.07174847808772)))
REPRESENTATION_ITEM('')
SURFACE()
);
#203=(
BOUNDED_SURFACE()
B_SPLINE_SURFACE(3,3,((#43709,#43710,#43711,#43712,#43713,#43714,#43715,
#43716,#43717),(#43718,#43719,#43720,#43721,#43722,#43723,#43724,#43725,
#43726),(#43727,#43728,#43729,#43730,#43731,#43732,#43733,#43734,#43735),
(#43736,#43737,#43738,#43739,#43740,#43741,#43742,#43743,#43744)),
 .UNSPECIFIED.,.F.,.F.,.F.)
B_SPLINE_SURFACE_WITH_KNOTS((4,4),(4,1,1,1,1,1,4),(0.0545793311456824,0.945422488105894),
(0.227011587403803,0.2408830109939,0.3597029788418,0.4766081773206,0.5901375306021,
0.6993568121789,0.773423223303175),.UNSPECIFIED.)
GEOMETRIC_REPRESENTATION_ITEM()
RATIONAL_B_SPLINE_SURFACE(((1.19600373875636,1.19600373875636,1.19600373875636,
1.19600373875636,1.19600373875636,1.19600373875636,1.19600373875636,1.19600373875636,
1.19600373875636),(0.934664886716483,0.934664886716483,0.934664886716483,
0.934664886716483,0.934664886716483,0.934664886716483,0.934664886716483,
0.934664886716483,0.934664886716483),(0.934665420415469,0.934665420415469,
0.934665420415469,0.934665420415469,0.934665420415469,0.934665420415469,
0.934665420415469,0.934665420415469,0.934665420415469),(1.19600533985332,
1.19600533985332,1.19600533985332,1.19600533985332,1.19600533985332,1.19600533985332,
1.19600533985332,1.19600533985332,1.19600533985332)))
REPRESENTATION_ITEM('')
SURFACE()
);
#204=(
BOUNDED_SURFACE()
B_SPLINE_SURFACE(3,3,((#43867,#43868,#43869,#43870,#43871,#43872,#43873,
#43874,#43875,#43876),(#43877,#43878,#43879,#43880,#43881,#43882,#43883,
#43884,#43885,#43886),(#43887,#43888,#43889,#43890,#43891,#43892,#43893,
#43894,#43895,#43896),(#43897,#43898,#43899,#43900,#43901,#43902,#43903,
#43904,#43905,#43906)),.UNSPECIFIED.,.F.,.F.,.F.)
B_SPLINE_SURFACE_WITH_KNOTS((4,4),(4,1,1,1,1,1,1,4),(0.0897026965389358,
0.903562338706292),(0.02295305876098,0.1427319370604,0.2857219203474,0.4285792797614,
0.5713515650105,0.7142098207389,0.8572808214069,0.9622634165798),
 .UNSPECIFIED.)
GEOMETRIC_REPRESENTATION_ITEM()
RATIONAL_B_SPLINE_SURFACE(((1.11534309473627,1.11534309473627,1.11534309473627,
1.11534309473627,1.11534309473627,1.11534309473627,1.11534309473627,1.11534309473627,
1.11534309473627,1.11534309473627),(0.962814527415761,0.962814527415761,
0.962814527415761,0.962814527415761,0.962814527415761,0.962814527415761,
0.962814527415761,0.962814527415761,0.962814527415761,0.962814527415761),
(0.961562661370903,0.961562661370903,0.961562661370903,0.961562661370903,
0.961562661370903,0.961562661370903,0.961562661370903,0.961562661370903,
0.961562661370903,0.961562661370903),(1.11158749660169,1.11158749660169,
1.11158749660169,1.11158749660169,1.11158749660169,1.11158749660169,1.11158749660169,
1.11158749660169,1.11158749660169,1.11158749660169)))
REPRESENTATION_ITEM('')
SURFACE()
);
#205=(
BOUNDED_SURFACE()
B_SPLINE_SURFACE(3,3,((#44125,#44126,#44127,#44128,#44129,#44130,#44131,
#44132,#44133,#44134),(#44135,#44136,#44137,#44138,#44139,#44140,#44141,
#44142,#44143,#44144),(#44145,#44146,#44147,#44148,#44149,#44150,#44151,
#44152,#44153,#44154),(#44155,#44156,#44157,#44158,#44159,#44160,#44161,
#44162,#44163,#44164)),.UNSPECIFIED.,.F.,.F.,.F.)
B_SPLINE_SURFACE_WITH_KNOTS((4,4),(4,1,1,1,1,1,1,4),(0.0573437802388626,
0.942642820662885),(0.2948660946595,0.3474071011045,0.4097589840936,0.4702619662571,
0.529805073191,0.590310974462,0.6526656534762,0.705101945972),
 .UNSPECIFIED.)
GEOMETRIC_REPRESENTATION_ITEM()
RATIONAL_B_SPLINE_SURFACE(((1.19357372994919,1.19357372994919,1.19357372994919,
1.19357372994919,1.19357372994919,1.19357372994919,1.19357372994919,1.19357372994919,
1.19357372994919,1.19357372994919),(0.935479329637411,0.935479329637411,
0.935479329637411,0.935479329637411,0.935479329637411,0.935479329637411,
0.935479329637411,0.935479329637411,0.935479329637411,0.935479329637411),
(0.935475423409424,0.935475423409424,0.935475423409424,0.935475423409424,
0.935475423409424,0.935475423409424,0.935475423409424,0.935475423409424,
0.935475423409424,0.935475423409424),(1.19356201126523,1.19356201126523,
1.19356201126523,1.19356201126523,1.19356201126523,1.19356201126523,1.19356201126523,
1.19356201126523,1.19356201126523,1.19356201126523)))
REPRESENTATION_ITEM('')
SURFACE()
);
#206=(
BOUNDED_SURFACE()
B_SPLINE_SURFACE(3,3,((#44259,#44260,#44261,#44262,#44263,#44264,#44265,
#44266,#44267),(#44268,#44269,#44270,#44271,#44272,#44273,#44274,#44275,
#44276),(#44277,#44278,#44279,#44280,#44281,#44282,#44283,#44284,#44285),
(#44286,#44287,#44288,#44289,#44290,#44291,#44292,#44293,#44294)),
 .UNSPECIFIED.,.F.,.F.,.F.)
B_SPLINE_SURFACE_WITH_KNOTS((4,4),(4,1,1,1,1,1,4),(0.0548579677244621,0.945143053644028),
(0.226589591927513,0.2992910874271,0.4098062007976,0.5242045106109,0.6406468664689,
0.7577450573157,0.772721238525241),.UNSPECIFIED.)
GEOMETRIC_REPRESENTATION_ITEM()
RATIONAL_B_SPLINE_SURFACE(((1.19575728709686,1.19575728709686,1.19575728709686,
1.19575728709686,1.19575728709686,1.19575728709686,1.19575728709686,1.19575728709686,
1.19575728709686),(0.934747271527121,0.934747271527121,0.934747271527121,
0.934747271527121,0.934747271527121,0.934747271527121,0.934747271527121,
0.934747271527121,0.934747271527121),(0.934747570967958,0.934747570967958,
0.934747570967958,0.934747570967958,0.934747570967958,0.934747570967958,
0.934747570967958,0.934747570967958,0.934747570967958),(1.19575818541937,
1.19575818541937,1.19575818541937,1.19575818541937,1.19575818541937,1.19575818541937,
1.19575818541937,1.19575818541937,1.19575818541937)))
REPRESENTATION_ITEM('')
SURFACE()
);
#207=(
BOUNDED_SURFACE()
B_SPLINE_SURFACE(3,3,((#44408,#44409,#44410,#44411,#44412,#44413,#44414,
#44415,#44416,#44417,#44418),(#44419,#44420,#44421,#44422,#44423,#44424,
#44425,#44426,#44427,#44428,#44429),(#44430,#44431,#44432,#44433,#44434,
#44435,#44436,#44437,#44438,#44439,#44440),(#44441,#44442,#44443,#44444,
#44445,#44446,#44447,#44448,#44449,#44450,#44451)),.UNSPECIFIED.,.F.,.F.,
 .F.)
B_SPLINE_SURFACE_WITH_KNOTS((4,4),(4,1,1,1,1,1,1,1,4),(0.075363327412368,
0.90576708085259),(-0.009670337409301,0.,0.1430996309434,0.2858291680282,
0.4284783625449,0.5715211775605,0.714546629698,0.8573667380228,0.9759160461734),
 .UNSPECIFIED.)
GEOMETRIC_REPRESENTATION_ITEM()
RATIONAL_B_SPLINE_SURFACE(((1.12354608676129,1.12354608676129,1.12354608676129,
1.12354608676129,1.12354608676129,1.12354608676129,1.12354608676129,1.12354608676129,
1.12354608676129,1.12354608676129,1.12354608676129),(0.962477985028778,
0.962477985028778,0.962477985028778,0.962477985028778,0.962477985028778,
0.962477985028778,0.962477985028778,0.962477985028778,0.962477985028778,
0.962477985028778,0.962477985028778),(0.958899291150656,0.958899291150656,
0.958899291150656,0.958899291150656,0.958899291150656,0.958899291150656,
0.958899291150656,0.958899291150656,0.958899291150656,0.958899291150656,
0.958899291150656),(1.11281000512692,1.11281000512692,1.11281000512692,
1.11281000512692,1.11281000512692,1.11281000512692,1.11281000512692,1.11281000512692,
1.11281000512692,1.11281000512692,1.11281000512692)))
REPRESENTATION_ITEM('')
SURFACE()
);
#208=(
BOUNDED_SURFACE()
B_SPLINE_SURFACE(3,3,((#44568,#44569,#44570,#44571),(#44572,#44573,#44574,
#44575),(#44576,#44577,#44578,#44579),(#44580,#44581,#44582,#44583)),
 .UNSPECIFIED.,.F.,.F.,.F.)
B_SPLINE_SURFACE_WITH_KNOTS((4,4),(4,4),(0.0986320319756791,0.901362552764652),
(-0.975145040412961,-0.0991746183684475),.UNSPECIFIED.)
GEOMETRIC_REPRESENTATION_ITEM()
RATIONAL_B_SPLINE_SURFACE(((1.17563600438331,1.17563600438331,1.17563600438331,
1.17563600438331),(0.941456244993666,0.941456244993666,0.941456244993666,
0.941456244993666),(0.941454665216122,0.941454665216122,0.941454665216122,
0.941454665216122),(1.17563126505067,1.17563126505067,1.17563126505067,
1.17563126505067)))
REPRESENTATION_ITEM('')
SURFACE()
);
#209=(
BOUNDED_SURFACE()
B_SPLINE_SURFACE(3,3,((#44602,#44603,#44604,#44605,#44606,#44607,#44608,
#44609,#44610,#44611,#44612,#44613,#44614,#44615,#44616,#44617,#44618,#44619,
#44620,#44621,#44622,#44623,#44624,#44625,#44626,#44627,#44628,#44629,#44630,
#44631,#44632,#44633,#44634),(#44635,#44636,#44637,#44638,#44639,#44640,
#44641,#44642,#44643,#44644,#44645,#44646,#44647,#44648,#44649,#44650,#44651,
#44652,#44653,#44654,#44655,#44656,#44657,#44658,#44659,#44660,#44661,#44662,
#44663,#44664,#44665,#44666,#44667),(#44668,#44669,#44670,#44671,#44672,
#44673,#44674,#44675,#44676,#44677,#44678,#44679,#44680,#44681,#44682,#44683,
#44684,#44685,#44686,#44687,#44688,#44689,#44690,#44691,#44692,#44693,#44694,
#44695,#44696,#44697,#44698,#44699,#44700),(#44701,#44702,#44703,#44704,
#44705,#44706,#44707,#44708,#44709,#44710,#44711,#44712,#44713,#44714,#44715,
#44716,#44717,#44718,#44719,#44720,#44721,#44722,#44723,#44724,#44725,#44726,
#44727,#44728,#44729,#44730,#44731,#44732,#44733)),.UNSPECIFIED.,.F.,.F.,
 .F.)
B_SPLINE_SURFACE_WITH_KNOTS((4,4),(4,1,1,1,1,1,1,1,1,1,1,1,1,1,1,1,1,1,
1,1,1,1,1,1,1,1,1,1,1,1,4),(0.108378650282158,0.90358623629129),(-0.009736901743293,
0.,0.02218413179616,0.04656961109721,0.07320227078019,0.1023246073732,0.1343070073132,
0.1695983831374,0.2086113444912,0.2515282384572,0.298570017754,0.3503280366984,
0.407666728873,0.4682132326112,0.5282256466259,0.5849768379281,0.6367767624527,
0.6825350754217,0.7235069669533,0.7605071950843,0.7940293660324,0.8241786597915,
0.8510660708046,0.8750221728306,0.8964633607917,0.915795400779,0.9333737553402,
0.9493579414425,0.9638585657324,0.9770543416126,0.985715500525),
 .UNSPECIFIED.)
GEOMETRIC_REPRESENTATION_ITEM()
RATIONAL_B_SPLINE_SURFACE(((1.07414501661197,1.07414501661197,1.07414501661197,
1.07414501661197,1.07414501661197,1.07414501661197,1.07414501661197,1.07414501661197,
1.07414501661197,1.07414501661197,1.07414501661197,1.07414501661197,1.07414501661197,
1.07414501661197,1.07414501661197,1.07414501661197,1.07414501661197,1.07414501661197,
1.07414501661197,1.07414501661197,1.07414501661197,1.07414501661197,1.07414501661197,
1.07414501661197,1.07414501661197,1.07414501661197,1.07414501661197,1.07414501661197,
1.07414501661197,1.07414501661197,1.07414501661197,1.07414501661197,1.07414501661197),
(0.973774799790487,0.973774799790487,0.973774799790487,0.973774799790487,
0.973774799790487,0.973774799790487,0.973774799790487,0.973774799790487,
0.973774799790487,0.973774799790487,0.973774799790487,0.973774799790487,
0.973774799790487,0.973774799790487,0.973774799790487,0.973774799790487,
0.973774799790487,0.973774799790487,0.973774799790487,0.973774799790487,
0.973774799790487,0.973774799790487,0.973774799790487,0.973774799790487,
0.973774799790487,0.973774799790487,0.973774799790487,0.973774799790487,
0.973774799790487,0.973774799790487,0.973774799790487,0.973774799790487,
0.973774799790487),(0.975308064333504,0.975308064333504,0.975308064333504,
0.975308064333504,0.975308064333504,0.975308064333504,0.975308064333504,
0.975308064333504,0.975308064333504,0.975308064333504,0.975308064333504,
0.975308064333504,0.975308064333504,0.975308064333504,0.975308064333504,
0.975308064333504,0.975308064333504,0.975308064333504,0.975308064333504,
0.975308064333504,0.975308064333504,0.975308064333504,0.975308064333504,
0.975308064333504,0.975308064333504,0.975308064333504,0.975308064333504,
0.975308064333504,0.975308064333504,0.975308064333504,0.975308064333504,
0.975308064333504,0.975308064333504),(1.07874481024102,1.07874481024102,
1.07874481024102,1.07874481024102,1.07874481024102,1.07874481024102,1.07874481024102,
1.07874481024102,1.07874481024102,1.07874481024102,1.07874481024102,1.07874481024102,
1.07874481024102,1.07874481024102,1.07874481024102,1.07874481024102,1.07874481024102,
1.07874481024102,1.07874481024102,1.07874481024102,1.07874481024102,1.07874481024102,
1.07874481024102,1.07874481024102,1.07874481024102,1.07874481024102,1.07874481024102,
1.07874481024102,1.07874481024102,1.07874481024102,1.07874481024102,1.07874481024102,
1.07874481024102)))
REPRESENTATION_ITEM('')
SURFACE()
);
#210=(
BOUNDED_SURFACE()
B_SPLINE_SURFACE(3,3,((#45120,#45121,#45122,#45123,#45124,#45125,#45126,
#45127,#45128,#45129),(#45130,#45131,#45132,#45133,#45134,#45135,#45136,
#45137,#45138,#45139),(#45140,#45141,#45142,#45143,#45144,#45145,#45146,
#45147,#45148,#45149),(#45150,#45151,#45152,#45153,#45154,#45155,#45156,
#45157,#45158,#45159)),.UNSPECIFIED.,.F.,.F.,.F.)
B_SPLINE_SURFACE_WITH_KNOTS((4,4),(4,1,1,1,1,1,1,4),(0.0576542468391072,
0.942338471723155),(0.2949063013325,0.3507658351833,0.4113946127403,0.470739629438,
0.5289312325493,0.5882633205163,0.6488928044224,0.7051344531532),
 .UNSPECIFIED.)
GEOMETRIC_REPRESENTATION_ITEM()
RATIONAL_B_SPLINE_SURFACE(((1.19330101599729,1.19330101599729,1.19330101599729,
1.19330101599729,1.19330101599729,1.19330101599729,1.19330101599729,1.19330101599729,
1.19330101599729,1.19330101599729),(0.935568449281609,0.935568449281609,
0.935568449281609,0.935568449281609,0.935568449281609,0.935568449281609,
0.935568449281609,0.935568449281609,0.935568449281609,0.935568449281609),
(0.935566328018295,0.935566328018295,0.935566328018295,0.935566328018295,
0.935566328018295,0.935566328018295,0.935566328018295,0.935566328018295,
0.935566328018295,0.935566328018295),(1.19329465220735,1.19329465220735,
1.19329465220735,1.19329465220735,1.19329465220735,1.19329465220735,1.19329465220735,
1.19329465220735,1.19329465220735,1.19329465220735)))
REPRESENTATION_ITEM('')
SURFACE()
);
#211=(
BOUNDED_SURFACE()
B_SPLINE_SURFACE(3,3,((#45250,#45251,#45252,#45253,#45254,#45255,#45256,
#45257,#45258),(#45259,#45260,#45261,#45262,#45263,#45264,#45265,#45266,
#45267),(#45268,#45269,#45270,#45271,#45272,#45273,#45274,#45275,#45276),
(#45277,#45278,#45279,#45280,#45281,#45282,#45283,#45284,#45285)),
 .UNSPECIFIED.,.F.,.F.,.F.)
B_SPLINE_SURFACE_WITH_KNOTS((4,4),(4,1,1,1,1,1,4),(0.0549539789496563,0.945047550786385),
(0.225999549185134,0.2426046586147,0.359632647929,0.4760208069216,0.5903747960474,
0.7008431878989,0.773895646058005),.UNSPECIFIED.)
GEOMETRIC_REPRESENTATION_ITEM()
RATIONAL_B_SPLINE_SURFACE(((1.19567368239687,1.19567368239687,1.19567368239687,
1.19567368239687,1.19567368239687,1.19567368239687,1.19567368239687,1.19567368239687,
1.19567368239687),(0.934774990814295,0.934774990814295,0.934774990814295,
0.934774990814295,0.934774990814295,0.934774990814295,0.934774990814295,
0.934774990814295,0.934774990814295),(0.93477543920178,0.93477543920178,
0.93477543920178,0.93477543920178,0.93477543920178,0.93477543920178,0.93477543920178,
0.93477543920178,0.93477543920178),(1.19567502755933,1.19567502755933,1.19567502755933,
1.19567502755933,1.19567502755933,1.19567502755933,1.19567502755933,1.19567502755933,
1.19567502755933)))
REPRESENTATION_ITEM('')
SURFACE()
);
#212=(
BOUNDED_SURFACE()
B_SPLINE_SURFACE(3,3,((#45402,#45403,#45404,#45405,#45406,#45407,#45408,
#45409,#45410,#45411),(#45412,#45413,#45414,#45415,#45416,#45417,#45418,
#45419,#45420,#45421),(#45422,#45423,#45424,#45425,#45426,#45427,#45428,
#45429,#45430,#45431),(#45432,#45433,#45434,#45435,#45436,#45437,#45438,
#45439,#45440,#45441)),.UNSPECIFIED.,.F.,.F.,.F.)
B_SPLINE_SURFACE_WITH_KNOTS((4,4),(4,1,1,1,1,1,1,4),(0.0902151502653892,
0.906139739364474),(0.0113422875341,0.1428793791643,0.2858116106518,0.4286834137584,
0.5714931631331,0.7143130817917,0.857293314129,0.9764111906614),
 .UNSPECIFIED.)
GEOMETRIC_REPRESENTATION_ITEM()
RATIONAL_B_SPLINE_SURFACE(((1.11548012320919,1.11548012320919,1.11548012320919,
1.11548012320919,1.11548012320919,1.11548012320919,1.11548012320919,1.11548012320919,
1.11548012320919,1.11548012320919),(0.962191436654982,0.962191436654982,
0.962191436654982,0.962191436654982,0.962191436654982,0.962191436654982,
0.962191436654982,0.962191436654982,0.962191436654982,0.962191436654982),
(0.961509671356259,0.961509671356259,0.961509671356259,0.961509671356259,
0.961509671356259,0.961509671356259,0.961509671356259,0.961509671356259,
0.961509671356259,0.961509671356259),(1.11343482731302,1.11343482731302,
1.11343482731302,1.11343482731302,1.11343482731302,1.11343482731302,1.11343482731302,
1.11343482731302,1.11343482731302,1.11343482731302)))
REPRESENTATION_ITEM('')
SURFACE()
);
#213=(
BOUNDED_SURFACE()
B_SPLINE_SURFACE(3,3,((#45468,#45469,#45470,#45471,#45472,#45473,#45474,
#45475),(#45476,#45477,#45478,#45479,#45480,#45481,#45482,#45483),(#45484,
#45485,#45486,#45487,#45488,#45489,#45490,#45491),(#45492,#45493,#45494,
#45495,#45496,#45497,#45498,#45499)),.UNSPECIFIED.,.F.,.F.,.F.)
B_SPLINE_SURFACE_WITH_KNOTS((4,4),(4,1,1,1,1,4),(0.0538108527545732,0.94619037239879),
(0.229096267158528,0.3087140271309,0.421124754351,0.5382875231502,0.659432849143,
0.77499777021192),.UNSPECIFIED.)
GEOMETRIC_REPRESENTATION_ITEM()
RATIONAL_B_SPLINE_SURFACE(((1.19668201979503,1.19668201979503,1.19668201979503,
1.19668201979503,1.19668201979503,1.19668201979503,1.19668201979503,1.19668201979503),
(0.934438966699946,0.934438966699946,0.934438966699946,0.934438966699946,
0.934438966699946,0.934438966699946,0.934438966699946,0.934438966699946),
(0.93443932673555,0.93443932673555,0.93443932673555,0.93443932673555,0.93443932673555,
0.93443932673555,0.93443932673555,0.93443932673555),(1.19668309990185,1.19668309990185,
1.19668309990185,1.19668309990185,1.19668309990185,1.19668309990185,1.19668309990185,
1.19668309990185)))
REPRESENTATION_ITEM('')
SURFACE()
);
#214=(
BOUNDED_SURFACE()
B_SPLINE_SURFACE(3,3,((#45616,#45617,#45618,#45619,#45620,#45621,#45622,
#45623,#45624,#45625),(#45626,#45627,#45628,#45629,#45630,#45631,#45632,
#45633,#45634,#45635),(#45636,#45637,#45638,#45639,#45640,#45641,#45642,
#45643,#45644,#45645),(#45646,#45647,#45648,#45649,#45650,#45651,#45652,
#45653,#45654,#45655)),.UNSPECIFIED.,.F.,.F.,.F.)
B_SPLINE_SURFACE_WITH_KNOTS((4,4),(4,1,1,1,1,1,1,4),(0.0902467380234992,
0.903452489290608),(0.02358777780153,0.1427066858466,0.2856869182934,0.4285068377462,
0.5713165853686,0.7141883873726,0.8571206201588,0.9886565450661),
 .UNSPECIFIED.)
GEOMETRIC_REPRESENTATION_ITEM()
RATIONAL_B_SPLINE_SURFACE(((1.11546232169106,1.11546232169106,1.11546232169106,
1.11546232169106,1.11546232169106,1.11546232169106,1.11546232169106,1.11546232169106,
1.11546232169106,1.11546232169106),(0.962696201577782,0.962696201577782,
0.962696201577782,0.962696201577782,0.962696201577782,0.962696201577782,
0.962696201577782,0.962696201577782,0.962696201577782,0.962696201577782),
(0.961521659864195,0.961521659864195,0.961521659864195,0.961521659864195,
0.961521659864195,0.961521659864195,0.961521659864195,0.961521659864195,
0.961521659864195,0.961521659864195),(1.1119386965503,1.1119386965503,1.1119386965503,
1.1119386965503,1.1119386965503,1.1119386965503,1.1119386965503,1.1119386965503,
1.1119386965503,1.1119386965503)))
REPRESENTATION_ITEM('')
SURFACE()
);
#215=(
BOUNDED_SURFACE()
B_SPLINE_SURFACE(3,3,((#45695,#45696,#45697,#45698,#45699,#45700),(#45701,
#45702,#45703,#45704,#45705,#45706),(#45707,#45708,#45709,#45710,#45711,
#45712),(#45713,#45714,#45715,#45716,#45717,#45718)),.UNSPECIFIED.,.F.,
 .F.,.F.)
B_SPLINE_SURFACE_WITH_KNOTS((4,4),(4,1,1,4),(0.0986342191388391,0.901369959991362),
(0.317543733196465,0.3333147448852,0.6666852551147,0.682456266811625),
 .UNSPECIFIED.)
GEOMETRIC_REPRESENTATION_ITEM()
RATIONAL_B_SPLINE_SURFACE(((1.17563408853202,1.17563408853202,1.17563408853202,
1.17563408853202,1.17563408853202,1.17563408853202),(0.941454084656006,
0.941454084656006,0.941454084656006,0.941454084656006,0.941454084656006,
0.941454084656006),(0.941455303829106,0.941455303829106,0.941455303829106,
0.941455303829106,0.941455303829106,0.941455303829106),(1.17563774605132,
1.17563774605132,1.17563774605132,1.17563774605132,1.17563774605132,1.17563774605132)))
REPRESENTATION_ITEM('')
SURFACE()
);
#216=(
BOUNDED_SURFACE()
B_SPLINE_SURFACE(3,3,((#45958,#45959,#45960,#45961,#45962,#45963,#45964,
#45965,#45966,#45967,#45968,#45969,#45970,#45971,#45972,#45973,#45974,#45975,
#45976,#45977,#45978,#45979,#45980,#45981,#45982,#45983,#45984,#45985,#45986,
#45987,#45988,#45989,#45990,#45991,#45992,#45993,#45994,#45995,#45996,#45997),
(#45998,#45999,#46000,#46001,#46002,#46003,#46004,#46005,#46006,#46007,
#46008,#46009,#46010,#46011,#46012,#46013,#46014,#46015,#46016,#46017,#46018,
#46019,#46020,#46021,#46022,#46023,#46024,#46025,#46026,#46027,#46028,#46029,
#46030,#46031,#46032,#46033,#46034,#46035,#46036,#46037),(#46038,#46039,
#46040,#46041,#46042,#46043,#46044,#46045,#46046,#46047,#46048,#46049,#46050,
#46051,#46052,#46053,#46054,#46055,#46056,#46057,#46058,#46059,#46060,#46061,
#46062,#46063,#46064,#46065,#46066,#46067,#46068,#46069,#46070,#46071,#46072,
#46073,#46074,#46075,#46076,#46077),(#46078,#46079,#46080,#46081,#46082,
#46083,#46084,#46085,#46086,#46087,#46088,#46089,#46090,#46091,#46092,#46093,
#46094,#46095,#46096,#46097,#46098,#46099,#46100,#46101,#46102,#46103,#46104,
#46105,#46106,#46107,#46108,#46109,#46110,#46111,#46112,#46113,#46114,#46115,
#46116,#46117)),.UNSPECIFIED.,.F.,.F.,.F.)
B_SPLINE_SURFACE_WITH_KNOTS((4,4),(4,1,1,1,1,1,1,1,1,1,1,1,1,1,1,1,1,1,
1,1,1,1,1,1,1,1,1,1,1,1,1,1,1,1,1,1,1,4),(0.109557621894297,0.885243870276793),
(-0.009601789273476,0.,0.02232833549642,0.04690550208409,0.0737936246764,
0.1032829469292,0.1358149659664,0.1719129604536,0.2120204765653,0.256254955895,
0.3048250014022,0.3583933178747,0.4161357109072,0.4734125795356,0.5265814299979,
0.5739176940624,0.615519024704,0.652991192313,0.6871377766576,0.7180210170715,
0.7460333746096,0.7715274743224,0.7947401813882,0.8158383097162,0.8349870800801,
0.8523592732018,0.8681377597697,0.8825020836392,0.8956292723193,0.907695283691,
0.9188455009777,0.9291452784588,0.9386432333898,0.9473858993637,0.9554254804025,
0.9628154053196,0.9696060115487,0.972066289616),.UNSPECIFIED.)
GEOMETRIC_REPRESENTATION_ITEM()
RATIONAL_B_SPLINE_SURFACE(((1.07369790078242,1.07369790078242,1.07369790078242,
1.07369790078242,1.07369790078242,1.07369790078242,1.07369790078242,1.07369790078242,
1.07369790078242,1.07369790078242,1.07369790078242,1.07369790078242,1.07369790078242,
1.07369790078242,1.07369790078242,1.07369790078242,1.07369790078242,1.07369790078242,
1.07369790078242,1.07369790078242,1.07369790078242,1.07369790078242,1.07369790078242,
1.07369790078242,1.07369790078242,1.07369790078242,1.07369790078242,1.07369790078242,
1.07369790078242,1.07369790078242,1.07369790078242,1.07369790078242,1.07369790078242,
1.07369790078242,1.07369790078242,1.07369790078242,1.07369790078242,1.07369790078242,
1.07369790078242,1.07369790078242),(0.976088195522974,0.976088195522974,
0.976088195522974,0.976088195522974,0.976088195522974,0.976088195522974,
0.976088195522974,0.976088195522974,0.976088195522974,0.976088195522974,
0.976088195522974,0.976088195522974,0.976088195522974,0.976088195522974,
0.976088195522974,0.976088195522974,0.976088195522974,0.976088195522974,
0.976088195522974,0.976088195522974,0.976088195522974,0.976088195522974,
0.976088195522974,0.976088195522974,0.976088195522974,0.976088195522974,
0.976088195522974,0.976088195522974,0.976088195522974,0.976088195522974,
0.976088195522974,0.976088195522974,0.976088195522974,0.976088195522974,
0.976088195522974,0.976088195522974,0.976088195522974,0.976088195522974,
0.976088195522974,0.976088195522974),(0.97543838796439,0.97543838796439,
0.97543838796439,0.97543838796439,0.97543838796439,0.97543838796439,0.97543838796439,
0.97543838796439,0.97543838796439,0.97543838796439,0.97543838796439,0.97543838796439,
0.97543838796439,0.97543838796439,0.97543838796439,0.97543838796439,0.97543838796439,
0.97543838796439,0.97543838796439,0.97543838796439,0.97543838796439,0.97543838796439,
0.97543838796439,0.97543838796439,0.97543838796439,0.97543838796439,0.97543838796439,
0.97543838796439,0.97543838796439,0.97543838796439,0.97543838796439,0.97543838796439,
0.97543838796439,0.97543838796439,0.97543838796439,0.97543838796439,0.97543838796439,
0.97543838796439,0.97543838796439,0.97543838796439),(1.07174847810667,1.07174847810667,
1.07174847810667,1.07174847810667,1.07174847810667,1.07174847810667,1.07174847810667,
1.07174847810667,1.07174847810667,1.07174847810667,1.07174847810667,1.07174847810667,
1.07174847810667,1.07174847810667,1.07174847810667,1.07174847810667,1.07174847810667,
1.07174847810667,1.07174847810667,1.07174847810667,1.07174847810667,1.07174847810667,
1.07174847810667,1.07174847810667,1.07174847810667,1.07174847810667,1.07174847810667,
1.07174847810667,1.07174847810667,1.07174847810667,1.07174847810667,1.07174847810667,
1.07174847810667,1.07174847810667,1.07174847810667,1.07174847810667,1.07174847810667,
1.07174847810667,1.07174847810667,1.07174847810667)))
REPRESENTATION_ITEM('')
SURFACE()
);
#217=(
BOUNDED_SURFACE()
B_SPLINE_SURFACE(3,3,((#46243,#46244,#46245,#46246,#46247,#46248,#46249,
#46250),(#46251,#46252,#46253,#46254,#46255,#46256,#46257,#46258),(#46259,
#46260,#46261,#46262,#46263,#46264,#46265,#46266),(#46267,#46268,#46269,
#46270,#46271,#46272,#46273,#46274)),.UNSPECIFIED.,.F.,.F.,.F.)
B_SPLINE_SURFACE_WITH_KNOTS((4,4),(4,1,1,1,1,4),(0.0538140162332302,0.946187598359706),
(0.226399629870169,0.3386790291836,0.4601779185567,0.5776891459497,0.6904350358172,
0.773432296606802),.UNSPECIFIED.)
GEOMETRIC_REPRESENTATION_ITEM()
RATIONAL_B_SPLINE_SURFACE(((1.19667979358655,1.19667979358655,1.19667979358655,
1.19667979358655,1.19667979358655,1.19667979358655,1.19667979358655,1.19667979358655),
(0.934439594326999,0.934439594326999,0.934439594326999,0.934439594326999,
0.934439594326999,0.934439594326999,0.934439594326999,0.934439594326999),
(0.934440068805344,0.934440068805343,0.934440068805343,0.934440068805343,
0.934440068805343,0.934440068805343,0.934440068805343,0.934440068805343),
(1.19668121702158,1.19668121702158,1.19668121702158,1.19668121702158,1.19668121702158,
1.19668121702158,1.19668121702158,1.19668121702158)))
REPRESENTATION_ITEM('')
SURFACE()
);
#218=(
BOUNDED_SURFACE()
B_SPLINE_SURFACE(3,3,((#46394,#46395,#46396,#46397,#46398,#46399,#46400,
#46401,#46402,#46403),(#46404,#46405,#46406,#46407,#46408,#46409,#46410,
#46411,#46412,#46413),(#46414,#46415,#46416,#46417,#46418,#46419,#46420,
#46421,#46422,#46423),(#46424,#46425,#46426,#46427,#46428,#46429,#46430,
#46431,#46432,#46433)),.UNSPECIFIED.,.F.,.F.,.F.)
B_SPLINE_SURFACE_WITH_KNOTS((4,4),(4,1,1,1,1,1,1,4),(0.0889032005159359,
0.902793520014641),(0.02295305876274,0.1427319133548,0.2857218418975,0.4285793286892,
0.5713517372348,0.7142096687795,0.8572807309771,0.9622634166072),
 .UNSPECIFIED.)
GEOMETRIC_REPRESENTATION_ITEM()
RATIONAL_B_SPLINE_SURFACE(((1.11579304262805,1.11579304262805,1.11579304262805,
1.11579304262805,1.11579304262805,1.11579304262805,1.11579304262805,1.11579304262805,
1.11579304262805,1.11579304262805),(0.962961500959473,0.962961500959473,
0.962961500959473,0.962961500959473,0.962961500959473,0.962961500959473,
0.962961500959473,0.962961500959473,0.962961500959473,0.962961500959473),
(0.961418065199563,0.961418065199563,0.961418065199563,0.961418065199563,
0.961418065199563,0.961418065199563,0.961418065199563,0.961418065199563,
0.961418065199563,0.961418065199563),(1.11116273534832,1.11116273534832,
1.11116273534832,1.11116273534832,1.11116273534832,1.11116273534832,1.11116273534832,
1.11116273534832,1.11116273534832,1.11116273534832)))
REPRESENTATION_ITEM('')
SURFACE()
);
#219=(
BOUNDED_SURFACE()
B_SPLINE_SURFACE(3,3,((#46652,#46653,#46654,#46655,#46656,#46657,#46658,
#46659,#46660,#46661),(#46662,#46663,#46664,#46665,#46666,#46667,#46668,
#46669,#46670,#46671),(#46672,#46673,#46674,#46675,#46676,#46677,#46678,
#46679,#46680,#46681),(#46682,#46683,#46684,#46685,#46686,#46687,#46688,
#46689,#46690,#46691)),.UNSPECIFIED.,.F.,.F.,.F.)
B_SPLINE_SURFACE_WITH_KNOTS((4,4),(4,1,1,1,1,1,1,4),(0.0566082084903071,
0.943377877952831),(0.294866436509,0.3476249436887,0.4099876923829,0.4703085802384,
0.5297603546224,0.5900842016518,0.6524504076229,0.7051016030693),
 .UNSPECIFIED.)
GEOMETRIC_REPRESENTATION_ITEM()
RATIONAL_B_SPLINE_SURFACE(((1.19421794191571,1.19421794191571,1.19421794191571,
1.19421794191571,1.19421794191571,1.19421794191571,1.19421794191571,1.19421794191571,
1.19421794191571,1.19421794191571),(0.935264749044728,0.935264749044728,
0.935264749044728,0.935264749044728,0.935264749044728,0.935264749044728,
0.935264749044728,0.935264749044728,0.935264749044728,0.935264749044728),
(0.935260686091779,0.935260686091779,0.935260686091779,0.935260686091779,
0.935260686091779,0.935260686091779,0.935260686091779,0.935260686091779,
0.935260686091779,0.935260686091779),(1.19420575305686,1.19420575305686,
1.19420575305686,1.19420575305686,1.19420575305686,1.19420575305686,1.19420575305686,
1.19420575305686,1.19420575305686,1.19420575305686)))
REPRESENTATION_ITEM('')
SURFACE()
);
#220=(
BOUNDED_SURFACE()
B_SPLINE_SURFACE(3,3,((#46787,#46788,#46789,#46790),(#46791,#46792,#46793,
#46794),(#46795,#46796,#46797,#46798),(#46799,#46800,#46801,#46802)),
 .UNSPECIFIED.,.F.,.F.,.F.)
B_SPLINE_SURFACE_WITH_KNOTS((4,4),(4,4),(0.0986320320012492,0.901362552769613),
(-0.975145040391543,-0.0991746183696281),.UNSPECIFIED.)
GEOMETRIC_REPRESENTATION_ITEM()
RATIONAL_B_SPLINE_SURFACE(((1.1756360043584,1.1756360043584,1.1756360043584,
1.1756360043584),(0.94145624499323,0.94145624499323,0.94145624499323,0.94145624499323),
(0.941454665224592,0.941454665224592,0.941454665224592,0.941454665224592),
(1.17563126505248,1.17563126505248,1.17563126505248,1.17563126505248)))
REPRESENTATION_ITEM('')
SURFACE()
);
#221=(
BOUNDED_SURFACE()
B_SPLINE_SURFACE(3,3,((#46821,#46822,#46823,#46824,#46825,#46826,#46827,
#46828,#46829,#46830,#46831),(#46832,#46833,#46834,#46835,#46836,#46837,
#46838,#46839,#46840,#46841,#46842),(#46843,#46844,#46845,#46846,#46847,
#46848,#46849,#46850,#46851,#46852,#46853),(#46854,#46855,#46856,#46857,
#46858,#46859,#46860,#46861,#46862,#46863,#46864)),.UNSPECIFIED.,.F.,.F.,
 .F.)
B_SPLINE_SURFACE_WITH_KNOTS((4,4),(4,1,1,1,1,1,1,1,4),(0.0753633925353489,
0.90355881590316),(-0.009670337421385,0.,0.1430991485311,0.2858285059199,
0.4284781713031,0.5715215149008,0.7145472299923,0.8573672624017,0.9759160460961),
 .UNSPECIFIED.)
GEOMETRIC_REPRESENTATION_ITEM()
RATIONAL_B_SPLINE_SURFACE(((1.12354604889356,1.12354604889356,1.12354604889356,
1.12354604889356,1.12354604889356,1.12354604889356,1.12354604889356,1.12354604889356,
1.12354604889356,1.12354604889356,1.12354604889356),(0.962906307414026,
0.962906307414026,0.962906307414026,0.962906307414026,0.962906307414026,
0.962906307414026,0.962906307414026,0.962906307414026,0.962906307414026,
0.962906307414026,0.962906307414026),(0.958919450266201,0.958919450266201,
0.958919450266201,0.958919450266201,0.958919450266201,0.958919450266201,
0.958919450266201,0.958919450266201,0.958919450266201,0.958919450266201,
0.958919450266201),(1.11158547745009,1.11158547745009,1.11158547745009,
1.11158547745009,1.11158547745009,1.11158547745009,1.11158547745009,1.11158547745009,
1.11158547745009,1.11158547745009,1.11158547745009)))
REPRESENTATION_ITEM('')
SURFACE()
);
#222=(
BOUNDED_SURFACE()
B_SPLINE_SURFACE(3,3,((#47032,#47033,#47034,#47035,#47036,#47037,#47038,
#47039,#47040),(#47041,#47042,#47043,#47044,#47045,#47046,#47047,#47048,
#47049),(#47050,#47051,#47052,#47053,#47054,#47055,#47056,#47057,#47058),
(#47059,#47060,#47061,#47062,#47063,#47064,#47065,#47066,#47067)),
 .UNSPECIFIED.,.F.,.F.,.F.)
B_SPLINE_SURFACE_WITH_KNOTS((4,4),(4,1,1,1,1,1,4),(0.0545899833427553,0.945411009430165),
(0.226573738413812,0.3006458185641,0.409865708208,0.5233967602136,0.6403051050053,
0.7591301880906,0.77297490226788),.UNSPECIFIED.)
GEOMETRIC_REPRESENTATION_ITEM()
RATIONAL_B_SPLINE_SURFACE(((1.19599304937649,1.19599304937649,1.19599304937649,
1.19599304937649,1.19599304937649,1.19599304937649,1.19599304937649,1.19599304937649,
1.19599304937649),(0.934668692308928,0.934668692308928,0.934668692308928,
0.934668692308928,0.934668692308928,0.934668692308928,0.934668692308928,
0.934668692308928,0.934668692308928),(0.934668983541427,0.934668983541427,
0.934668983541427,0.934668983541427,0.934668983541427,0.934668983541427,
0.934668983541427,0.934668983541427,0.934668983541427),(1.19599392307399,
1.19599392307399,1.19599392307399,1.19599392307399,1.19599392307399,1.19599392307399,
1.19599392307399,1.19599392307399,1.19599392307399)))
REPRESENTATION_ITEM('')
SURFACE()
);
#223=(
BOUNDED_SURFACE()
B_SPLINE_SURFACE(3,3,((#47118,#47119,#47120,#47121,#47122,#47123,#47124,
#47125,#47126,#47127),(#47128,#47129,#47130,#47131,#47132,#47133,#47134,
#47135,#47136,#47137),(#47138,#47139,#47140,#47141,#47142,#47143,#47144,
#47145,#47146,#47147),(#47148,#47149,#47150,#47151,#47152,#47153,#47154,
#47155,#47156,#47157)),.UNSPECIFIED.,.F.,.F.,.F.)
B_SPLINE_SURFACE_WITH_KNOTS((4,4),(4,1,1,1,1,1,1,4),(0.0573875678003812,
0.942600786703194),(0.2949023604086,0.3473747858184,0.4097087132847,0.4701865626765,
0.5297465130048,0.5902215650413,0.6525525187134,0.7051382449586),
 .UNSPECIFIED.)
GEOMETRIC_REPRESENTATION_ITEM()
RATIONAL_B_SPLINE_SURFACE(((1.19353520188251,1.19353520188251,1.19353520188251,
1.19353520188251,1.19353520188251,1.19353520188251,1.19353520188251,1.19353520188251,
1.19353520188251,1.19353520188251),(0.935491660752717,0.935491660752717,
0.935491660752717,0.935491660752717,0.935491660752717,0.935491660752717,
0.935491660752717,0.935491660752717,0.935491660752717,0.935491660752717),
(0.935488266084021,0.935488266084021,0.935488266084021,0.935488266084021,
0.935488266084021,0.935488266084021,0.935488266084021,0.935488266084021,
0.935488266084021,0.935488266084021),(1.19352501787643,1.19352501787643,
1.19352501787643,1.19352501787643,1.19352501787643,1.19352501787643,1.19352501787643,
1.19352501787643,1.19352501787643,1.19352501787643)))
REPRESENTATION_ITEM('')
SURFACE()
);
#224=(
BOUNDED_SURFACE()
B_SPLINE_SURFACE(3,3,((#47465,#47466,#47467,#47468,#47469,#47470,#47471,
#47472,#47473,#47474,#47475,#47476,#47477,#47478,#47479,#47480,#47481,#47482,
#47483,#47484,#47485,#47486,#47487,#47488,#47489,#47490,#47491,#47492,#47493,
#47494,#47495,#47496,#47497),(#47498,#47499,#47500,#47501,#47502,#47503,
#47504,#47505,#47506,#47507,#47508,#47509,#47510,#47511,#47512,#47513,#47514,
#47515,#47516,#47517,#47518,#47519,#47520,#47521,#47522,#47523,#47524,#47525,
#47526,#47527,#47528,#47529,#47530),(#47531,#47532,#47533,#47534,#47535,
#47536,#47537,#47538,#47539,#47540,#47541,#47542,#47543,#47544,#47545,#47546,
#47547,#47548,#47549,#47550,#47551,#47552,#47553,#47554,#47555,#47556,#47557,
#47558,#47559,#47560,#47561,#47562,#47563),(#47564,#47565,#47566,#47567,
#47568,#47569,#47570,#47571,#47572,#47573,#47574,#47575,#47576,#47577,#47578,
#47579,#47580,#47581,#47582,#47583,#47584,#47585,#47586,#47587,#47588,#47589,
#47590,#47591,#47592,#47593,#47594,#47595,#47596)),.UNSPECIFIED.,.F.,.F.,
 .F.)
B_SPLINE_SURFACE_WITH_KNOTS((4,4),(4,1,1,1,1,1,1,1,1,1,1,1,1,1,1,1,1,1,
1,1,1,1,1,1,1,1,1,1,1,1,4),(0.108387652276654,0.903585982346435),(-0.00973690173883,
0.,0.02218340749114,0.04656850383599,0.0732012163466,0.102323831163,0.1343066238718,
0.1695984990841,0.2086121558901,0.2515303853581,0.298574638964,0.3503366286747,
0.4076785718675,0.4682255700403,0.5282360307647,0.5849839255341,0.6367806003876,
0.6825368401862,0.7235074075035,0.7605068126486,0.7940285468258,0.8241776680749,
0.8510650518271,0.8750212083659,0.8964625051051,0.9157946807002,0.9333731860453,
0.9493575699013,0.9638584550805,0.9770544701579,0.9857155005173),
 .UNSPECIFIED.)
GEOMETRIC_REPRESENTATION_ITEM()
RATIONAL_B_SPLINE_SURFACE(((1.07414161106479,1.07414161106479,1.07414161106479,
1.07414161106479,1.07414161106479,1.07414161106479,1.07414161106479,1.07414161106479,
1.07414161106479,1.07414161106479,1.07414161106479,1.07414161106479,1.07414161106479,
1.07414161106479,1.07414161106479,1.07414161106479,1.07414161106479,1.07414161106479,
1.07414161106479,1.07414161106479,1.07414161106479,1.07414161106479,1.07414161106479,
1.07414161106479,1.07414161106479,1.07414161106479,1.07414161106479,1.07414161106479,
1.07414161106479,1.07414161106479,1.07414161106479,1.07414161106479,1.07414161106479),
(0.973774865480363,0.973774865480363,0.973774865480363,0.973774865480363,
0.973774865480363,0.973774865480363,0.973774865480363,0.973774865480363,
0.973774865480363,0.973774865480363,0.973774865480363,0.973774865480363,
0.973774865480363,0.973774865480363,0.973774865480363,0.973774865480363,
0.973774865480363,0.973774865480363,0.973774865480363,0.973774865480363,
0.973774865480363,0.973774865480363,0.973774865480363,0.973774865480363,
0.973774865480363,0.973774865480363,0.973774865480363,0.973774865480363,
0.973774865480363,0.973774865480363,0.973774865480363,0.973774865480363,
0.973774865480363),(0.975309233263865,0.975309233263865,0.975309233263865,
0.975309233263865,0.975309233263865,0.975309233263865,0.975309233263865,
0.975309233263865,0.975309233263865,0.975309233263865,0.975309233263865,
0.975309233263865,0.975309233263865,0.975309233263865,0.975309233263865,
0.975309233263865,0.975309233263865,0.975309233263865,0.975309233263865,
0.975309233263865,0.975309233263865,0.975309233263865,0.975309233263865,
0.975309233263865,0.975309233263865,0.975309233263865,0.975309233263865,
0.975309233263865,0.975309233263865,0.975309233263865,0.975309233263865,
0.975309233263865,0.975309233263865),(1.0787447144153,1.0787447144153,1.0787447144153,
1.0787447144153,1.0787447144153,1.0787447144153,1.0787447144153,1.0787447144153,
1.0787447144153,1.0787447144153,1.0787447144153,1.0787447144153,1.0787447144153,
1.0787447144153,1.0787447144153,1.0787447144153,1.0787447144153,1.0787447144153,
1.0787447144153,1.0787447144153,1.0787447144153,1.0787447144153,1.0787447144153,
1.0787447144153,1.0787447144153,1.0787447144153,1.0787447144153,1.0787447144153,
1.0787447144153,1.0787447144153,1.0787447144153,1.0787447144153,1.0787447144153)))
REPRESENTATION_ITEM('')
SURFACE()
);
#225=(
BOUNDED_SURFACE()
B_SPLINE_SURFACE(3,3,((#47691,#47692,#47693,#47694,#47695,#47696,#47697,
#47698,#47699,#47700),(#47701,#47702,#47703,#47704,#47705,#47706,#47707,
#47708,#47709,#47710),(#47711,#47712,#47713,#47714,#47715,#47716,#47717,
#47718,#47719,#47720),(#47721,#47722,#47723,#47724,#47725,#47726,#47727,
#47728,#47729,#47730)),.UNSPECIFIED.,.F.,.F.,.F.)
B_SPLINE_SURFACE_WITH_KNOTS((4,4),(4,1,1,1,1,1,1,4),(0.0902161588351993,
0.903852934841359),(0.01134228752764,0.1428794983947,0.2858119429636,0.4286835294563,
0.5714929704347,0.7143131105204,0.8572933443558,0.9764111906647),
 .UNSPECIFIED.)
GEOMETRIC_REPRESENTATION_ITEM()
RATIONAL_B_SPLINE_SURFACE(((1.115479554767,1.115479554767,1.115479554767,
1.115479554767,1.115479554767,1.115479554767,1.115479554767,1.115479554767,
1.115479554767,1.115479554767),(0.96262105849538,0.96262105849538,0.96262105849538,
0.96262105849538,0.96262105849538,0.96262105849538,0.96262105849538,0.96262105849538,
0.96262105849538,0.96262105849538),(0.96151487844256,0.96151487844256,0.96151487844256,
0.96151487844256,0.96151487844256,0.96151487844256,0.96151487844256,0.96151487844256,
0.96151487844256,0.96151487844256),(1.11216101460854,1.11216101460854,1.11216101460854,
1.11216101460854,1.11216101460854,1.11216101460854,1.11216101460854,1.11216101460854,
1.11216101460854,1.11216101460854)))
REPRESENTATION_ITEM('')
SURFACE()
);
#226=(
BOUNDED_SURFACE()
B_SPLINE_SURFACE(3,3,((#47806,#47807,#47808,#47809,#47810,#47811,#47812,
#47813,#47814),(#47815,#47816,#47817,#47818,#47819,#47820,#47821,#47822,
#47823),(#47824,#47825,#47826,#47827,#47828,#47829,#47830,#47831,#47832),
(#47833,#47834,#47835,#47836,#47837,#47838,#47839,#47840,#47841)),
 .UNSPECIFIED.,.F.,.F.,.F.)
B_SPLINE_SURFACE_WITH_KNOTS((4,4),(4,1,1,1,1,1,4),(0.0546747561307775,0.945326746030744),
(0.22573546897307,0.241174738978,0.3599582619168,0.4768206617324,0.5903023688699,
0.699474730988,0.773102378452142),.UNSPECIFIED.)
GEOMETRIC_REPRESENTATION_ITEM()
RATIONAL_B_SPLINE_SURFACE(((1.19591932446267,1.19591932446267,1.19591932446267,
1.19591932446267,1.19591932446267,1.19591932446267,1.19591932446267,1.19591932446267,
1.19591932446267),(0.934693117931845,0.934693117931846,0.934693117931845,
0.934693117931845,0.934693117931845,0.934693117931845,0.934693117931845,
0.934693117931845,0.934693117931845),(0.934693558513152,0.934693558513152,
0.934693558513152,0.934693558513152,0.934693558513152,0.934693558513152,
0.934693558513152,0.934693558513152,0.934693558513152),(1.19592064620659,
1.19592064620659,1.19592064620659,1.19592064620659,1.19592064620659,1.19592064620659,
1.19592064620659,1.19592064620659,1.19592064620659)))
REPRESENTATION_ITEM('')
SURFACE()
);
#227=(
BOUNDED_SURFACE()
B_SPLINE_SURFACE(3,3,((#47899,#47900,#47901,#47902,#47903,#47904,#47905,
#47906,#47907),(#47908,#47909,#47910,#47911,#47912,#47913,#47914,#47915,
#47916),(#47917,#47918,#47919,#47920,#47921,#47922,#47923,#47924,#47925),
(#47926,#47927,#47928,#47929,#47930,#47931,#47932,#47933,#47934)),
 .UNSPECIFIED.,.F.,.F.,.F.)
B_SPLINE_SURFACE_WITH_KNOTS((4,4),(4,1,1,1,1,1,4),(0.0546340546499548,0.945366954784258),
(0.0404198562176404,0.1289115432366,0.2650470428868,0.4067050538029,0.552064790134,
0.7002092373436,0.711879622175772),.UNSPECIFIED.)
GEOMETRIC_REPRESENTATION_ITEM()
RATIONAL_B_SPLINE_SURFACE(((1.19595478336993,1.19595478336993,1.19595478336993,
1.19595478336993,1.19595478336993,1.19595478336993,1.19595478336993,1.19595478336993,
1.19595478336993),(0.934681442785239,0.934681442785239,0.934681442785239,
0.934681442785239,0.934681442785239,0.934681442785239,0.934681442785239,
0.934681442785239,0.934681442785239),(0.934681738876859,0.934681738876859,
0.93468173887686,0.934681738876859,0.934681738876859,0.934681738876859,
0.934681738876859,0.934681738876859,0.934681738876859),(1.19595567164479,
1.19595567164479,1.19595567164479,1.19595567164479,1.19595567164479,1.19595567164479,
1.19595567164479,1.19595567164479,1.19595567164479)))
REPRESENTATION_ITEM('')
SURFACE()
);
#228=(
BOUNDED_SURFACE()
B_SPLINE_SURFACE(3,3,((#48048,#48049,#48050,#48051,#48052,#48053,#48054,
#48055,#48056,#48057,#48058),(#48059,#48060,#48061,#48062,#48063,#48064,
#48065,#48066,#48067,#48068,#48069),(#48070,#48071,#48072,#48073,#48074,
#48075,#48076,#48077,#48078,#48079,#48080),(#48081,#48082,#48083,#48084,
#48085,#48086,#48087,#48088,#48089,#48090,#48091)),.UNSPECIFIED.,.F.,.F.,
 .F.)
B_SPLINE_SURFACE_WITH_KNOTS((4,4),(4,1,1,1,1,1,1,1,4),(0.075363327330941,
0.903974066580243),(-0.009670337409304,0.,0.1430996309434,0.2858291680282,
0.4284783625449,0.5715211775606,0.714546629698,0.8573667380228,0.9759160461734),
 .UNSPECIFIED.)
GEOMETRIC_REPRESENTATION_ITEM()
RATIONAL_B_SPLINE_SURFACE(((1.12354608686857,1.12354608686857,1.12354608686857,
1.12354608686857,1.12354608686857,1.12354608686857,1.12354608686857,1.12354608686857,
1.12354608686857,1.12354608686857,1.12354608686857),(0.962825764515366,
0.962825764515366,0.962825764515366,0.962825764515366,0.962825764515366,
0.962825764515366,0.962825764515366,0.962825764515366,0.962825764515366,
0.962825764515366,0.962825764515366),(0.958915479647154,0.958915479647154,
0.958915479647154,0.958915479647154,0.958915479647154,0.958915479647154,
0.958915479647154,0.958915479647154,0.958915479647154,0.958915479647154,
0.958915479647154),(1.11181523226393,1.11181523226393,1.11181523226393,
1.11181523226393,1.11181523226393,1.11181523226393,1.11181523226393,1.11181523226393,
1.11181523226393,1.11181523226393,1.11181523226393)))
REPRESENTATION_ITEM('')
SURFACE()
);
#229=(
BOUNDED_SURFACE()
B_SPLINE_SURFACE(3,3,((#48208,#48209,#48210,#48211),(#48212,#48213,#48214,
#48215),(#48216,#48217,#48218,#48219),(#48220,#48221,#48222,#48223)),
 .UNSPECIFIED.,.F.,.F.,.F.)
B_SPLINE_SURFACE_WITH_KNOTS((4,4),(4,4),(0.0986320319978618,0.901362552762759),
(-0.975145040400047,-0.0991746183719311),.UNSPECIFIED.)
GEOMETRIC_REPRESENTATION_ITEM()
RATIONAL_B_SPLINE_SURFACE(((1.17563600436588,1.17563600436588,1.17563600436588,
1.17563600436588),(0.941456244993756,0.941456244993756,0.941456244993756,
0.941456244993756),(0.941454665222131,0.941454665222131,0.941454665222131,
0.941454665222131),(1.175631265051,1.175631265051,1.175631265051,1.175631265051)))
REPRESENTATION_ITEM('')
SURFACE()
);
#230=(
BOUNDED_SURFACE()
B_SPLINE_SURFACE(3,3,((#48242,#48243,#48244,#48245,#48246,#48247,#48248,
#48249,#48250,#48251,#48252,#48253,#48254,#48255,#48256,#48257,#48258,#48259,
#48260,#48261,#48262,#48263,#48264,#48265,#48266,#48267,#48268,#48269,#48270,
#48271,#48272,#48273,#48274),(#48275,#48276,#48277,#48278,#48279,#48280,
#48281,#48282,#48283,#48284,#48285,#48286,#48287,#48288,#48289,#48290,#48291,
#48292,#48293,#48294,#48295,#48296,#48297,#48298,#48299,#48300,#48301,#48302,
#48303,#48304,#48305,#48306,#48307),(#48308,#48309,#48310,#48311,#48312,
#48313,#48314,#48315,#48316,#48317,#48318,#48319,#48320,#48321,#48322,#48323,
#48324,#48325,#48326,#48327,#48328,#48329,#48330,#48331,#48332,#48333,#48334,
#48335,#48336,#48337,#48338,#48339,#48340),(#48341,#48342,#48343,#48344,
#48345,#48346,#48347,#48348,#48349,#48350,#48351,#48352,#48353,#48354,#48355,
#48356,#48357,#48358,#48359,#48360,#48361,#48362,#48363,#48364,#48365,#48366,
#48367,#48368,#48369,#48370,#48371,#48372,#48373)),.UNSPECIFIED.,.F.,.F.,
 .F.)
B_SPLINE_SURFACE_WITH_KNOTS((4,4),(4,1,1,1,1,1,1,1,1,1,1,1,1,1,1,1,1,1,
1,1,1,1,1,1,1,1,1,1,1,1,4),(0.108373753360322,0.903586374444769),(-0.00973690174573,
0.,0.02218452663189,0.04657021466942,0.07320284553102,0.1023250304429,0.1343072162648,
0.1695983198482,0.2086109020835,0.2515270680609,0.2985674986552,0.3503233532582,
0.4076602728557,0.4682065066511,0.528219985243,0.5849729736978,0.6367746699729,
0.6825341132663,0.7235067267525,0.7605074035617,0.7940298126239,0.8241792004265,
0.851066626301,0.8750226986103,0.896463827273,0.9157957933363,0.9333740656998,
0.949358143999,0.9638586260694,0.9770542715531,0.9857155005292),
 .UNSPECIFIED.)
GEOMETRIC_REPRESENTATION_ITEM()
RATIONAL_B_SPLINE_SURFACE(((1.07414686918065,1.07414686918065,1.07414686918065,
1.07414686918065,1.07414686918065,1.07414686918065,1.07414686918065,1.07414686918065,
1.07414686918065,1.07414686918065,1.07414686918065,1.07414686918065,1.07414686918065,
1.07414686918065,1.07414686918065,1.07414686918065,1.07414686918065,1.07414686918065,
1.07414686918065,1.07414686918065,1.07414686918065,1.07414686918065,1.07414686918065,
1.07414686918065,1.07414686918065,1.07414686918065,1.07414686918065,1.07414686918065,
1.07414686918065,1.07414686918065,1.07414686918065,1.07414686918065,1.07414686918065),
(0.973774764072452,0.973774764072452,0.973774764072452,0.973774764072452,
0.973774764072452,0.973774764072452,0.973774764072452,0.973774764072452,
0.973774764072452,0.973774764072452,0.973774764072452,0.973774764072452,
0.973774764072452,0.973774764072452,0.973774764072452,0.973774764072452,
0.973774764072452,0.973774764072452,0.973774764072452,0.973774764072452,
0.973774764072452,0.973774764072452,0.973774764072452,0.973774764072452,
0.973774764072452,0.973774764072452,0.973774764072452,0.973774764072452,
0.973774764072452,0.973774764072452,0.973774764072452,0.973774764072452,
0.973774764072452),(0.975307428462876,0.975307428462876,0.975307428462876,
0.975307428462876,0.975307428462876,0.975307428462876,0.975307428462876,
0.975307428462876,0.975307428462876,0.975307428462876,0.975307428462876,
0.975307428462876,0.975307428462876,0.975307428462876,0.975307428462876,
0.975307428462876,0.975307428462876,0.975307428462876,0.975307428462876,
0.975307428462876,0.975307428462876,0.975307428462876,0.975307428462876,
0.975307428462876,0.975307428462876,0.975307428462876,0.975307428462876,
0.975307428462876,0.975307428462876,0.975307428462876,0.975307428462876,
0.975307428462876,0.975307428462876),(1.07874486235192,1.07874486235192,
1.07874486235192,1.07874486235192,1.07874486235192,1.07874486235192,1.07874486235192,
1.07874486235192,1.07874486235192,1.07874486235192,1.07874486235192,1.07874486235192,
1.07874486235192,1.07874486235192,1.07874486235192,1.07874486235192,1.07874486235192,
1.07874486235192,1.07874486235192,1.07874486235192,1.07874486235192,1.07874486235192,
1.07874486235192,1.07874486235192,1.07874486235192,1.07874486235192,1.07874486235192,
1.07874486235192,1.07874486235192,1.07874486235192,1.07874486235192,1.07874486235192,
1.07874486235192)))
REPRESENTATION_ITEM('')
SURFACE()
);
#231=(
BOUNDED_SURFACE()
B_SPLINE_SURFACE(3,3,((#48758,#48759,#48760,#48761,#48762,#48763,#48764,
#48765,#48766,#48767,#48768,#48769,#48770),(#48771,#48772,#48773,#48774,
#48775,#48776,#48777,#48778,#48779,#48780,#48781,#48782,#48783),(#48784,
#48785,#48786,#48787,#48788,#48789,#48790,#48791,#48792,#48793,#48794,#48795,
#48796),(#48797,#48798,#48799,#48800,#48801,#48802,#48803,#48804,#48805,
#48806,#48807,#48808,#48809)),.UNSPECIFIED.,.F.,.F.,.F.)
B_SPLINE_SURFACE_WITH_KNOTS((4,4),(4,1,1,1,1,1,1,1,1,1,4),(0.0574231646653068,
0.945306788892276),(0.1309905936005,0.1664977910666,0.2356164564824,0.3128428890291,
0.4007505433904,0.5000361747357,0.5993121726045,0.6872040763411,0.7644181606731,
0.8335262268397,0.8690088218608),.UNSPECIFIED.)
GEOMETRIC_REPRESENTATION_ITEM()
RATIONAL_B_SPLINE_SURFACE(((1.19350274020032,1.19350274020032,1.19350274020032,
1.19350274020032,1.19350274020032,1.19350274020032,1.19350274020032,1.19350274020032,
1.19350274020032,1.19350274020032,1.19350274020032,1.19350274020032,1.19350274020032),
(0.934703362630941,0.934703362630941,0.934703362630941,0.934703362630941,
0.934703362630941,0.934703362630941,0.934703362630941,0.934703362630941,
0.934703362630941,0.934703362630941,0.934703362630941,0.934703362630941,
0.934703362630941),(0.935501540738208,0.935501540738208,0.935501540738208,
0.935501540738208,0.935501540738208,0.935501540738208,0.935501540738208,
0.935501540738208,0.935501540738208,0.935501540738208,0.935501540738208,
0.935501540738208,0.935501540738208),(1.19589727452213,1.19589727452213,
1.19589727452213,1.19589727452213,1.19589727452213,1.19589727452213,1.19589727452213,
1.19589727452213,1.19589727452213,1.19589727452213,1.19589727452213,1.19589727452213,
1.19589727452213)))
REPRESENTATION_ITEM('')
SURFACE()
);
#232=(
BOUNDED_SURFACE()
B_SPLINE_SURFACE(3,3,((#48921,#48922,#48923,#48924,#48925,#48926,#48927,
#48928,#48929),(#48930,#48931,#48932,#48933,#48934,#48935,#48936,#48937,
#48938),(#48939,#48940,#48941,#48942,#48943,#48944,#48945,#48946,#48947),
(#48948,#48949,#48950,#48951,#48952,#48953,#48954,#48955,#48956)),
 .UNSPECIFIED.,.F.,.F.,.F.)
B_SPLINE_SURFACE_WITH_KNOTS((4,4),(4,1,1,1,1,1,4),(0.0546972932257005,0.945304219631693),
(0.286889171703242,0.3000858921602,0.4481462942066,0.5934294748234,0.7350160218511,
0.8711055251025,0.961148082229091),.UNSPECIFIED.)
GEOMETRIC_REPRESENTATION_ITEM()
RATIONAL_B_SPLINE_SURFACE(((1.19590004288633,1.19590004288633,1.19590004288633,
1.19590004288633,1.19590004288633,1.19590004288633,1.19590004288633,1.19590004288633,
1.19590004288633),(0.934699542008166,0.934699542008166,0.934699542008166,
0.934699542008166,0.934699542008166,0.934699542008166,0.934699542008166,
0.934699542008166,0.934699542008166),(0.934699985705345,0.934699985705345,
0.934699985705345,0.934699985705345,0.934699985705345,0.934699985705345,
0.934699985705345,0.934699985705345,0.934699985705345),(1.19590137397786,
1.19590137397786,1.19590137397786,1.19590137397786,1.19590137397786,1.19590137397786,
1.19590137397786,1.19590137397786,1.19590137397786)))
REPRESENTATION_ITEM('')
SURFACE()
);
#233=(
BOUNDED_SURFACE()
B_SPLINE_SURFACE(3,3,((#49070,#49071,#49072,#49073,#49074,#49075,#49076,
#49077,#49078,#49079),(#49080,#49081,#49082,#49083,#49084,#49085,#49086,
#49087,#49088,#49089),(#49090,#49091,#49092,#49093,#49094,#49095,#49096,
#49097,#49098,#49099),(#49100,#49101,#49102,#49103,#49104,#49105,#49106,
#49107,#49108,#49109)),.UNSPECIFIED.,.F.,.F.,.F.)
B_SPLINE_SURFACE_WITH_KNOTS((4,4),(4,1,1,1,1,1,1,4),(0.0902165725701947,
0.904252559393621),(0.0113422875341,0.1428793759885,0.285811601384,0.4286834096628,
0.5714931672581,0.7143130821911,0.8572933140146,0.9764111906785),
 .UNSPECIFIED.)
GEOMETRIC_REPRESENTATION_ITEM()
RATIONAL_B_SPLINE_SURFACE(((1.11547932157709,1.11547932157709,1.11547932157709,
1.11547932157709,1.11547932157709,1.11547932157709,1.11547932157709,1.11547932157709,
1.11547932157709,1.11547932157709),(0.962545979710326,0.962545979710326,
0.962545979710326,0.962545979710326,0.962545979710326,0.962545979710326,
0.962545979710326,0.962545979710326,0.962545979710326,0.962545979710326),
(0.961513905112406,0.961513905112406,0.961513905112406,0.961513905112406,
0.961513905112406,0.961513905112406,0.961513905112406,0.961513905112406,
0.961513905112406,0.961513905112406),(1.11238309778333,1.11238309778333,
1.11238309778333,1.11238309778333,1.11238309778333,1.11238309778333,1.11238309778333,
1.11238309778333,1.11238309778333,1.11238309778333)))
REPRESENTATION_ITEM('')
SURFACE()
);
#234=(
BOUNDED_SURFACE()
B_SPLINE_SURFACE(3,3,((#49136,#49137,#49138,#49139,#49140,#49141,#49142,
#49143,#49144),(#49145,#49146,#49147,#49148,#49149,#49150,#49151,#49152,
#49153),(#49154,#49155,#49156,#49157,#49158,#49159,#49160,#49161,#49162),
(#49163,#49164,#49165,#49166,#49167,#49168,#49169,#49170,#49171)),
 .UNSPECIFIED.,.F.,.F.,.F.)
B_SPLINE_SURFACE_WITH_KNOTS((4,4),(4,1,1,1,1,1,4),(0.0547421202676084,0.945259392236121),
(0.038975628375885,0.1288834130457,0.26496497341,0.4065466125696,0.5518231987718,
0.6998761197252,0.71318036205432),.UNSPECIFIED.)
GEOMETRIC_REPRESENTATION_ITEM()
RATIONAL_B_SPLINE_SURFACE(((1.19586062030508,1.19586062030508,1.19586062030508,
1.19586062030508,1.19586062030508,1.19586062030508,1.19586062030508,1.19586062030508,
1.19586062030508),(0.934712683016858,0.934712683016858,0.934712683016858,
0.934712683016858,0.934712683016858,0.934712683016858,0.934712683016858,
0.934712683016858,0.934712683016858),(0.934713126565695,0.934713126565695,
0.934713126565695,0.934713126565695,0.934713126565695,0.934713126565695,
0.934713126565695,0.934713126565695,0.934713126565695),(1.19586195095159,
1.19586195095159,1.19586195095159,1.19586195095159,1.19586195095159,1.19586195095159,
1.19586195095159,1.19586195095159,1.19586195095159)))
REPRESENTATION_ITEM('')
SURFACE()
);
#235=(
BOUNDED_SURFACE()
B_SPLINE_SURFACE(3,3,((#49285,#49286,#49287,#49288,#49289,#49290,#49291,
#49292,#49293,#49294),(#49295,#49296,#49297,#49298,#49299,#49300,#49301,
#49302,#49303,#49304),(#49305,#49306,#49307,#49308,#49309,#49310,#49311,
#49312,#49313,#49314),(#49315,#49316,#49317,#49318,#49319,#49320,#49321,
#49322,#49323,#49324)),.UNSPECIFIED.,.F.,.F.,.F.)
B_SPLINE_SURFACE_WITH_KNOTS((4,4),(4,1,1,1,1,1,1,4),(0.0902480906385812,
0.904266113670097),(0.02358777780563,0.1427066860199,0.2856869176887,0.4285068315006,
0.5713165915697,0.7141884014049,0.8571206249672,0.9886565450657),
 .UNSPECIFIED.)
GEOMETRIC_REPRESENTATION_ITEM()
RATIONAL_B_SPLINE_SURFACE(((1.11546155940106,1.11546155940106,1.11546155940106,
1.11546155940106,1.11546155940106,1.11546155940106,1.11546155940106,1.11546155940106,
1.11546155940106,1.11546155940106),(0.962543353412622,0.962543353412622,
0.962543353412622,0.962543353412622,0.962543353412622,0.962543353412622,
0.962543353412622,0.962543353412622,0.962543353412622,0.962543353412622),
(0.961519712013558,0.961519712013558,0.961519712013558,0.961519712013558,
0.961519712013558,0.961519712013558,0.961519712013558,0.961519712013558,
0.961519712013558,0.961519712013558),(1.11239063520387,1.11239063520387,
1.11239063520387,1.11239063520387,1.11239063520387,1.11239063520387,1.11239063520387,
1.11239063520387,1.11239063520387,1.11239063520387)))
REPRESENTATION_ITEM('')
SURFACE()
);
#236=(
BOUNDED_SURFACE()
B_SPLINE_SURFACE(3,3,((#49364,#49365,#49366,#49367,#49368,#49369),(#49370,
#49371,#49372,#49373,#49374,#49375),(#49376,#49377,#49378,#49379,#49380,
#49381),(#49382,#49383,#49384,#49385,#49386,#49387)),.UNSPECIFIED.,.F.,
 .F.,.F.)
B_SPLINE_SURFACE_WITH_KNOTS((4,4),(4,1,1,4),(0.0986342191388939,0.901369960074243),
(0.317543733191689,0.3333147448852,0.6666852551147,0.682456266808865),
 .UNSPECIFIED.)
GEOMETRIC_REPRESENTATION_ITEM()
RATIONAL_B_SPLINE_SURFACE(((1.17563408853197,1.17563408853197,1.17563408853197,
1.17563408853197,1.17563408853197,1.17563408853197),(0.941454084631828,
0.941454084631828,0.941454084631828,0.941454084631828,0.941454084631828,
0.941454084631828),(0.941455303829123,0.941455303829123,0.941455303829123,
0.941455303829123,0.941455303829123,0.941455303829123),(1.17563774612386,
1.17563774612386,1.17563774612386,1.17563774612386,1.17563774612386,1.17563774612386)))
REPRESENTATION_ITEM('')
SURFACE()
);
#237=(
BOUNDED_SURFACE()
B_SPLINE_SURFACE(3,3,((#49627,#49628,#49629,#49630,#49631,#49632,#49633,
#49634,#49635,#49636,#49637,#49638,#49639,#49640,#49641,#49642,#49643,#49644,
#49645,#49646,#49647,#49648,#49649,#49650,#49651,#49652,#49653,#49654,#49655,
#49656,#49657,#49658,#49659,#49660,#49661,#49662,#49663,#49664,#49665,#49666),
(#49667,#49668,#49669,#49670,#49671,#49672,#49673,#49674,#49675,#49676,
#49677,#49678,#49679,#49680,#49681,#49682,#49683,#49684,#49685,#49686,#49687,
#49688,#49689,#49690,#49691,#49692,#49693,#49694,#49695,#49696,#49697,#49698,
#49699,#49700,#49701,#49702,#49703,#49704,#49705,#49706),(#49707,#49708,
#49709,#49710,#49711,#49712,#49713,#49714,#49715,#49716,#49717,#49718,#49719,
#49720,#49721,#49722,#49723,#49724,#49725,#49726,#49727,#49728,#49729,#49730,
#49731,#49732,#49733,#49734,#49735,#49736,#49737,#49738,#49739,#49740,#49741,
#49742,#49743,#49744,#49745,#49746),(#49747,#49748,#49749,#49750,#49751,
#49752,#49753,#49754,#49755,#49756,#49757,#49758,#49759,#49760,#49761,#49762,
#49763,#49764,#49765,#49766,#49767,#49768,#49769,#49770,#49771,#49772,#49773,
#49774,#49775,#49776,#49777,#49778,#49779,#49780,#49781,#49782,#49783,#49784,
#49785,#49786)),.UNSPECIFIED.,.F.,.F.,.F.)
B_SPLINE_SURFACE_WITH_KNOTS((4,4),(4,1,1,1,1,1,1,1,1,1,1,1,1,1,1,1,1,1,
1,1,1,1,1,1,1,1,1,1,1,1,1,1,1,1,1,1,1,4),(0.109557513697332,0.88523983460631),
(-0.009601789277903,0.,0.02232873710628,0.04690611139379,0.07379420329328,
0.1032833799132,0.1358151932356,0.1719129234016,0.2120200511384,0.2562537498977,
0.3048223338256,0.3583884089718,0.4161300533589,0.4734080944977,0.5265789086099,
0.5739168290462,0.615519134979,0.652991960542,0.6871390289507,0.7180225588761,
0.7460350579758,0.7715291821123,0.7947418182217,0.8158398112656,0.8349884136664,
0.8523604287723,0.8681387312846,0.8825028670571,0.8956298657939,0.9076956876584,
0.9188457170059,0.9291453143216,0.9386431055222,0.9473856329388,0.9554251084374,
0.9628149684932,0.9696055559494,0.9720662896547),.UNSPECIFIED.)
GEOMETRIC_REPRESENTATION_ITEM()
RATIONAL_B_SPLINE_SURFACE(((1.0736979416248,1.0736979416248,1.0736979416248,
1.0736979416248,1.0736979416248,1.0736979416248,1.0736979416248,1.0736979416248,
1.0736979416248,1.0736979416248,1.0736979416248,1.0736979416248,1.0736979416248,
1.0736979416248,1.0736979416248,1.0736979416248,1.0736979416248,1.0736979416248,
1.0736979416248,1.0736979416248,1.0736979416248,1.0736979416248,1.0736979416248,
1.0736979416248,1.0736979416248,1.0736979416248,1.0736979416248,1.0736979416248,
1.0736979416248,1.0736979416248,1.0736979416248,1.0736979416248,1.0736979416248,
1.0736979416248,1.0736979416248,1.0736979416248,1.0736979416248,1.0736979416248,
1.0736979416248,1.0736979416248),(0.976088703540388,0.976088703540388,0.976088703540388,
0.976088703540388,0.976088703540388,0.976088703540388,0.976088703540388,
0.976088703540388,0.976088703540388,0.976088703540388,0.976088703540388,
0.976088703540388,0.976088703540388,0.976088703540388,0.976088703540388,
0.976088703540388,0.976088703540388,0.976088703540388,0.976088703540388,
0.976088703540388,0.976088703540388,0.976088703540388,0.976088703540388,
0.976088703540388,0.976088703540388,0.976088703540388,0.976088703540388,
0.976088703540388,0.976088703540388,0.976088703540388,0.976088703540388,
0.976088703540388,0.976088703540388,0.976088703540388,0.976088703540388,
0.976088703540388,0.976088703540388,0.976088703540388,0.976088703540388,
0.976088703540388),(0.975438381295863,0.975438381295863,0.975438381295863,
0.975438381295863,0.975438381295863,0.975438381295863,0.975438381295863,
0.975438381295863,0.975438381295863,0.975438381295863,0.975438381295863,
0.975438381295863,0.975438381295863,0.975438381295863,0.975438381295863,
0.975438381295863,0.975438381295863,0.975438381295863,0.975438381295863,
0.975438381295863,0.975438381295863,0.975438381295863,0.975438381295863,
0.975438381295863,0.975438381295863,0.975438381295863,0.975438381295863,
0.975438381295863,0.975438381295863,0.975438381295863,0.975438381295863,
0.975438381295863,0.975438381295863,0.975438381295863,0.975438381295863,
0.975438381295863,0.975438381295863,0.975438381295863,0.975438381295863,
0.975438381295863),(1.07174697489122,1.07174697489122,1.07174697489122,
1.07174697489122,1.07174697489122,1.07174697489122,1.07174697489122,1.07174697489122,
1.07174697489122,1.07174697489122,1.07174697489122,1.07174697489122,1.07174697489122,
1.07174697489122,1.07174697489122,1.07174697489122,1.07174697489122,1.07174697489122,
1.07174697489122,1.07174697489122,1.07174697489122,1.07174697489122,1.07174697489122,
1.07174697489122,1.07174697489122,1.07174697489122,1.07174697489122,1.07174697489122,
1.07174697489122,1.07174697489122,1.07174697489122,1.07174697489122,1.07174697489122,
1.07174697489122,1.07174697489122,1.07174697489122,1.07174697489122,1.07174697489122,
1.07174697489122,1.07174697489122)))
REPRESENTATION_ITEM('')
SURFACE()
);
#238=(
BOUNDED_SURFACE()
B_SPLINE_SURFACE(3,3,((#49912,#49913,#49914,#49915,#49916,#49917,#49918,
#49919,#49920),(#49921,#49922,#49923,#49924,#49925,#49926,#49927,#49928,
#49929),(#49930,#49931,#49932,#49933,#49934,#49935,#49936,#49937,#49938),
(#49939,#49940,#49941,#49942,#49943,#49944,#49945,#49946,#49947)),
 .UNSPECIFIED.,.F.,.F.,.F.)
B_SPLINE_SURFACE_WITH_KNOTS((4,4),(4,1,1,1,1,1,4),(0.0546349420399352,0.945366895174421),
(0.288003830103446,0.2998193985502,0.4479601517394,0.5933162069375,0.7349712858318,
0.871099664451,0.959211435602542),.UNSPECIFIED.)
GEOMETRIC_REPRESENTATION_ITEM()
RATIONAL_B_SPLINE_SURFACE(((1.19595529172475,1.19595529172475,1.19595529172475,
1.19595529172475,1.19595529172475,1.19595529172475,1.19595529172475,1.19595529172475,
1.19595529172475),(0.93468103052344,0.93468103052344,0.93468103052344,0.93468103052344,
0.93468103052344,0.93468103052344,0.93468103052344,0.93468103052344,0.93468103052344),
(0.934681569426094,0.934681569426094,0.934681569426094,0.934681569426094,
0.934681569426094,0.934681569426094,0.934681569426094,0.934681569426094,
0.934681569426094),(1.19595690843272,1.19595690843272,1.19595690843272,
1.19595690843272,1.19595690843272,1.19595690843272,1.19595690843272,1.19595690843272,
1.19595690843272)))
REPRESENTATION_ITEM('')
SURFACE()
);
#239=(
BOUNDED_SURFACE()
B_SPLINE_SURFACE(3,3,((#50064,#50065,#50066,#50067,#50068,#50069,#50070,
#50071,#50072,#50073),(#50074,#50075,#50076,#50077,#50078,#50079,#50080,
#50081,#50082,#50083),(#50084,#50085,#50086,#50087,#50088,#50089,#50090,
#50091,#50092,#50093),(#50094,#50095,#50096,#50097,#50098,#50099,#50100,
#50101,#50102,#50103)),.UNSPECIFIED.,.F.,.F.,.F.)
B_SPLINE_SURFACE_WITH_KNOTS((4,4),(4,1,1,1,1,1,1,4),(0.0897027042850842,
0.903974528617832),(0.02295305876273,0.1427319133548,0.2857218418975,0.4285793286892,
0.5713517372348,0.7142096687795,0.8572807309771,0.9622634166072),
 .UNSPECIFIED.)
GEOMETRIC_REPRESENTATION_ITEM()
RATIONAL_B_SPLINE_SURFACE(((1.11534309040735,1.11534309040735,1.11534309040735,
1.11534309040735,1.11534309040735,1.11534309040735,1.11534309040735,1.11534309040735,
1.11534309040735,1.11534309040735),(0.962737277287542,0.962737277287542,
0.962737277287542,0.962737277287542,0.962737277287542,0.962737277287542,
0.962737277287542,0.962737277287542,0.962737277287542,0.962737277287542),
(0.961561433546803,0.961561433546803,0.961561433546803,0.961561433546803,
0.961561433546803,0.961561433546803,0.961561433546803,0.961561433546803,
0.961561433546803,0.961561433546803),(1.11181555918513,1.11181555918513,
1.11181555918513,1.11181555918513,1.11181555918513,1.11181555918513,1.11181555918513,
1.11181555918513,1.11181555918513,1.11181555918513)))
REPRESENTATION_ITEM('')
SURFACE()
);
#240=(
BOUNDED_SURFACE()
B_SPLINE_SURFACE(3,3,((#50322,#50323,#50324,#50325,#50326,#50327,#50328,
#50329,#50330,#50331,#50332,#50333,#50334),(#50335,#50336,#50337,#50338,
#50339,#50340,#50341,#50342,#50343,#50344,#50345,#50346,#50347),(#50348,
#50349,#50350,#50351,#50352,#50353,#50354,#50355,#50356,#50357,#50358,#50359,
#50360),(#50361,#50362,#50363,#50364,#50365,#50366,#50367,#50368,#50369,
#50370,#50371,#50372,#50373)),.UNSPECIFIED.,.F.,.F.,.F.)
B_SPLINE_SURFACE_WITH_KNOTS((4,4),(4,1,1,1,1,1,1,1,1,1,4),(0.0573922460373052,
0.945244139733566),(0.1310483619551,0.1664290842009,0.2355281267714,0.3127253439453,
0.4006209236964,0.4999619679894,0.5993131607486,0.6872253246198,0.7644355181441,
0.8335456904892,0.8689506588994),.UNSPECIFIED.)
GEOMETRIC_REPRESENTATION_ITEM()
RATIONAL_B_SPLINE_SURFACE(((1.19353001815818,1.19353001815818,1.19353001815818,
1.19353001815818,1.19353001815818,1.19353001815818,1.19353001815818,1.19353001815818,
1.19353001815818,1.19353001815818,1.19353001815818,1.19353001815818,1.19353001815818),
(0.934721488377597,0.934721488377597,0.934721488377597,0.934721488377597,
0.934721488377597,0.934721488377597,0.934721488377597,0.934721488377597,
0.934721488377597,0.934721488377597,0.934721488377597,0.934721488377597,
0.934721488377597),(0.935492282742568,0.935492282742568,0.935492282742568,
0.935492282742568,0.935492282742568,0.935492282742568,0.935492282742568,
0.935492282742568,0.935492282742568,0.935492282742568,0.935492282742568,
0.935492282742568,0.935492282742568),(1.19584240125309,1.19584240125309,
1.19584240125309,1.19584240125309,1.19584240125309,1.19584240125309,1.19584240125309,
1.19584240125309,1.19584240125309,1.19584240125309,1.19584240125309,1.19584240125309,
1.19584240125309)))
REPRESENTATION_ITEM('')
SURFACE()
);
#241=(
BOUNDED_SURFACE()
B_SPLINE_SURFACE(2,2,((#50483,#50484,#50485),(#50486,#50487,#50488),(#50489,
#50490,#50491)),.UNSPECIFIED.,.F.,.F.,.F.)
B_SPLINE_SURFACE_WITH_KNOTS((3,3),(3,3),(-0.384396778003823,0.384396780054855),
(0.714171252135544,1.38022246560866),.UNSPECIFIED.)
GEOMETRIC_REPRESENTATION_ITEM()
RATIONAL_B_SPLINE_SURFACE(((1.,0.945057588082017,1.),(0.92702480918682,
0.876091830262289,0.92702480918682),(1.,0.945057588082017,1.)))
REPRESENTATION_ITEM('')
SURFACE()
);
#242=(
BOUNDED_SURFACE()
B_SPLINE_SURFACE(2,2,((#50597,#50598,#50599),(#50600,#50601,#50602),(#50603,
#50604,#50605)),.UNSPECIFIED.,.F.,.F.,.F.)
B_SPLINE_SURFACE_WITH_KNOTS((3,3),(3,3),(-0.384396778088211,0.384396780096543),
(1.76137009171851,2.42742001680813),.UNSPECIFIED.)
GEOMETRIC_REPRESENTATION_ITEM()
RATIONAL_B_SPLINE_SURFACE(((1.,0.945057798670611,1.),(0.927024809163182,
0.8760920254608,0.927024809163182),(1.,0.945057798670611,1.)))
REPRESENTATION_ITEM('')
SURFACE()
);
#243=(
BOUNDED_SURFACE()
B_SPLINE_SURFACE(2,2,((#50608,#50609,#50610),(#50611,#50612,#50613),(#50614,
#50615,#50616)),.UNSPECIFIED.,.F.,.F.,.F.)
B_SPLINE_SURFACE_WITH_KNOTS((3,3),(3,3),(-0.384396778254674,0.384396780219765),
(-0.333024963743409,0.33302496374341),.UNSPECIFIED.)
GEOMETRIC_REPRESENTATION_ITEM()
RATIONAL_B_SPLINE_SURFACE(((1.,0.945057798278785,1.),(0.927024809108865,
0.876092025046235,0.927024809108865),(1.,0.945057798278785,1.)))
REPRESENTATION_ITEM('')
SURFACE()
);
#244=(
BOUNDED_SURFACE()
B_SPLINE_SURFACE(2,2,((#50619,#50620,#50621),(#50622,#50623,#50624),(#50625,
#50626,#50627)),.UNSPECIFIED.,.F.,.F.,.F.)
B_SPLINE_SURFACE_WITH_KNOTS((3,3),(3,3),(-0.384396778076674,0.384396780107987),
(-2.42742011306213,-1.76137023584075),.UNSPECIFIED.)
GEOMETRIC_REPRESENTATION_ITEM()
RATIONAL_B_SPLINE_SURFACE(((1.,0.945057806494753,1.),(0.927024809163199,
0.87609203271399,0.927024809163199),(1.,0.945057806494753,1.)))
REPRESENTATION_ITEM('')
SURFACE()
);
#245=(
BOUNDED_SURFACE()
B_SPLINE_SURFACE(2,2,((#50630,#50631,#50632),(#50633,#50634,#50635),(#50636,
#50637,#50638)),.UNSPECIFIED.,.F.,.F.,.F.)
B_SPLINE_SURFACE_WITH_KNOTS((3,3),(3,3),(-0.384396775432716,0.384396776804917),
(-1.38022383251571,-0.714172862049472),.UNSPECIFIED.)
GEOMETRIC_REPRESENTATION_ITEM()
RATIONAL_B_SPLINE_SURFACE(((1.,0.945057627801957,1.),(0.927024810278266,
0.876091868115137,0.927024810278266),(1.,0.945057627801957,1.)))
REPRESENTATION_ITEM('')
SURFACE()
);
#246=(
BOUNDED_SURFACE()
B_SPLINE_SURFACE(2,2,((#50641,#50642,#50643),(#50644,#50645,#50646),(#50647,
#50648,#50649)),.UNSPECIFIED.,.F.,.F.,.F.)
B_SPLINE_SURFACE_WITH_KNOTS((3,3),(3,3),(-0.384396777981939,0.384396780078218),
(-0.333024791636522,0.333024914411102),.UNSPECIFIED.)
GEOMETRIC_REPRESENTATION_ITEM()
RATIONAL_B_SPLINE_SURFACE(((1.,0.945057834473379,1.),(0.927024809186542,
0.876092058672931,0.927024809186542),(1.,0.945057834473379,1.)))
REPRESENTATION_ITEM('')
SURFACE()
);
#247=(
BOUNDED_SURFACE()
B_SPLINE_SURFACE(3,3,((#50680,#50681,#50682,#50683,#50684,#50685),(#50686,
#50687,#50688,#50689,#50690,#50691),(#50692,#50693,#50694,#50695,#50696,
#50697),(#50698,#50699,#50700,#50701,#50702,#50703)),.UNSPECIFIED.,.F.,
 .F.,.F.)
B_SPLINE_SURFACE_WITH_KNOTS((4,4),(4,1,1,4),(0.0986342191388488,0.901369960096482),
(0.317543733191041,0.3333147448853,0.6666852551147,0.682456266810084),
 .UNSPECIFIED.)
GEOMETRIC_REPRESENTATION_ITEM()
RATIONAL_B_SPLINE_SURFACE(((1.17563408853201,1.17563408853201,1.17563408853201,
1.17563408853201,1.17563408853201,1.17563408853201),(0.94145408462534,0.94145408462534,
0.94145408462534,0.94145408462534,0.94145408462534,0.94145408462534),(0.941455303829109,
0.941455303829109,0.941455303829109,0.941455303829109,0.941455303829109,
0.941455303829109),(1.17563774614332,1.17563774614332,1.17563774614332,
1.17563774614332,1.17563774614332,1.17563774614332)))
REPRESENTATION_ITEM('')
SURFACE()
);
#248=(
BOUNDED_SURFACE()
B_SPLINE_SURFACE(3,3,((#50930,#50931,#50932,#50933,#50934,#50935,#50936,
#50937,#50938,#50939,#50940,#50941,#50942,#50943,#50944,#50945,#50946,#50947,
#50948,#50949,#50950,#50951,#50952,#50953,#50954,#50955,#50956,#50957,#50958,
#50959,#50960,#50961,#50962,#50963,#50964,#50965,#50966,#50967,#50968,#50969),
(#50970,#50971,#50972,#50973,#50974,#50975,#50976,#50977,#50978,#50979,
#50980,#50981,#50982,#50983,#50984,#50985,#50986,#50987,#50988,#50989,#50990,
#50991,#50992,#50993,#50994,#50995,#50996,#50997,#50998,#50999,#51000,#51001,
#51002,#51003,#51004,#51005,#51006,#51007,#51008,#51009),(#51010,#51011,
#51012,#51013,#51014,#51015,#51016,#51017,#51018,#51019,#51020,#51021,#51022,
#51023,#51024,#51025,#51026,#51027,#51028,#51029,#51030,#51031,#51032,#51033,
#51034,#51035,#51036,#51037,#51038,#51039,#51040,#51041,#51042,#51043,#51044,
#51045,#51046,#51047,#51048,#51049),(#51050,#51051,#51052,#51053,#51054,
#51055,#51056,#51057,#51058,#51059,#51060,#51061,#51062,#51063,#51064,#51065,
#51066,#51067,#51068,#51069,#51070,#51071,#51072,#51073,#51074,#51075,#51076,
#51077,#51078,#51079,#51080,#51081,#51082,#51083,#51084,#51085,#51086,#51087,
#51088,#51089)),.UNSPECIFIED.,.F.,.F.,.F.)
B_SPLINE_SURFACE_WITH_KNOTS((4,4),(4,1,1,1,1,1,1,1,1,1,1,1,1,1,1,1,1,1,
1,1,1,1,1,1,1,1,1,1,1,1,1,1,1,1,1,1,1,4),(0.109557826006967,0.885251264281302),
(-0.009601789265348,0.,0.02232759876008,0.04690438428648,0.07379256313311,
0.1032821525075,0.1358145488879,0.1719130282207,0.2120212567498,0.2562571680312,
0.304829894919,0.3584023230986,0.416146088449,0.4734208057249,0.5265860543759,
0.5739192804694,0.6155188222685,0.6529897830592,0.6871354795221,0.7180181888986,
0.7460302867701,0.7715243416762,0.7947371788921,0.8158355553727,0.8349846338425,
0.8523571535141,0.8681359777133,0.8825006466294,0.8956281837449,0.9076945427548,
0.9188451048053,0.9291452127891,0.9386434680718,0.9473863882147,0.9554261628483,
0.9628162067304,0.9696068473725,0.972066289545),.UNSPECIFIED.)
GEOMETRIC_REPRESENTATION_ITEM()
RATIONAL_B_SPLINE_SURFACE(((1.07369782373338,1.07369782373338,1.07369782373338,
1.07369782373338,1.07369782373338,1.07369782373338,1.07369782373338,1.07369782373338,
1.07369782373338,1.07369782373338,1.07369782373338,1.07369782373338,1.07369782373338,
1.07369782373338,1.07369782373338,1.07369782373338,1.07369782373338,1.07369782373338,
1.07369782373338,1.07369782373338,1.07369782373338,1.07369782373338,1.07369782373338,
1.07369782373338,1.07369782373338,1.07369782373338,1.07369782373338,1.07369782373338,
1.07369782373338,1.07369782373338,1.07369782373338,1.07369782373338,1.07369782373338,
1.07369782373338,1.07369782373338,1.07369782373338,1.07369782373338,1.07369782373338,
1.07369782373338,1.07369782373338),(0.976087264743372,0.976087264743372,
0.976087264743372,0.976087264743372,0.976087264743372,0.976087264743372,
0.976087264743372,0.976087264743372,0.976087264743372,0.976087264743372,
0.976087264743372,0.976087264743372,0.976087264743372,0.976087264743372,
0.976087264743372,0.976087264743372,0.976087264743372,0.976087264743372,
0.976087264743372,0.976087264743372,0.976087264743372,0.976087264743372,
0.976087264743372,0.976087264743372,0.976087264743372,0.976087264743372,
0.976087264743372,0.976087264743372,0.976087264743372,0.976087264743372,
0.976087264743372,0.976087264743372,0.976087264743372,0.976087264743372,
0.976087264743372,0.976087264743372,0.976087264743372,0.976087264743372,
0.976087264743372,0.976087264743372),(0.975438400926425,0.975438400926425,
0.975438400926425,0.975438400926425,0.975438400926425,0.975438400926425,
0.975438400926425,0.975438400926425,0.975438400926425,0.975438400926425,
0.975438400926425,0.975438400926425,0.975438400926425,0.975438400926425,
0.975438400926425,0.975438400926425,0.975438400926425,0.975438400926425,
0.975438400926425,0.975438400926425,0.975438400926425,0.975438400926425,
0.975438400926425,0.975438400926425,0.975438400926425,0.975438400926425,
0.975438400926425,0.975438400926425,0.975438400926425,0.975438400926425,
0.975438400926425,0.975438400926425,0.975438400926425,0.975438400926425,
0.975438400926425,0.975438400926425,0.975438400926425,0.975438400926425,
0.975438400926425,0.975438400926425),(1.07175123228254,1.07175123228254,
1.07175123228254,1.07175123228254,1.07175123228254,1.07175123228254,1.07175123228254,
1.07175123228254,1.07175123228254,1.07175123228254,1.07175123228254,1.07175123228254,
1.07175123228254,1.07175123228254,1.07175123228254,1.07175123228254,1.07175123228254,
1.07175123228254,1.07175123228254,1.07175123228254,1.07175123228254,1.07175123228254,
1.07175123228254,1.07175123228254,1.07175123228254,1.07175123228254,1.07175123228254,
1.07175123228254,1.07175123228254,1.07175123228254,1.07175123228254,1.07175123228254,
1.07175123228254,1.07175123228254,1.07175123228254,1.07175123228254,1.07175123228254,
1.07175123228254,1.07175123228254,1.07175123228254)))
REPRESENTATION_ITEM('')
SURFACE()
);
#249=(
BOUNDED_SURFACE()
B_SPLINE_SURFACE(3,3,((#51342,#51343,#51344,#51345,#51346,#51347,#51348,
#51349,#51350,#51351,#51352),(#51353,#51354,#51355,#51356,#51357,#51358,
#51359,#51360,#51361,#51362,#51363),(#51364,#51365,#51366,#51367,#51368,
#51369,#51370,#51371,#51372,#51373,#51374),(#51375,#51376,#51377,#51378,
#51379,#51380,#51381,#51382,#51383,#51384,#51385)),.UNSPECIFIED.,.F.,.F.,
 .F.)
B_SPLINE_SURFACE_WITH_KNOTS((4,4),(4,1,1,1,1,1,1,1,4),(0.0572583228212178,
0.942717312100056),(0.294864893273,0.3218289753162,0.3824545414156,0.4420617671716,
0.5001624934407,0.5582690238001,0.6178889113001,0.678495276987,0.7051030418064),
 .UNSPECIFIED.)
GEOMETRIC_REPRESENTATION_ITEM()
RATIONAL_B_SPLINE_SURFACE(((1.19364643609647,1.19364643609647,1.19364643609647,
1.19364643609647,1.19364643609647,1.19364643609647,1.19364643609647,1.19364643609647,
1.19364643609647,1.19364643609647,1.19364643609647),(0.93545829250305,0.93545829250305,
0.93545829250305,0.93545829250305,0.93545829250305,0.93545829250305,0.93545829250305,
0.93545829250305,0.93545829250305,0.93545829250305,0.93545829250305),(0.935451188163467,
0.935451188163467,0.935451188163467,0.935451188163467,0.935451188163467,
0.935451188163467,0.935451188163467,0.935451188163467,0.935451188163467,
0.935451188163467,0.935451188163467),(1.19362512307772,1.19362512307772,
1.19362512307772,1.19362512307772,1.19362512307772,1.19362512307772,1.19362512307772,
1.19362512307772,1.19362512307772,1.19362512307772,1.19362512307772)))
REPRESENTATION_ITEM('')
SURFACE()
);
#250=(
BOUNDED_SURFACE()
B_SPLINE_SURFACE(3,3,((#51387,#51388,#51389,#51390,#51391,#51392,#51393,
#51394,#51395),(#51396,#51397,#51398,#51399,#51400,#51401,#51402,#51403,
#51404),(#51405,#51406,#51407,#51408,#51409,#51410,#51411,#51412,#51413),
(#51414,#51415,#51416,#51417,#51418,#51419,#51420,#51421,#51422)),
 .UNSPECIFIED.,.F.,.F.,.F.)
B_SPLINE_SURFACE_WITH_KNOTS((4,4),(4,1,1,1,1,1,4),(0.0529020528542322,0.947099750452704),
(0.225333279461291,0.239572547302,0.3572550155842,0.4733386917216,0.5865153077446,
0.6955949780245,0.773470390427119),.UNSPECIFIED.)
GEOMETRIC_REPRESENTATION_ITEM()
RATIONAL_B_SPLINE_SURFACE(((1.19748288514912,1.19748288514912,1.19748288514912,
1.19748288514912,1.19748288514912,1.19748288514912,1.19748288514912,1.19748288514912,
1.19748288514912),(0.934171840603826,0.934171840603826,0.934171840603826,
0.934171840603826,0.934171840603826,0.934171840603826,0.934171840603826,
0.934171840603826,0.934171840603826),(0.934172371617932,0.934172371617932,
0.934172371617932,0.934172371617932,0.934172371617932,0.934172371617932,
0.934172371617932,0.934172371617932,0.934172371617932),(1.19748447819143,
1.19748447819143,1.19748447819143,1.19748447819143,1.19748447819143,1.19748447819143,
1.19748447819143,1.19748447819143,1.19748447819143)))
REPRESENTATION_ITEM('')
SURFACE()
);
#251=(
BOUNDED_SURFACE()
B_SPLINE_SURFACE(3,3,((#51525,#51526,#51527,#51528,#51529,#51530,#51531,
#51532,#51533,#51534),(#51535,#51536,#51537,#51538,#51539,#51540,#51541,
#51542,#51543,#51544),(#51545,#51546,#51547,#51548,#51549,#51550,#51551,
#51552,#51553,#51554),(#51555,#51556,#51557,#51558,#51559,#51560,#51561,
#51562,#51563,#51564)),.UNSPECIFIED.,.F.,.F.,.F.)
B_SPLINE_SURFACE_WITH_KNOTS((4,4),(4,1,1,1,1,1,1,4),(0.0889268305855224,
0.904017315502728),(0.02295305876099,0.1427319370604,0.2857219203474,0.4285792797614,
0.5713515650105,0.7142098207389,0.8572808214069,0.9622634165798),
 .UNSPECIFIED.)
GEOMETRIC_REPRESENTATION_ITEM()
RATIONAL_B_SPLINE_SURFACE(((1.11577973130528,1.11577973130528,1.11577973130528,
1.11577973130528,1.11577973130528,1.11577973130528,1.11577973130528,1.11577973130528,
1.11577973130528,1.11577973130528),(0.962731621536822,0.962731621536822,
0.962731621536822,0.962731621536822,0.962731621536822,0.962731621536822,
0.962731621536822,0.962731621536822,0.962731621536822,0.962731621536822),
(0.961418126538433,0.961418126538433,0.961418126538433,0.961418126538433,
0.961418126538433,0.961418126538433,0.961418126538433,0.961418126538433,
0.961418126538433,0.961418126538433),(1.11183924631011,1.11183924631011,
1.11183924631011,1.11183924631011,1.11183924631011,1.11183924631011,1.11183924631011,
1.11183924631011,1.11183924631011,1.11183924631011)))
REPRESENTATION_ITEM('')
SURFACE()
);
#252=(
BOUNDED_SURFACE()
B_SPLINE_SURFACE(2,2,((#54133,#54134,#54135,#54136,#54137,#54138,#54139,
#54140,#54141),(#54142,#54143,#54144,#54145,#54146,#54147,#54148,#54149,
#54150),(#54151,#54152,#54153,#54154,#54155,#54156,#54157,#54158,#54159)),
 .UNSPECIFIED.,.F.,.T.,.F.)
B_SPLINE_SURFACE_WITH_KNOTS((3,3),(3,2,2,2,3),(0.,1.43998883071719),(-3.14159265358979,
-1.5707963267949,0.,1.5707963267949,3.14159265358979),.UNSPECIFIED.)
GEOMETRIC_REPRESENTATION_ITEM()
RATIONAL_B_SPLINE_SURFACE(((1.,0.707106781186548,1.,0.707106781186548,1.,
0.707106781186548,1.,0.707106781186548,1.),(0.751809411556116,0.531609533071198,
0.751809411556116,0.531609533071198,0.751809411556116,0.531609533071198,
0.751809411556116,0.531609533071198,0.751809411556116),(1.,0.707106781186548,
1.,0.707106781186548,1.,0.707106781186548,1.,0.707106781186548,1.)))
REPRESENTATION_ITEM('')
SURFACE()
);
#253=(
BOUNDED_SURFACE()
B_SPLINE_SURFACE(2,2,((#56066,#56067,#56068,#56069,#56070,#56071,#56072,
#56073,#56074),(#56075,#56076,#56077,#56078,#56079,#56080,#56081,#56082,
#56083),(#56084,#56085,#56086,#56087,#56088,#56089,#56090,#56091,#56092)),
 .UNSPECIFIED.,.F.,.T.,.F.)
B_SPLINE_SURFACE_WITH_KNOTS((3,3),(3,2,2,2,3),(-0.371257902576148,0.541962924803503),
(-3.14159265358979,-1.5707963267949,0.,1.5707963267949,3.14159265358979),
 .UNSPECIFIED.)
GEOMETRIC_REPRESENTATION_ITEM()
RATIONAL_B_SPLINE_SURFACE(((1.,0.707106781186548,1.,0.707106781186548,1.,
0.707106781186548,1.,0.707106781186548,1.),(0.897552147568833,0.634665210014471,
0.897552147568833,0.634665210014471,0.897552147568833,0.634665210014471,
0.897552147568833,0.634665210014471,0.897552147568833),(1.,0.707106781186548,
1.,0.707106781186548,1.,0.707106781186548,1.,0.707106781186548,1.)))
REPRESENTATION_ITEM('')
SURFACE()
);
#254=SPHERICAL_SURFACE('',#25482,0.4000000000033);
#255=SPHERICAL_SURFACE('',#25492,0.4);
#256=SPHERICAL_SURFACE('',#25497,0.4000000000033);
#257=SPHERICAL_SURFACE('',#25501,0.4000000000033);
#258=SPHERICAL_SURFACE('',#25506,0.4000000000004);
#259=SPHERICAL_SURFACE('',#25514,0.4);
#260=SPHERICAL_SURFACE('',#25519,0.4000000000033);
#261=SPHERICAL_SURFACE('',#25523,0.4000000000033);
#262=SPHERICAL_SURFACE('',#25528,0.4000000000004);
#263=SPHERICAL_SURFACE('',#25536,0.4);
#264=SPHERICAL_SURFACE('',#25541,0.4000000000033);
#265=SPHERICAL_SURFACE('',#25545,0.4000000000033);
#266=SPHERICAL_SURFACE('',#25550,0.4000000000004);
#267=SPHERICAL_SURFACE('',#25558,0.4);
#268=SPHERICAL_SURFACE('',#25563,0.4000000000033);
#269=SPHERICAL_SURFACE('',#25567,0.4000000000033);
#270=SPHERICAL_SURFACE('',#25572,0.4000000000004);
#271=SPHERICAL_SURFACE('',#25575,0.4000000000003);
#272=SPHERICAL_SURFACE('',#25581,0.4);
#273=SPHERICAL_SURFACE('',#25587,0.4000000000033);
#274=SPHERICAL_SURFACE('',#25595,0.4);
#275=SPHERICAL_SURFACE('',#25600,0.4000000000033);
#276=SPHERICAL_SURFACE('',#25604,0.4000000000033);
#277=SPHERICAL_SURFACE('',#25609,0.4000000000004);
#278=SPHERICAL_SURFACE('',#27116,1.2);
#279=SPHERICAL_SURFACE('',#27135,4.);
#280=ITEM_DEFINED_TRANSFORMATION($,$,#24937,#25054);
#281=ITEM_DEFINED_TRANSFORMATION($,$,#24990,#25055);
#282=ITEM_DEFINED_TRANSFORMATION($,$,#25057,#25272);
#283=ITEM_DEFINED_TRANSFORMATION($,$,#25263,#25273);
#284=ITEM_DEFINED_TRANSFORMATION($,$,#25214,#25274);
#285=ITEM_DEFINED_TRANSFORMATION($,$,#25263,#25275);
#286=ITEM_DEFINED_TRANSFORMATION($,$,#25277,#25370);
#287=ITEM_DEFINED_TRANSFORMATION($,$,#25337,#25371);
#288=ITEM_DEFINED_TRANSFORMATION($,$,#25470,#25975);
#289=ITEM_DEFINED_TRANSFORMATION($,$,#25644,#25976);
#290=ITEM_DEFINED_TRANSFORMATION($,$,#25657,#25977);
#291=ITEM_DEFINED_TRANSFORMATION($,$,#25807,#25978);
#292=ITEM_DEFINED_TRANSFORMATION($,$,#25820,#25979);
#293=ITEM_DEFINED_TRANSFORMATION($,$,#25469,#25980);
#294=ITEM_DEFINED_TRANSFORMATION($,$,#25982,#26041);
#295=ITEM_DEFINED_TRANSFORMATION($,$,#26016,#26042);
#296=ITEM_DEFINED_TRANSFORMATION($,$,#26270,#27179);
#297=ITEM_DEFINED_TRANSFORMATION($,$,#26507,#27180);
#298=ITEM_DEFINED_TRANSFORMATION($,$,#27107,#27181);
#299=ITEM_DEFINED_TRANSFORMATION($,$,#26507,#27182);
#300=ITEM_DEFINED_TRANSFORMATION($,$,#27107,#27183);
#301=ITEM_DEFINED_TRANSFORMATION($,$,#26270,#27184);
#302=ITEM_DEFINED_TRANSFORMATION($,$,#26507,#27185);
#303=ITEM_DEFINED_TRANSFORMATION($,$,#27107,#27186);
#304=ITEM_DEFINED_TRANSFORMATION($,$,#26507,#27187);
#305=ITEM_DEFINED_TRANSFORMATION($,$,#27107,#27188);
#306=ITEM_DEFINED_TRANSFORMATION($,$,#24884,#27414);
#307=ITEM_DEFINED_TRANSFORMATION($,$,#27189,#27415);
#308=ITEM_DEFINED_TRANSFORMATION($,$,#24935,#27416);
#309=ITEM_DEFINED_TRANSFORMATION($,$,#24936,#27417);
#310=ITEM_DEFINED_TRANSFORMATION($,$,#25056,#27418);
#311=ITEM_DEFINED_TRANSFORMATION($,$,#25276,#27419);
#312=ITEM_DEFINED_TRANSFORMATION($,$,#25372,#27420);
#313=ITEM_DEFINED_TRANSFORMATION($,$,#25397,#27421);
#314=ITEM_DEFINED_TRANSFORMATION($,$,#25422,#27422);
#315=ITEM_DEFINED_TRANSFORMATION($,$,#25468,#27423);
#316=ITEM_DEFINED_TRANSFORMATION($,$,#25981,#27424);
#317=ITEM_DEFINED_TRANSFORMATION($,$,#26043,#27425);
#318=ITEM_DEFINED_TRANSFORMATION($,$,#26068,#27426);
#319=ITEM_DEFINED_TRANSFORMATION($,$,#26269,#27427);
#320=ITEM_DEFINED_TRANSFORMATION($,$,#27315,#27428);
#321=ITEM_DEFINED_TRANSFORMATION($,$,#27392,#27429);
#322=ITEM_DEFINED_TRANSFORMATION($,$,#27370,#27430);
#323=ITEM_DEFINED_TRANSFORMATION($,$,#27238,#27431);
#324=ITEM_DEFINED_TRANSFORMATION($,$,#27293,#27432);
#325=ITEM_DEFINED_TRANSFORMATION($,$,#27189,#27433);
#326=ITEM_DEFINED_TRANSFORMATION($,$,#27315,#27434);
#327=ITEM_DEFINED_TRANSFORMATION($,$,#27370,#27435);
#328=ITEM_DEFINED_TRANSFORMATION($,$,#27238,#27436);
#329=ITEM_DEFINED_TRANSFORMATION($,$,#27238,#27437);
#330=ITEM_DEFINED_TRANSFORMATION($,$,#27238,#27438);
#331=ITEM_DEFINED_TRANSFORMATION($,$,#27238,#27439);
#332=ITEM_DEFINED_TRANSFORMATION($,$,#27238,#27440);
#333=ITEM_DEFINED_TRANSFORMATION($,$,#27293,#27441);
#334=ITEM_DEFINED_TRANSFORMATION($,$,#27293,#27442);
#335=ITEM_DEFINED_TRANSFORMATION($,$,#27293,#27443);
#336=ITEM_DEFINED_TRANSFORMATION($,$,#27293,#27444);
#337=ITEM_DEFINED_TRANSFORMATION($,$,#27293,#27445);
#338=ITEM_DEFINED_TRANSFORMATION($,$,#27293,#27446);
#339=ITEM_DEFINED_TRANSFORMATION($,$,#27293,#27447);
#340=ITEM_DEFINED_TRANSFORMATION($,$,#27293,#27448);
#341=ITEM_DEFINED_TRANSFORMATION($,$,#27293,#27449);
#342=ITEM_DEFINED_TRANSFORMATION($,$,#27293,#27450);
#343=ITEM_DEFINED_TRANSFORMATION($,$,#27293,#27451);
#344=ITEM_DEFINED_TRANSFORMATION($,$,#27293,#27452);
#345=ITEM_DEFINED_TRANSFORMATION($,$,#27293,#27453);
#346=ITEM_DEFINED_TRANSFORMATION($,$,#27293,#27454);
#347=ITEM_DEFINED_TRANSFORMATION($,$,#27293,#27455);
#348=ITEM_DEFINED_TRANSFORMATION($,$,#27370,#27456);
#349=ITEM_DEFINED_TRANSFORMATION($,$,#27315,#27457);
#350=ITEM_DEFINED_TRANSFORMATION($,$,#27315,#27458);
#351=ITEM_DEFINED_TRANSFORMATION($,$,#27370,#27459);
#352=ITEM_DEFINED_TRANSFORMATION($,$,#27370,#27460);
#353=ITEM_DEFINED_TRANSFORMATION($,$,#27370,#27461);
#354=ITEM_DEFINED_TRANSFORMATION($,$,#27370,#27462);
#355=ITEM_DEFINED_TRANSFORMATION($,$,#27370,#27463);
#356=ITEM_DEFINED_TRANSFORMATION($,$,#27370,#27464);
#357=ITEM_DEFINED_TRANSFORMATION($,$,#27370,#27465);
#358=ITEM_DEFINED_TRANSFORMATION($,$,#27370,#27466);
#359=ITEM_DEFINED_TRANSFORMATION($,$,#27370,#27467);
#360=ITEM_DEFINED_TRANSFORMATION($,$,#27370,#27468);
#361=ITEM_DEFINED_TRANSFORMATION($,$,#27370,#27469);
#362=ITEM_DEFINED_TRANSFORMATION($,$,#27370,#27470);
#363=ITEM_DEFINED_TRANSFORMATION($,$,#27370,#27471);
#364=ITEM_DEFINED_TRANSFORMATION($,$,#27370,#27472);
#365=ITEM_DEFINED_TRANSFORMATION($,$,#27370,#27473);
#366=ITEM_DEFINED_TRANSFORMATION($,$,#27392,#27474);
#367=ITEM_DEFINED_TRANSFORMATION($,$,#27392,#27475);
#368=ITEM_DEFINED_TRANSFORMATION($,$,#27392,#27476);
#369=(
REPRESENTATION_RELATIONSHIP($,$,#57253,#57252)
REPRESENTATION_RELATIONSHIP_WITH_TRANSFORMATION(#280)
SHAPE_REPRESENTATION_RELATIONSHIP()
);
#370=(
REPRESENTATION_RELATIONSHIP($,$,#57254,#57252)
REPRESENTATION_RELATIONSHIP_WITH_TRANSFORMATION(#281)
SHAPE_REPRESENTATION_RELATIONSHIP()
);
#371=(
REPRESENTATION_RELATIONSHIP($,$,#57256,#57255)
REPRESENTATION_RELATIONSHIP_WITH_TRANSFORMATION(#282)
SHAPE_REPRESENTATION_RELATIONSHIP()
);
#372=(
REPRESENTATION_RELATIONSHIP($,$,#57258,#57255)
REPRESENTATION_RELATIONSHIP_WITH_TRANSFORMATION(#283)
SHAPE_REPRESENTATION_RELATIONSHIP()
);
#373=(
REPRESENTATION_RELATIONSHIP($,$,#57257,#57255)
REPRESENTATION_RELATIONSHIP_WITH_TRANSFORMATION(#284)
SHAPE_REPRESENTATION_RELATIONSHIP()
);
#374=(
REPRESENTATION_RELATIONSHIP($,$,#57258,#57255)
REPRESENTATION_RELATIONSHIP_WITH_TRANSFORMATION(#285)
SHAPE_REPRESENTATION_RELATIONSHIP()
);
#375=(
REPRESENTATION_RELATIONSHIP($,$,#57260,#57259)
REPRESENTATION_RELATIONSHIP_WITH_TRANSFORMATION(#286)
SHAPE_REPRESENTATION_RELATIONSHIP()
);
#376=(
REPRESENTATION_RELATIONSHIP($,$,#57261,#57259)
REPRESENTATION_RELATIONSHIP_WITH_TRANSFORMATION(#287)
SHAPE_REPRESENTATION_RELATIONSHIP()
);
#377=(
REPRESENTATION_RELATIONSHIP($,$,#57267,#57266)
REPRESENTATION_RELATIONSHIP_WITH_TRANSFORMATION(#288)
SHAPE_REPRESENTATION_RELATIONSHIP()
);
#378=(
REPRESENTATION_RELATIONSHIP($,$,#57268,#57266)
REPRESENTATION_RELATIONSHIP_WITH_TRANSFORMATION(#289)
SHAPE_REPRESENTATION_RELATIONSHIP()
);
#379=(
REPRESENTATION_RELATIONSHIP($,$,#57269,#57266)
REPRESENTATION_RELATIONSHIP_WITH_TRANSFORMATION(#290)
SHAPE_REPRESENTATION_RELATIONSHIP()
);
#380=(
REPRESENTATION_RELATIONSHIP($,$,#57270,#57266)
REPRESENTATION_RELATIONSHIP_WITH_TRANSFORMATION(#291)
SHAPE_REPRESENTATION_RELATIONSHIP()
);
#381=(
REPRESENTATION_RELATIONSHIP($,$,#57271,#57266)
REPRESENTATION_RELATIONSHIP_WITH_TRANSFORMATION(#292)
SHAPE_REPRESENTATION_RELATIONSHIP()
);
#382=(
REPRESENTATION_RELATIONSHIP($,$,#57266,#57265)
REPRESENTATION_RELATIONSHIP_WITH_TRANSFORMATION(#293)
SHAPE_REPRESENTATION_RELATIONSHIP()
);
#383=(
REPRESENTATION_RELATIONSHIP($,$,#57273,#57272)
REPRESENTATION_RELATIONSHIP_WITH_TRANSFORMATION(#294)
SHAPE_REPRESENTATION_RELATIONSHIP()
);
#384=(
REPRESENTATION_RELATIONSHIP($,$,#57274,#57272)
REPRESENTATION_RELATIONSHIP_WITH_TRANSFORMATION(#295)
SHAPE_REPRESENTATION_RELATIONSHIP()
);
#385=(
REPRESENTATION_RELATIONSHIP($,$,#57278,#57251)
REPRESENTATION_RELATIONSHIP_WITH_TRANSFORMATION(#296)
SHAPE_REPRESENTATION_RELATIONSHIP()
);
#386=(
REPRESENTATION_RELATIONSHIP($,$,#57279,#57251)
REPRESENTATION_RELATIONSHIP_WITH_TRANSFORMATION(#297)
SHAPE_REPRESENTATION_RELATIONSHIP()
);
#387=(
REPRESENTATION_RELATIONSHIP($,$,#57280,#57251)
REPRESENTATION_RELATIONSHIP_WITH_TRANSFORMATION(#298)
SHAPE_REPRESENTATION_RELATIONSHIP()
);
#388=(
REPRESENTATION_RELATIONSHIP($,$,#57279,#57251)
REPRESENTATION_RELATIONSHIP_WITH_TRANSFORMATION(#299)
SHAPE_REPRESENTATION_RELATIONSHIP()
);
#389=(
REPRESENTATION_RELATIONSHIP($,$,#57280,#57251)
REPRESENTATION_RELATIONSHIP_WITH_TRANSFORMATION(#300)
SHAPE_REPRESENTATION_RELATIONSHIP()
);
#390=(
REPRESENTATION_RELATIONSHIP($,$,#57278,#57277)
REPRESENTATION_RELATIONSHIP_WITH_TRANSFORMATION(#301)
SHAPE_REPRESENTATION_RELATIONSHIP()
);
#391=(
REPRESENTATION_RELATIONSHIP($,$,#57279,#57277)
REPRESENTATION_RELATIONSHIP_WITH_TRANSFORMATION(#302)
SHAPE_REPRESENTATION_RELATIONSHIP()
);
#392=(
REPRESENTATION_RELATIONSHIP($,$,#57280,#57277)
REPRESENTATION_RELATIONSHIP_WITH_TRANSFORMATION(#303)
SHAPE_REPRESENTATION_RELATIONSHIP()
);
#393=(
REPRESENTATION_RELATIONSHIP($,$,#57279,#57277)
REPRESENTATION_RELATIONSHIP_WITH_TRANSFORMATION(#304)
SHAPE_REPRESENTATION_RELATIONSHIP()
);
#394=(
REPRESENTATION_RELATIONSHIP($,$,#57280,#57277)
REPRESENTATION_RELATIONSHIP_WITH_TRANSFORMATION(#305)
SHAPE_REPRESENTATION_RELATIONSHIP()
);
#395=(
REPRESENTATION_RELATIONSHIP($,$,#57250,#57249)
REPRESENTATION_RELATIONSHIP_WITH_TRANSFORMATION(#306)
SHAPE_REPRESENTATION_RELATIONSHIP()
);
#396=(
REPRESENTATION_RELATIONSHIP($,$,#57281,#57249)
REPRESENTATION_RELATIONSHIP_WITH_TRANSFORMATION(#307)
SHAPE_REPRESENTATION_RELATIONSHIP()
);
#397=(
REPRESENTATION_RELATIONSHIP($,$,#57251,#57249)
REPRESENTATION_RELATIONSHIP_WITH_TRANSFORMATION(#308)
SHAPE_REPRESENTATION_RELATIONSHIP()
);
#398=(
REPRESENTATION_RELATIONSHIP($,$,#57252,#57249)
REPRESENTATION_RELATIONSHIP_WITH_TRANSFORMATION(#309)
SHAPE_REPRESENTATION_RELATIONSHIP()
);
#399=(
REPRESENTATION_RELATIONSHIP($,$,#57255,#57249)
REPRESENTATION_RELATIONSHIP_WITH_TRANSFORMATION(#310)
SHAPE_REPRESENTATION_RELATIONSHIP()
);
#400=(
REPRESENTATION_RELATIONSHIP($,$,#57259,#57249)
REPRESENTATION_RELATIONSHIP_WITH_TRANSFORMATION(#311)
SHAPE_REPRESENTATION_RELATIONSHIP()
);
#401=(
REPRESENTATION_RELATIONSHIP($,$,#57262,#57249)
REPRESENTATION_RELATIONSHIP_WITH_TRANSFORMATION(#312)
SHAPE_REPRESENTATION_RELATIONSHIP()
);
#402=(
REPRESENTATION_RELATIONSHIP($,$,#57263,#57249)
REPRESENTATION_RELATIONSHIP_WITH_TRANSFORMATION(#313)
SHAPE_REPRESENTATION_RELATIONSHIP()
);
#403=(
REPRESENTATION_RELATIONSHIP($,$,#57264,#57249)
REPRESENTATION_RELATIONSHIP_WITH_TRANSFORMATION(#314)
SHAPE_REPRESENTATION_RELATIONSHIP()
);
#404=(
REPRESENTATION_RELATIONSHIP($,$,#57265,#57249)
REPRESENTATION_RELATIONSHIP_WITH_TRANSFORMATION(#315)
SHAPE_REPRESENTATION_RELATIONSHIP()
);
#405=(
REPRESENTATION_RELATIONSHIP($,$,#57272,#57249)
REPRESENTATION_RELATIONSHIP_WITH_TRANSFORMATION(#316)
SHAPE_REPRESENTATION_RELATIONSHIP()
);
#406=(
REPRESENTATION_RELATIONSHIP($,$,#57275,#57249)
REPRESENTATION_RELATIONSHIP_WITH_TRANSFORMATION(#317)
SHAPE_REPRESENTATION_RELATIONSHIP()
);
#407=(
REPRESENTATION_RELATIONSHIP($,$,#57276,#57249)
REPRESENTATION_RELATIONSHIP_WITH_TRANSFORMATION(#318)
SHAPE_REPRESENTATION_RELATIONSHIP()
);
#408=(
REPRESENTATION_RELATIONSHIP($,$,#57277,#57249)
REPRESENTATION_RELATIONSHIP_WITH_TRANSFORMATION(#319)
SHAPE_REPRESENTATION_RELATIONSHIP()
);
#409=(
REPRESENTATION_RELATIONSHIP($,$,#57284,#57249)
REPRESENTATION_RELATIONSHIP_WITH_TRANSFORMATION(#320)
SHAPE_REPRESENTATION_RELATIONSHIP()
);
#410=(
REPRESENTATION_RELATIONSHIP($,$,#57286,#57249)
REPRESENTATION_RELATIONSHIP_WITH_TRANSFORMATION(#321)
SHAPE_REPRESENTATION_RELATIONSHIP()
);
#411=(
REPRESENTATION_RELATIONSHIP($,$,#57285,#57249)
REPRESENTATION_RELATIONSHIP_WITH_TRANSFORMATION(#322)
SHAPE_REPRESENTATION_RELATIONSHIP()
);
#412=(
REPRESENTATION_RELATIONSHIP($,$,#57282,#57249)
REPRESENTATION_RELATIONSHIP_WITH_TRANSFORMATION(#323)
SHAPE_REPRESENTATION_RELATIONSHIP()
);
#413=(
REPRESENTATION_RELATIONSHIP($,$,#57283,#57249)
REPRESENTATION_RELATIONSHIP_WITH_TRANSFORMATION(#324)
SHAPE_REPRESENTATION_RELATIONSHIP()
);
#414=(
REPRESENTATION_RELATIONSHIP($,$,#57281,#57249)
REPRESENTATION_RELATIONSHIP_WITH_TRANSFORMATION(#325)
SHAPE_REPRESENTATION_RELATIONSHIP()
);
#415=(
REPRESENTATION_RELATIONSHIP($,$,#57284,#57249)
REPRESENTATION_RELATIONSHIP_WITH_TRANSFORMATION(#326)
SHAPE_REPRESENTATION_RELATIONSHIP()
);
#416=(
REPRESENTATION_RELATIONSHIP($,$,#57285,#57249)
REPRESENTATION_RELATIONSHIP_WITH_TRANSFORMATION(#327)
SHAPE_REPRESENTATION_RELATIONSHIP()
);
#417=(
REPRESENTATION_RELATIONSHIP($,$,#57282,#57249)
REPRESENTATION_RELATIONSHIP_WITH_TRANSFORMATION(#328)
SHAPE_REPRESENTATION_RELATIONSHIP()
);
#418=(
REPRESENTATION_RELATIONSHIP($,$,#57282,#57249)
REPRESENTATION_RELATIONSHIP_WITH_TRANSFORMATION(#329)
SHAPE_REPRESENTATION_RELATIONSHIP()
);
#419=(
REPRESENTATION_RELATIONSHIP($,$,#57282,#57249)
REPRESENTATION_RELATIONSHIP_WITH_TRANSFORMATION(#330)
SHAPE_REPRESENTATION_RELATIONSHIP()
);
#420=(
REPRESENTATION_RELATIONSHIP($,$,#57282,#57249)
REPRESENTATION_RELATIONSHIP_WITH_TRANSFORMATION(#331)
SHAPE_REPRESENTATION_RELATIONSHIP()
);
#421=(
REPRESENTATION_RELATIONSHIP($,$,#57282,#57249)
REPRESENTATION_RELATIONSHIP_WITH_TRANSFORMATION(#332)
SHAPE_REPRESENTATION_RELATIONSHIP()
);
#422=(
REPRESENTATION_RELATIONSHIP($,$,#57283,#57249)
REPRESENTATION_RELATIONSHIP_WITH_TRANSFORMATION(#333)
SHAPE_REPRESENTATION_RELATIONSHIP()
);
#423=(
REPRESENTATION_RELATIONSHIP($,$,#57283,#57249)
REPRESENTATION_RELATIONSHIP_WITH_TRANSFORMATION(#334)
SHAPE_REPRESENTATION_RELATIONSHIP()
);
#424=(
REPRESENTATION_RELATIONSHIP($,$,#57283,#57249)
REPRESENTATION_RELATIONSHIP_WITH_TRANSFORMATION(#335)
SHAPE_REPRESENTATION_RELATIONSHIP()
);
#425=(
REPRESENTATION_RELATIONSHIP($,$,#57283,#57249)
REPRESENTATION_RELATIONSHIP_WITH_TRANSFORMATION(#336)
SHAPE_REPRESENTATION_RELATIONSHIP()
);
#426=(
REPRESENTATION_RELATIONSHIP($,$,#57283,#57249)
REPRESENTATION_RELATIONSHIP_WITH_TRANSFORMATION(#337)
SHAPE_REPRESENTATION_RELATIONSHIP()
);
#427=(
REPRESENTATION_RELATIONSHIP($,$,#57283,#57249)
REPRESENTATION_RELATIONSHIP_WITH_TRANSFORMATION(#338)
SHAPE_REPRESENTATION_RELATIONSHIP()
);
#428=(
REPRESENTATION_RELATIONSHIP($,$,#57283,#57249)
REPRESENTATION_RELATIONSHIP_WITH_TRANSFORMATION(#339)
SHAPE_REPRESENTATION_RELATIONSHIP()
);
#429=(
REPRESENTATION_RELATIONSHIP($,$,#57283,#57249)
REPRESENTATION_RELATIONSHIP_WITH_TRANSFORMATION(#340)
SHAPE_REPRESENTATION_RELATIONSHIP()
);
#430=(
REPRESENTATION_RELATIONSHIP($,$,#57283,#57249)
REPRESENTATION_RELATIONSHIP_WITH_TRANSFORMATION(#341)
SHAPE_REPRESENTATION_RELATIONSHIP()
);
#431=(
REPRESENTATION_RELATIONSHIP($,$,#57283,#57249)
REPRESENTATION_RELATIONSHIP_WITH_TRANSFORMATION(#342)
SHAPE_REPRESENTATION_RELATIONSHIP()
);
#432=(
REPRESENTATION_RELATIONSHIP($,$,#57283,#57249)
REPRESENTATION_RELATIONSHIP_WITH_TRANSFORMATION(#343)
SHAPE_REPRESENTATION_RELATIONSHIP()
);
#433=(
REPRESENTATION_RELATIONSHIP($,$,#57283,#57249)
REPRESENTATION_RELATIONSHIP_WITH_TRANSFORMATION(#344)
SHAPE_REPRESENTATION_RELATIONSHIP()
);
#434=(
REPRESENTATION_RELATIONSHIP($,$,#57283,#57249)
REPRESENTATION_RELATIONSHIP_WITH_TRANSFORMATION(#345)
SHAPE_REPRESENTATION_RELATIONSHIP()
);
#435=(
REPRESENTATION_RELATIONSHIP($,$,#57283,#57249)
REPRESENTATION_RELATIONSHIP_WITH_TRANSFORMATION(#346)
SHAPE_REPRESENTATION_RELATIONSHIP()
);
#436=(
REPRESENTATION_RELATIONSHIP($,$,#57283,#57249)
REPRESENTATION_RELATIONSHIP_WITH_TRANSFORMATION(#347)
SHAPE_REPRESENTATION_RELATIONSHIP()
);
#437=(
REPRESENTATION_RELATIONSHIP($,$,#57285,#57249)
REPRESENTATION_RELATIONSHIP_WITH_TRANSFORMATION(#348)
SHAPE_REPRESENTATION_RELATIONSHIP()
);
#438=(
REPRESENTATION_RELATIONSHIP($,$,#57284,#57249)
REPRESENTATION_RELATIONSHIP_WITH_TRANSFORMATION(#349)
SHAPE_REPRESENTATION_RELATIONSHIP()
);
#439=(
REPRESENTATION_RELATIONSHIP($,$,#57284,#57249)
REPRESENTATION_RELATIONSHIP_WITH_TRANSFORMATION(#350)
SHAPE_REPRESENTATION_RELATIONSHIP()
);
#440=(
REPRESENTATION_RELATIONSHIP($,$,#57285,#57249)
REPRESENTATION_RELATIONSHIP_WITH_TRANSFORMATION(#351)
SHAPE_REPRESENTATION_RELATIONSHIP()
);
#441=(
REPRESENTATION_RELATIONSHIP($,$,#57285,#57249)
REPRESENTATION_RELATIONSHIP_WITH_TRANSFORMATION(#352)
SHAPE_REPRESENTATION_RELATIONSHIP()
);
#442=(
REPRESENTATION_RELATIONSHIP($,$,#57285,#57249)
REPRESENTATION_RELATIONSHIP_WITH_TRANSFORMATION(#353)
SHAPE_REPRESENTATION_RELATIONSHIP()
);
#443=(
REPRESENTATION_RELATIONSHIP($,$,#57285,#57249)
REPRESENTATION_RELATIONSHIP_WITH_TRANSFORMATION(#354)
SHAPE_REPRESENTATION_RELATIONSHIP()
);
#444=(
REPRESENTATION_RELATIONSHIP($,$,#57285,#57249)
REPRESENTATION_RELATIONSHIP_WITH_TRANSFORMATION(#355)
SHAPE_REPRESENTATION_RELATIONSHIP()
);
#445=(
REPRESENTATION_RELATIONSHIP($,$,#57285,#57249)
REPRESENTATION_RELATIONSHIP_WITH_TRANSFORMATION(#356)
SHAPE_REPRESENTATION_RELATIONSHIP()
);
#446=(
REPRESENTATION_RELATIONSHIP($,$,#57285,#57249)
REPRESENTATION_RELATIONSHIP_WITH_TRANSFORMATION(#357)
SHAPE_REPRESENTATION_RELATIONSHIP()
);
#447=(
REPRESENTATION_RELATIONSHIP($,$,#57285,#57249)
REPRESENTATION_RELATIONSHIP_WITH_TRANSFORMATION(#358)
SHAPE_REPRESENTATION_RELATIONSHIP()
);
#448=(
REPRESENTATION_RELATIONSHIP($,$,#57285,#57249)
REPRESENTATION_RELATIONSHIP_WITH_TRANSFORMATION(#359)
SHAPE_REPRESENTATION_RELATIONSHIP()
);
#449=(
REPRESENTATION_RELATIONSHIP($,$,#57285,#57249)
REPRESENTATION_RELATIONSHIP_WITH_TRANSFORMATION(#360)
SHAPE_REPRESENTATION_RELATIONSHIP()
);
#450=(
REPRESENTATION_RELATIONSHIP($,$,#57285,#57249)
REPRESENTATION_RELATIONSHIP_WITH_TRANSFORMATION(#361)
SHAPE_REPRESENTATION_RELATIONSHIP()
);
#451=(
REPRESENTATION_RELATIONSHIP($,$,#57285,#57249)
REPRESENTATION_RELATIONSHIP_WITH_TRANSFORMATION(#362)
SHAPE_REPRESENTATION_RELATIONSHIP()
);
#452=(
REPRESENTATION_RELATIONSHIP($,$,#57285,#57249)
REPRESENTATION_RELATIONSHIP_WITH_TRANSFORMATION(#363)
SHAPE_REPRESENTATION_RELATIONSHIP()
);
#453=(
REPRESENTATION_RELATIONSHIP($,$,#57285,#57249)
REPRESENTATION_RELATIONSHIP_WITH_TRANSFORMATION(#364)
SHAPE_REPRESENTATION_RELATIONSHIP()
);
#454=(
REPRESENTATION_RELATIONSHIP($,$,#57285,#57249)
REPRESENTATION_RELATIONSHIP_WITH_TRANSFORMATION(#365)
SHAPE_REPRESENTATION_RELATIONSHIP()
);
#455=(
REPRESENTATION_RELATIONSHIP($,$,#57286,#57249)
REPRESENTATION_RELATIONSHIP_WITH_TRANSFORMATION(#366)
SHAPE_REPRESENTATION_RELATIONSHIP()
);
#456=(
REPRESENTATION_RELATIONSHIP($,$,#57286,#57249)
REPRESENTATION_RELATIONSHIP_WITH_TRANSFORMATION(#367)
SHAPE_REPRESENTATION_RELATIONSHIP()
);
#457=(
REPRESENTATION_RELATIONSHIP($,$,#57286,#57249)
REPRESENTATION_RELATIONSHIP_WITH_TRANSFORMATION(#368)
SHAPE_REPRESENTATION_RELATIONSHIP()
);
#458=CONTEXT_DEPENDENT_SHAPE_REPRESENTATION(#369,#57128);
#459=CONTEXT_DEPENDENT_SHAPE_REPRESENTATION(#370,#57129);
#460=CONTEXT_DEPENDENT_SHAPE_REPRESENTATION(#371,#57134);
#461=CONTEXT_DEPENDENT_SHAPE_REPRESENTATION(#372,#57135);
#462=CONTEXT_DEPENDENT_SHAPE_REPRESENTATION(#373,#57136);
#463=CONTEXT_DEPENDENT_SHAPE_REPRESENTATION(#374,#57137);
#464=CONTEXT_DEPENDENT_SHAPE_REPRESENTATION(#375,#57141);
#465=CONTEXT_DEPENDENT_SHAPE_REPRESENTATION(#376,#57142);
#466=CONTEXT_DEPENDENT_SHAPE_REPRESENTATION(#377,#57153);
#467=CONTEXT_DEPENDENT_SHAPE_REPRESENTATION(#378,#57154);
#468=CONTEXT_DEPENDENT_SHAPE_REPRESENTATION(#379,#57155);
#469=CONTEXT_DEPENDENT_SHAPE_REPRESENTATION(#380,#57156);
#470=CONTEXT_DEPENDENT_SHAPE_REPRESENTATION(#381,#57157);
#471=CONTEXT_DEPENDENT_SHAPE_REPRESENTATION(#382,#57158);
#472=CONTEXT_DEPENDENT_SHAPE_REPRESENTATION(#383,#57162);
#473=CONTEXT_DEPENDENT_SHAPE_REPRESENTATION(#384,#57163);
#474=CONTEXT_DEPENDENT_SHAPE_REPRESENTATION(#385,#57170);
#475=CONTEXT_DEPENDENT_SHAPE_REPRESENTATION(#386,#57171);
#476=CONTEXT_DEPENDENT_SHAPE_REPRESENTATION(#387,#57172);
#477=CONTEXT_DEPENDENT_SHAPE_REPRESENTATION(#388,#57173);
#478=CONTEXT_DEPENDENT_SHAPE_REPRESENTATION(#389,#57174);
#479=CONTEXT_DEPENDENT_SHAPE_REPRESENTATION(#390,#57175);
#480=CONTEXT_DEPENDENT_SHAPE_REPRESENTATION(#391,#57176);
#481=CONTEXT_DEPENDENT_SHAPE_REPRESENTATION(#392,#57177);
#482=CONTEXT_DEPENDENT_SHAPE_REPRESENTATION(#393,#57178);
#483=CONTEXT_DEPENDENT_SHAPE_REPRESENTATION(#394,#57179);
#484=CONTEXT_DEPENDENT_SHAPE_REPRESENTATION(#395,#57186);
#485=CONTEXT_DEPENDENT_SHAPE_REPRESENTATION(#396,#57187);
#486=CONTEXT_DEPENDENT_SHAPE_REPRESENTATION(#397,#57188);
#487=CONTEXT_DEPENDENT_SHAPE_REPRESENTATION(#398,#57189);
#488=CONTEXT_DEPENDENT_SHAPE_REPRESENTATION(#399,#57190);
#489=CONTEXT_DEPENDENT_SHAPE_REPRESENTATION(#400,#57191);
#490=CONTEXT_DEPENDENT_SHAPE_REPRESENTATION(#401,#57192);
#491=CONTEXT_DEPENDENT_SHAPE_REPRESENTATION(#402,#57193);
#492=CONTEXT_DEPENDENT_SHAPE_REPRESENTATION(#403,#57194);
#493=CONTEXT_DEPENDENT_SHAPE_REPRESENTATION(#404,#57195);
#494=CONTEXT_DEPENDENT_SHAPE_REPRESENTATION(#405,#57196);
#495=CONTEXT_DEPENDENT_SHAPE_REPRESENTATION(#406,#57197);
#496=CONTEXT_DEPENDENT_SHAPE_REPRESENTATION(#407,#57198);
#497=CONTEXT_DEPENDENT_SHAPE_REPRESENTATION(#408,#57199);
#498=CONTEXT_DEPENDENT_SHAPE_REPRESENTATION(#409,#57200);
#499=CONTEXT_DEPENDENT_SHAPE_REPRESENTATION(#410,#57201);
#500=CONTEXT_DEPENDENT_SHAPE_REPRESENTATION(#411,#57202);
#501=CONTEXT_DEPENDENT_SHAPE_REPRESENTATION(#412,#57203);
#502=CONTEXT_DEPENDENT_SHAPE_REPRESENTATION(#413,#57204);
#503=CONTEXT_DEPENDENT_SHAPE_REPRESENTATION(#414,#57205);
#504=CONTEXT_DEPENDENT_SHAPE_REPRESENTATION(#415,#57206);
#505=CONTEXT_DEPENDENT_SHAPE_REPRESENTATION(#416,#57207);
#506=CONTEXT_DEPENDENT_SHAPE_REPRESENTATION(#417,#57208);
#507=CONTEXT_DEPENDENT_SHAPE_REPRESENTATION(#418,#57209);
#508=CONTEXT_DEPENDENT_SHAPE_REPRESENTATION(#419,#57210);
#509=CONTEXT_DEPENDENT_SHAPE_REPRESENTATION(#420,#57211);
#510=CONTEXT_DEPENDENT_SHAPE_REPRESENTATION(#421,#57212);
#511=CONTEXT_DEPENDENT_SHAPE_REPRESENTATION(#422,#57213);
#512=CONTEXT_DEPENDENT_SHAPE_REPRESENTATION(#423,#57214);
#513=CONTEXT_DEPENDENT_SHAPE_REPRESENTATION(#424,#57215);
#514=CONTEXT_DEPENDENT_SHAPE_REPRESENTATION(#425,#57216);
#515=CONTEXT_DEPENDENT_SHAPE_REPRESENTATION(#426,#57217);
#516=CONTEXT_DEPENDENT_SHAPE_REPRESENTATION(#427,#57218);
#517=CONTEXT_DEPENDENT_SHAPE_REPRESENTATION(#428,#57219);
#518=CONTEXT_DEPENDENT_SHAPE_REPRESENTATION(#429,#57220);
#519=CONTEXT_DEPENDENT_SHAPE_REPRESENTATION(#430,#57221);
#520=CONTEXT_DEPENDENT_SHAPE_REPRESENTATION(#431,#57222);
#521=CONTEXT_DEPENDENT_SHAPE_REPRESENTATION(#432,#57223);
#522=CONTEXT_DEPENDENT_SHAPE_REPRESENTATION(#433,#57224);
#523=CONTEXT_DEPENDENT_SHAPE_REPRESENTATION(#434,#57225);
#524=CONTEXT_DEPENDENT_SHAPE_REPRESENTATION(#435,#57226);
#525=CONTEXT_DEPENDENT_SHAPE_REPRESENTATION(#436,#57227);
#526=CONTEXT_DEPENDENT_SHAPE_REPRESENTATION(#437,#57228);
#527=CONTEXT_DEPENDENT_SHAPE_REPRESENTATION(#438,#57229);
#528=CONTEXT_DEPENDENT_SHAPE_REPRESENTATION(#439,#57230);
#529=CONTEXT_DEPENDENT_SHAPE_REPRESENTATION(#440,#57231);
#530=CONTEXT_DEPENDENT_SHAPE_REPRESENTATION(#441,#57232);
#531=CONTEXT_DEPENDENT_SHAPE_REPRESENTATION(#442,#57233);
#532=CONTEXT_DEPENDENT_SHAPE_REPRESENTATION(#443,#57234);
#533=CONTEXT_DEPENDENT_SHAPE_REPRESENTATION(#444,#57235);
#534=CONTEXT_DEPENDENT_SHAPE_REPRESENTATION(#445,#57236);
#535=CONTEXT_DEPENDENT_SHAPE_REPRESENTATION(#446,#57237);
#536=CONTEXT_DEPENDENT_SHAPE_REPRESENTATION(#447,#57238);
#537=CONTEXT_DEPENDENT_SHAPE_REPRESENTATION(#448,#57239);
#538=CONTEXT_DEPENDENT_SHAPE_REPRESENTATION(#449,#57240);
#539=CONTEXT_DEPENDENT_SHAPE_REPRESENTATION(#450,#57241);
#540=CONTEXT_DEPENDENT_SHAPE_REPRESENTATION(#451,#57242);
#541=CONTEXT_DEPENDENT_SHAPE_REPRESENTATION(#452,#57243);
#542=CONTEXT_DEPENDENT_SHAPE_REPRESENTATION(#453,#57244);
#543=CONTEXT_DEPENDENT_SHAPE_REPRESENTATION(#454,#57245);
#544=CONTEXT_DEPENDENT_SHAPE_REPRESENTATION(#455,#57246);
#545=CONTEXT_DEPENDENT_SHAPE_REPRESENTATION(#456,#57247);
#546=CONTEXT_DEPENDENT_SHAPE_REPRESENTATION(#457,#57248);
#547=NEXT_ASSEMBLY_USAGE_OCCURRENCE('Ball Screw Shaft:1',
'Ball Screw Shaft:1','Ball Screw Shaft:1',#57291,#57292,
'Ball Screw Shaft:1');
#548=NEXT_ASSEMBLY_USAGE_OCCURRENCE('Ball Screw Nut:1',
'Ball Screw Nut:1','Ball Screw Nut:1',#57291,#57293,'Ball Screw Nut:1');
#549=NEXT_ASSEMBLY_USAGE_OCCURRENCE('Floating Bearing Housing:1',
'Floating Bearing Housing:1','Floating Bearing Housing:1',#57294,#57295,
'Floating Bearing Housing:1');
#550=NEXT_ASSEMBLY_USAGE_OCCURRENCE('Collar:1','Collar:1','Collar:1',#57294,
#57297,'Collar:1');
#551=NEXT_ASSEMBLY_USAGE_OCCURRENCE('Lock Nut:1','Lock Nut:1',
'Lock Nut:1',#57294,#57296,'Lock Nut:1');
#552=NEXT_ASSEMBLY_USAGE_OCCURRENCE('Collar:2','Collar:2','Collar:2',#57294,
#57297,'Collar:2');
#553=NEXT_ASSEMBLY_USAGE_OCCURRENCE('Fixed Bearing Housing:1',
'Fixed Bearing Housing:1','Fixed Bearing Housing:1',#57298,#57299,
'Fixed Bearing Housing:1');
#554=NEXT_ASSEMBLY_USAGE_OCCURRENCE('Washer:1','Washer:1','Washer:1',#57298,
#57300,'Washer:1');
#555=NEXT_ASSEMBLY_USAGE_OCCURRENCE('Coupling Spider:1',
'Coupling Spider:1','Coupling Spider:1',#57305,#57306,
'Coupling Spider:1');
#556=NEXT_ASSEMBLY_USAGE_OCCURRENCE('Coupling Set Screw 1:1',
'Coupling Set Screw 1:1','Coupling Set Screw 1:1',#57305,#57307,
'Coupling Set Screw 1:1');
#557=NEXT_ASSEMBLY_USAGE_OCCURRENCE('Coupling Hub 1:1',
'Coupling Hub 1:1','Coupling Hub 1:1',#57305,#57308,'Coupling Hub 1:1');
#558=NEXT_ASSEMBLY_USAGE_OCCURRENCE('Coupling Set Screw 2:1',
'Coupling Set Screw 2:1','Coupling Set Screw 2:1',#57305,#57309,
'Coupling Set Screw 2:1');
#559=NEXT_ASSEMBLY_USAGE_OCCURRENCE('Coupling Hub 2:1',
'Coupling Hub 2:1','Coupling Hub 2:1',#57305,#57310,'Coupling Hub 2:1');
#560=NEXT_ASSEMBLY_USAGE_OCCURRENCE('Coupling Components:1',
'Coupling Components:1','Coupling Components:1',#57304,#57305,
'Coupling Components:1');
#561=NEXT_ASSEMBLY_USAGE_OCCURRENCE('Ball Screw Support Bracket:1',
'Ball Screw Support Bracket:1','Ball Screw Support Bracket:1',#57311,#57312,
'Ball Screw Support Bracket:1');
#562=NEXT_ASSEMBLY_USAGE_OCCURRENCE('Ball Screw Support Plate:1',
'Ball Screw Support Plate:1','Ball Screw Support Plate:1',#57311,#57313,
'Ball Screw Support Plate:1');
#563=NEXT_ASSEMBLY_USAGE_OCCURRENCE('Linear Guide Rail:1',
'Linear Guide Rail:1','Linear Guide Rail:1',#57290,#57317,
'Linear Guide Rail:1');
#564=NEXT_ASSEMBLY_USAGE_OCCURRENCE('Linear Guide Slider:1',
'Linear Guide Slider:1','Linear Guide Slider:1',#57290,#57318,
'Linear Guide Slider:1');
#565=NEXT_ASSEMBLY_USAGE_OCCURRENCE('Slider End Cap:1',
'Slider End Cap:1','Slider End Cap:1',#57290,#57319,'Slider End Cap:1');
#566=NEXT_ASSEMBLY_USAGE_OCCURRENCE('Linear Guide Slider:2',
'Linear Guide Slider:2','Linear Guide Slider:2',#57290,#57318,
'Linear Guide Slider:2');
#567=NEXT_ASSEMBLY_USAGE_OCCURRENCE('Slider End Cap:2',
'Slider End Cap:2','Slider End Cap:2',#57290,#57319,'Slider End Cap:2');
#568=NEXT_ASSEMBLY_USAGE_OCCURRENCE('Linear Guide Rail:2',
'Linear Guide Rail:2','Linear Guide Rail:2',#57316,#57317,
'Linear Guide Rail:2');
#569=NEXT_ASSEMBLY_USAGE_OCCURRENCE('Linear Guide Slider:3',
'Linear Guide Slider:3','Linear Guide Slider:3',#57316,#57318,
'Linear Guide Slider:3');
#570=NEXT_ASSEMBLY_USAGE_OCCURRENCE('Slider End Cap:3',
'Slider End Cap:3','Slider End Cap:3',#57316,#57319,'Slider End Cap:3');
#571=NEXT_ASSEMBLY_USAGE_OCCURRENCE('Linear Guide Slider:4',
'Linear Guide Slider:4','Linear Guide Slider:4',#57316,#57318,
'Linear Guide Slider:4');
#572=NEXT_ASSEMBLY_USAGE_OCCURRENCE('Slider End Cap:4',
'Slider End Cap:4','Slider End Cap:4',#57316,#57319,'Slider End Cap:4');
#573=NEXT_ASSEMBLY_USAGE_OCCURRENCE('Main Plate:1','Main Plate:1',
'Main Plate:1',#57288,#57289,'Main Plate:1');
#574=NEXT_ASSEMBLY_USAGE_OCCURRENCE('Linear Guide Spacer:1',
'Linear Guide Spacer:1','Linear Guide Spacer:1',#57288,#57320,
'Linear Guide Spacer:1');
#575=NEXT_ASSEMBLY_USAGE_OCCURRENCE('Linear Guide Assembly 1:1',
'Linear Guide Assembly 1:1','Linear Guide Assembly 1:1',#57288,#57290,
'Linear Guide Assembly 1:1');
#576=NEXT_ASSEMBLY_USAGE_OCCURRENCE('Ball Screw Assembly:1',
'Ball Screw Assembly:1','Ball Screw Assembly:1',#57288,#57291,
'Ball Screw Assembly:1');
#577=NEXT_ASSEMBLY_USAGE_OCCURRENCE(
'Floating Bearing Support Assembly:1',
'Floating Bearing Support Assembly:1',
'Floating Bearing Support Assembly:1',#57288,#57294,
'Floating Bearing Support Assembly:1');
#578=NEXT_ASSEMBLY_USAGE_OCCURRENCE('Fixed Bearing Support Assembly:1',
'Fixed Bearing Support Assembly:1','Fixed Bearing Support Assembly:1',#57288,
#57298,'Fixed Bearing Support Assembly:1');
#579=NEXT_ASSEMBLY_USAGE_OCCURRENCE('Ball Screw Spacer 1:1',
'Ball Screw Spacer 1:1','Ball Screw Spacer 1:1',#57288,#57301,
'Ball Screw Spacer 1:1');
#580=NEXT_ASSEMBLY_USAGE_OCCURRENCE('Ball Screw Spacer 2:1',
'Ball Screw Spacer 2:1','Ball Screw Spacer 2:1',#57288,#57302,
'Ball Screw Spacer 2:1');
#581=NEXT_ASSEMBLY_USAGE_OCCURRENCE('Motor Mount Plate:1',
'Motor Mount Plate:1','Motor Mount Plate:1',#57288,#57303,
'Motor Mount Plate:1');
#582=NEXT_ASSEMBLY_USAGE_OCCURRENCE('Coupling Assembly:1',
'Coupling Assembly:1','Coupling Assembly:1',#57288,#57304,
'Coupling Assembly:1');
#583=NEXT_ASSEMBLY_USAGE_OCCURRENCE('Ball Screw Support Assembly:1',
'Ball Screw Support Assembly:1','Ball Screw Support Assembly:1',#57288,
#57311,'Ball Screw Support Assembly:1');
#584=NEXT_ASSEMBLY_USAGE_OCCURRENCE('Ball Screw Support Spacer:1',
'Ball Screw Support Spacer:1','Ball Screw Support Spacer:1',#57288,#57314,
'Ball Screw Support Spacer:1');
#585=NEXT_ASSEMBLY_USAGE_OCCURRENCE('Motor Mount Bracket:1',
'Motor Mount Bracket:1','Motor Mount Bracket:1',#57288,#57315,
'Motor Mount Bracket:1');
#586=NEXT_ASSEMBLY_USAGE_OCCURRENCE('Linear Guide Assembly 2:1',
'Linear Guide Assembly 2:1','Linear Guide Assembly 2:1',#57288,#57316,
'Linear Guide Assembly 2:1');
#587=NEXT_ASSEMBLY_USAGE_OCCURRENCE('Low Head Cap Screw M8x45:1',
'Low Head Cap Screw M8x45:1','Low Head Cap Screw M8x45:1',#57288,#57323,
'Low Head Cap Screw M8x45:1');
#588=NEXT_ASSEMBLY_USAGE_OCCURRENCE('Socket Head Cap Screw M4x20:1',
'Socket Head Cap Screw M4x20:1','Socket Head Cap Screw M4x20:1',#57288,
#57325,'Socket Head Cap Screw M4x20:1');
#589=NEXT_ASSEMBLY_USAGE_OCCURRENCE('Socket Head Cap Screw M6x20:1',
'Socket Head Cap Screw M6x20:1','Socket Head Cap Screw M6x20:1',#57288,
#57324,'Socket Head Cap Screw M6x20:1');
#590=NEXT_ASSEMBLY_USAGE_OCCURRENCE('Low Head Cap Screw M5x25:1',
'Low Head Cap Screw M5x25:1','Low Head Cap Screw M5x25:1',#57288,#57321,
'Low Head Cap Screw M5x25:1');
#591=NEXT_ASSEMBLY_USAGE_OCCURRENCE('Socket Head Cap Screw M6x25:1',
'Socket Head Cap Screw M6x25:1','Socket Head Cap Screw M6x25:1',#57288,
#57322,'Socket Head Cap Screw M6x25:1');
#592=NEXT_ASSEMBLY_USAGE_OCCURRENCE('Linear Guide Spacer:2',
'Linear Guide Spacer:2','Linear Guide Spacer:2',#57288,#57320,
'Linear Guide Spacer:2');
#593=NEXT_ASSEMBLY_USAGE_OCCURRENCE('Low Head Cap Screw M8x45:2',
'Low Head Cap Screw M8x45:2','Low Head Cap Screw M8x45:2',#57288,#57323,
'Low Head Cap Screw M8x45:2');
#594=NEXT_ASSEMBLY_USAGE_OCCURRENCE('Socket Head Cap Screw M6x20:2',
'Socket Head Cap Screw M6x20:2','Socket Head Cap Screw M6x20:2',#57288,
#57324,'Socket Head Cap Screw M6x20:2');
#595=NEXT_ASSEMBLY_USAGE_OCCURRENCE('Low Head Cap Screw M5x25:2',
'Low Head Cap Screw M5x25:2','Low Head Cap Screw M5x25:2',#57288,#57321,
'Low Head Cap Screw M5x25:2');
#596=NEXT_ASSEMBLY_USAGE_OCCURRENCE('Low Head Cap Screw M5x25:3',
'Low Head Cap Screw M5x25:3','Low Head Cap Screw M5x25:3',#57288,#57321,
'Low Head Cap Screw M5x25:3');
#597=NEXT_ASSEMBLY_USAGE_OCCURRENCE('Low Head Cap Screw M5x25:4',
'Low Head Cap Screw M5x25:4','Low Head Cap Screw M5x25:4',#57288,#57321,
'Low Head Cap Screw M5x25:4');
#598=NEXT_ASSEMBLY_USAGE_OCCURRENCE('Low Head Cap Screw M5x25:5',
'Low Head Cap Screw M5x25:5','Low Head Cap Screw M5x25:5',#57288,#57321,
'Low Head Cap Screw M5x25:5');
#599=NEXT_ASSEMBLY_USAGE_OCCURRENCE('Low Head Cap Screw M5x25:6',
'Low Head Cap Screw M5x25:6','Low Head Cap Screw M5x25:6',#57288,#57321,
'Low Head Cap Screw M5x25:6');
#600=NEXT_ASSEMBLY_USAGE_OCCURRENCE('Socket Head Cap Screw M6x25:2',
'Socket Head Cap Screw M6x25:2','Socket Head Cap Screw M6x25:2',#57288,
#57322,'Socket Head Cap Screw M6x25:2');
#601=NEXT_ASSEMBLY_USAGE_OCCURRENCE('Socket Head Cap Screw M6x25:3',
'Socket Head Cap Screw M6x25:3','Socket Head Cap Screw M6x25:3',#57288,
#57322,'Socket Head Cap Screw M6x25:3');
#602=NEXT_ASSEMBLY_USAGE_OCCURRENCE('Socket Head Cap Screw M6x25:4',
'Socket Head Cap Screw M6x25:4','Socket Head Cap Screw M6x25:4',#57288,
#57322,'Socket Head Cap Screw M6x25:4');
#603=NEXT_ASSEMBLY_USAGE_OCCURRENCE('Socket Head Cap Screw M6x25:5',
'Socket Head Cap Screw M6x25:5','Socket Head Cap Screw M6x25:5',#57288,
#57322,'Socket Head Cap Screw M6x25:5');
#604=NEXT_ASSEMBLY_USAGE_OCCURRENCE('Socket Head Cap Screw M6x25:6',
'Socket Head Cap Screw M6x25:6','Socket Head Cap Screw M6x25:6',#57288,
#57322,'Socket Head Cap Screw M6x25:6');
#605=NEXT_ASSEMBLY_USAGE_OCCURRENCE('Socket Head Cap Screw M6x25:7',
'Socket Head Cap Screw M6x25:7','Socket Head Cap Screw M6x25:7',#57288,
#57322,'Socket Head Cap Screw M6x25:7');
#606=NEXT_ASSEMBLY_USAGE_OCCURRENCE('Socket Head Cap Screw M6x25:8',
'Socket Head Cap Screw M6x25:8','Socket Head Cap Screw M6x25:8',#57288,
#57322,'Socket Head Cap Screw M6x25:8');
#607=NEXT_ASSEMBLY_USAGE_OCCURRENCE('Socket Head Cap Screw M6x25:9',
'Socket Head Cap Screw M6x25:9','Socket Head Cap Screw M6x25:9',#57288,
#57322,'Socket Head Cap Screw M6x25:9');
#608=NEXT_ASSEMBLY_USAGE_OCCURRENCE('Socket Head Cap Screw M6x25:10',
'Socket Head Cap Screw M6x25:10','Socket Head Cap Screw M6x25:10',#57288,
#57322,'Socket Head Cap Screw M6x25:10');
#609=NEXT_ASSEMBLY_USAGE_OCCURRENCE('Socket Head Cap Screw M6x25:11',
'Socket Head Cap Screw M6x25:11','Socket Head Cap Screw M6x25:11',#57288,
#57322,'Socket Head Cap Screw M6x25:11');
#610=NEXT_ASSEMBLY_USAGE_OCCURRENCE('Socket Head Cap Screw M6x25:12',
'Socket Head Cap Screw M6x25:12','Socket Head Cap Screw M6x25:12',#57288,
#57322,'Socket Head Cap Screw M6x25:12');
#611=NEXT_ASSEMBLY_USAGE_OCCURRENCE('Socket Head Cap Screw M6x25:13',
'Socket Head Cap Screw M6x25:13','Socket Head Cap Screw M6x25:13',#57288,
#57322,'Socket Head Cap Screw M6x25:13');
#612=NEXT_ASSEMBLY_USAGE_OCCURRENCE('Socket Head Cap Screw M6x25:14',
'Socket Head Cap Screw M6x25:14','Socket Head Cap Screw M6x25:14',#57288,
#57322,'Socket Head Cap Screw M6x25:14');
#613=NEXT_ASSEMBLY_USAGE_OCCURRENCE('Socket Head Cap Screw M6x25:15',
'Socket Head Cap Screw M6x25:15','Socket Head Cap Screw M6x25:15',#57288,
#57322,'Socket Head Cap Screw M6x25:15');
#614=NEXT_ASSEMBLY_USAGE_OCCURRENCE('Socket Head Cap Screw M6x25:16',
'Socket Head Cap Screw M6x25:16','Socket Head Cap Screw M6x25:16',#57288,
#57322,'Socket Head Cap Screw M6x25:16');
#615=NEXT_ASSEMBLY_USAGE_OCCURRENCE('Socket Head Cap Screw M6x20:3',
'Socket Head Cap Screw M6x20:3','Socket Head Cap Screw M6x20:3',#57288,
#57324,'Socket Head Cap Screw M6x20:3');
#616=NEXT_ASSEMBLY_USAGE_OCCURRENCE('Low Head Cap Screw M8x45:3',
'Low Head Cap Screw M8x45:3','Low Head Cap Screw M8x45:3',#57288,#57323,
'Low Head Cap Screw M8x45:3');
#617=NEXT_ASSEMBLY_USAGE_OCCURRENCE('Low Head Cap Screw M8x45:4',
'Low Head Cap Screw M8x45:4','Low Head Cap Screw M8x45:4',#57288,#57323,
'Low Head Cap Screw M8x45:4');
#618=NEXT_ASSEMBLY_USAGE_OCCURRENCE('Socket Head Cap Screw M6x20:4',
'Socket Head Cap Screw M6x20:4','Socket Head Cap Screw M6x20:4',#57288,
#57324,'Socket Head Cap Screw M6x20:4');
#619=NEXT_ASSEMBLY_USAGE_OCCURRENCE('Socket Head Cap Screw M6x20:5',
'Socket Head Cap Screw M6x20:5','Socket Head Cap Screw M6x20:5',#57288,
#57324,'Socket Head Cap Screw M6x20:5');
#620=NEXT_ASSEMBLY_USAGE_OCCURRENCE('Socket Head Cap Screw M6x20:6',
'Socket Head Cap Screw M6x20:6','Socket Head Cap Screw M6x20:6',#57288,
#57324,'Socket Head Cap Screw M6x20:6');
#621=NEXT_ASSEMBLY_USAGE_OCCURRENCE('Socket Head Cap Screw M6x20:7',
'Socket Head Cap Screw M6x20:7','Socket Head Cap Screw M6x20:7',#57288,
#57324,'Socket Head Cap Screw M6x20:7');
#622=NEXT_ASSEMBLY_USAGE_OCCURRENCE('Socket Head Cap Screw M6x20:8',
'Socket Head Cap Screw M6x20:8','Socket Head Cap Screw M6x20:8',#57288,
#57324,'Socket Head Cap Screw M6x20:8');
#623=NEXT_ASSEMBLY_USAGE_OCCURRENCE('Socket Head Cap Screw M6x20:9',
'Socket Head Cap Screw M6x20:9','Socket Head Cap Screw M6x20:9',#57288,
#57324,'Socket Head Cap Screw M6x20:9');
#624=NEXT_ASSEMBLY_USAGE_OCCURRENCE('Socket Head Cap Screw M6x20:10',
'Socket Head Cap Screw M6x20:10','Socket Head Cap Screw M6x20:10',#57288,
#57324,'Socket Head Cap Screw M6x20:10');
#625=NEXT_ASSEMBLY_USAGE_OCCURRENCE('Socket Head Cap Screw M6x20:11',
'Socket Head Cap Screw M6x20:11','Socket Head Cap Screw M6x20:11',#57288,
#57324,'Socket Head Cap Screw M6x20:11');
#626=NEXT_ASSEMBLY_USAGE_OCCURRENCE('Socket Head Cap Screw M6x20:12',
'Socket Head Cap Screw M6x20:12','Socket Head Cap Screw M6x20:12',#57288,
#57324,'Socket Head Cap Screw M6x20:12');
#627=NEXT_ASSEMBLY_USAGE_OCCURRENCE('Socket Head Cap Screw M6x20:13',
'Socket Head Cap Screw M6x20:13','Socket Head Cap Screw M6x20:13',#57288,
#57324,'Socket Head Cap Screw M6x20:13');
#628=NEXT_ASSEMBLY_USAGE_OCCURRENCE('Socket Head Cap Screw M6x20:14',
'Socket Head Cap Screw M6x20:14','Socket Head Cap Screw M6x20:14',#57288,
#57324,'Socket Head Cap Screw M6x20:14');
#629=NEXT_ASSEMBLY_USAGE_OCCURRENCE('Socket Head Cap Screw M6x20:15',
'Socket Head Cap Screw M6x20:15','Socket Head Cap Screw M6x20:15',#57288,
#57324,'Socket Head Cap Screw M6x20:15');
#630=NEXT_ASSEMBLY_USAGE_OCCURRENCE('Socket Head Cap Screw M6x20:16',
'Socket Head Cap Screw M6x20:16','Socket Head Cap Screw M6x20:16',#57288,
#57324,'Socket Head Cap Screw M6x20:16');
#631=NEXT_ASSEMBLY_USAGE_OCCURRENCE('Socket Head Cap Screw M6x20:17',
'Socket Head Cap Screw M6x20:17','Socket Head Cap Screw M6x20:17',#57288,
#57324,'Socket Head Cap Screw M6x20:17');
#632=NEXT_ASSEMBLY_USAGE_OCCURRENCE('Socket Head Cap Screw M6x20:18',
'Socket Head Cap Screw M6x20:18','Socket Head Cap Screw M6x20:18',#57288,
#57324,'Socket Head Cap Screw M6x20:18');
#633=NEXT_ASSEMBLY_USAGE_OCCURRENCE('Socket Head Cap Screw M4x20:2',
'Socket Head Cap Screw M4x20:2','Socket Head Cap Screw M4x20:2',#57288,
#57325,'Socket Head Cap Screw M4x20:2');
#634=NEXT_ASSEMBLY_USAGE_OCCURRENCE('Socket Head Cap Screw M4x20:3',
'Socket Head Cap Screw M4x20:3','Socket Head Cap Screw M4x20:3',#57288,
#57325,'Socket Head Cap Screw M4x20:3');
#635=NEXT_ASSEMBLY_USAGE_OCCURRENCE('Socket Head Cap Screw M4x20:4',
'Socket Head Cap Screw M4x20:4','Socket Head Cap Screw M4x20:4',#57288,
#57325,'Socket Head Cap Screw M4x20:4');
#636=TOROIDAL_SURFACE('',#24942,5.2000000000001,0.199999999999989);
#637=TOROIDAL_SURFACE('',#24950,6.30000000000001,0.300000000000011);
#638=TOROIDAL_SURFACE('',#24961,5.3,0.3);
#639=TOROIDAL_SURFACE('',#25028,13.5,0.5);
#640=TOROIDAL_SURFACE('',#25034,23.,1.);
#641=TOROIDAL_SURFACE('',#25036,23.,1.);
#642=TOROIDAL_SURFACE('',#25042,23.,1.);
#643=TOROIDAL_SURFACE('',#25044,23.,1.);
#644=TOROIDAL_SURFACE('',#25301,5.3,0.300000000000002);
#645=TOROIDAL_SURFACE('',#25307,5.3,0.300000000000002);
#646=TOROIDAL_SURFACE('',#25316,12.7,0.300000000000001);
#647=TOROIDAL_SURFACE('',#25322,12.7,0.300000000000002);
#648=TOROIDAL_SURFACE('',#27108,4.25,1.21);
#649=B_SPLINE_CURVE_WITH_KNOTS('',3,(#34781,#34782,#34783,#34784,#34785,
#34786,#34787,#34788,#34789,#34790,#34791,#34792,#34793,#34794,#34795,#34796,
#34797,#34798),.UNSPECIFIED.,.F.,.F.,(4,2,2,2,2,2,2,2,4),(0.,0.0568915880983864,
0.113783176196773,0.170657815990574,0.227532455784374,0.284407095578175,
0.341281735371975,0.398173323470362,0.455064911568748),.UNSPECIFIED.);
#650=B_SPLINE_CURVE_WITH_KNOTS('',3,(#34871,#34872,#34873,#34874),
 .UNSPECIFIED.,.F.,.F.,(4,4),(0.00307564709988169,0.0038021193092735),
 .UNSPECIFIED.);
#651=B_SPLINE_CURVE_WITH_KNOTS('',3,(#34877,#34878,#34879,#34880),
 .UNSPECIFIED.,.F.,.F.,(4,4),(0.00334106894839127,0.00406713764756004),
 .UNSPECIFIED.);
#652=B_SPLINE_CURVE_WITH_KNOTS('',3,(#34902,#34903,#34904,#34905,#34906,
#34907,#34908,#34909,#34910,#34911,#34912,#34913,#34914,#34915,#34916,#34917,
#34918,#34919,#34920,#34921,#34922,#34923,#34924,#34925,#34926,#34927,#34928,
#34929,#34930,#34931,#34932,#34933,#34934,#34935),.UNSPECIFIED.,.T.,.F.,
(4,2,2,2,2,2,2,2,2,2,2,2,2,2,2,2,4),(-1.49374524883065,-1.40036599345989,
-1.30698673808914,-1.21364783735606,-1.12030893662298,-1.02697003588991,
-0.933631135156828,-0.840251879786076,-0.746872624415323,-0.65349336904457,
-0.560114113673817,-0.466775212940739,-0.373436312207661,-0.280097411474584,
-0.186758510741506,-0.0933792553707528,0.),.UNSPECIFIED.);
#653=B_SPLINE_CURVE_WITH_KNOTS('',3,(#34938,#34939,#34940,#34941,#34942,
#34943,#34944,#34945,#34946,#34947,#34948,#34949,#34950,#34951,#34952,#34953,
#34954,#34955,#34956,#34957,#34958,#34959,#34960,#34961,#34962,#34963,#34964,
#34965,#34966,#34967,#34968,#34969,#34970,#34971),.UNSPECIFIED.,.T.,.F.,
(4,2,2,2,2,2,2,2,2,2,2,2,2,2,2,2,4),(-1.48285153280719,-1.39017313824889,
-1.2974947436906,-1.204816696648,-1.11213864960539,-1.01946060256279,-0.926782555520185,
-0.83410416096189,-0.741425766403595,-0.6487473718453,-0.556068977287005,
-0.463390930244401,-0.370712883201798,-0.278034836159194,-0.18535678911659,
-0.0926783945582951,0.),.UNSPECIFIED.);
#654=B_SPLINE_CURVE_WITH_KNOTS('',3,(#35059,#35060,#35061,#35062,#35063,
#35064,#35065,#35066,#35067,#35068),.UNSPECIFIED.,.F.,.F.,(4,2,2,2,4),(-0.928911626390741,
-0.898926291162783,-0.857409357377827,-0.796302001537034,-0.707624607638868),
 .UNSPECIFIED.);
#655=B_SPLINE_CURVE_WITH_KNOTS('',3,(#35071,#35072,#35073,#35074,#35075,
#35076,#35077,#35078,#35079,#35080),.UNSPECIFIED.,.F.,.F.,(4,2,2,2,4),(-0.221287018750753,
-0.132609624853036,-0.0715022690125521,-0.0299853352278067,0.),
 .UNSPECIFIED.);
#656=B_SPLINE_CURVE_WITH_KNOTS('',3,(#35083,#35084,#35085,#35086,#35087,
#35088,#35089,#35090,#35091,#35092),.UNSPECIFIED.,.F.,.F.,(4,2,2,2,4),(-0.221287018750753,
-0.132609624853036,-0.0715022690125519,-0.0299853352278066,0.),
 .UNSPECIFIED.);
#657=B_SPLINE_CURVE_WITH_KNOTS('',3,(#35094,#35095,#35096,#35097,#35098,
#35099,#35100,#35101,#35102,#35103),.UNSPECIFIED.,.F.,.F.,(4,2,2,2,4),(-0.928911626390741,
-0.898926291162935,-0.857409357378189,-0.796302001537705,-0.707624607639988),
 .UNSPECIFIED.);
#658=B_SPLINE_CURVE_WITH_KNOTS('',3,(#35119,#35120,#35121,#35122,#35123,
#35124,#35125,#35126,#35127,#35128),.UNSPECIFIED.,.F.,.F.,(4,2,2,2,4),(-0.221287018750753,
-0.132609624853036,-0.071502269012552,-0.0299853352278066,2.77555756156289E-17),
 .UNSPECIFIED.);
#659=B_SPLINE_CURVE_WITH_KNOTS('',3,(#35131,#35132,#35133,#35134,#35135,
#35136,#35137,#35138,#35139,#35140),.UNSPECIFIED.,.F.,.F.,(4,2,2,2,4),(-0.928911626390742,
-0.898926291162935,-0.857409357378189,-0.796302001537705,-0.707624607639988),
 .UNSPECIFIED.);
#660=B_SPLINE_CURVE_WITH_KNOTS('',3,(#35143,#35144,#35145,#35146,#35147,
#35148,#35149,#35150,#35151,#35152),.UNSPECIFIED.,.F.,.F.,(4,2,2,2,4),(-0.928911626390739,
-0.898926291162933,-0.857409357378188,-0.796302001537705,-0.707624607639989),
 .UNSPECIFIED.);
#661=B_SPLINE_CURVE_WITH_KNOTS('',3,(#35154,#35155,#35156,#35157,#35158,
#35159,#35160,#35161,#35162,#35163),.UNSPECIFIED.,.F.,.F.,(4,2,2,2,4),(-0.221287018750753,
-0.132609624853036,-0.0715022690125519,-0.0299853352278065,0.),
 .UNSPECIFIED.);
#662=B_SPLINE_CURVE_WITH_KNOTS('',3,(#35659,#35660,#35661,#35662,#35663,
#35664,#35665,#35666,#35667,#35668,#35669,#35670,#35671,#35672,#35673,#35674,
#35675,#35676,#35677,#35678,#35679,#35680,#35681,#35682,#35683,#35684,#35685,
#35686,#35687,#35688,#35689,#35690,#35691,#35692),.UNSPECIFIED.,.T.,.F.,
(4,2,2,2,2,2,2,2,2,2,2,2,2,2,2,2,4),(-0.983408728494514,-0.921936907009434,
-0.860465085524354,-0.799010815947619,-0.737556546370885,-0.676102276794151,
-0.614648007217417,-0.553176185732337,-0.491704364247257,-0.430232542762177,
-0.368760721277097,-0.307306451700363,-0.245852182123629,-0.184397912546894,
-0.12294364297016,-0.06147182148508,0.),.UNSPECIFIED.);
#663=B_SPLINE_CURVE_WITH_KNOTS('',3,(#35695,#35696,#35697,#35698,#35699,
#35700,#35701,#35702,#35703,#35704,#35705,#35706,#35707,#35708,#35709,#35710,
#35711,#35712,#35713,#35714,#35715,#35716,#35717,#35718,#35719,#35720,#35721,
#35722,#35723,#35724,#35725,#35726,#35727,#35728),.UNSPECIFIED.,.T.,.F.,
(4,2,2,2,2,2,2,2,2,2,2,2,2,2,2,2,4),(-0.978506763751944,-0.917349594723415,
-0.856192425694886,-0.795036249254422,-0.733880072813958,-0.672723896373494,
-0.611567719933029,-0.550410550904501,-0.489253381875972,-0.428096212847443,
-0.366939043818914,-0.30578286737845,-0.244626690937986,-0.183470514497522,
-0.122314338057057,-0.0611571690285287,0.),.UNSPECIFIED.);
#664=B_SPLINE_CURVE_WITH_KNOTS('',3,(#36464,#36465,#36466,#36467,#36468,
#36469,#36470,#36471,#36472,#36473,#36474,#36475,#36476,#36477,#36478,#36479,
#36480,#36481,#36482,#36483,#36484,#36485),.UNSPECIFIED.,.F.,.F.,(4,3,3,
3,3,3,3,4),(0.,0.1428571428571,0.2857142857143,0.4285714285714,0.5714285714286,
0.7142857142857,0.8571428571429,0.999999898934281),.UNSPECIFIED.);
#665=B_SPLINE_CURVE_WITH_KNOTS('',3,(#36487,#36488,#36489,#36490,#36491,
#36492,#36493,#36494,#36495,#36496),.UNSPECIFIED.,.F.,.F.,(4,2,2,2,4),(0.,
0.25,0.5,0.75,0.999999977827856),.UNSPECIFIED.);
#666=B_SPLINE_CURVE_WITH_KNOTS('',3,(#36497,#36498,#36499,#36500,#36501,
#36502,#36503,#36504,#36505,#36506,#36507,#36508,#36509,#36510,#36511,#36512,
#36513,#36514,#36515,#36516,#36517,#36518,#36519,#36520,#36521,#36522,#36523,
#36524,#36525,#36526,#36527,#36528,#36529,#36530,#36531,#36532,#36533,#36534,
#36535,#36536,#36537,#36538,#36539,#36540,#36541,#36542,#36543,#36544,#36545,
#36546,#36547,#36548,#36549,#36550,#36551,#36552,#36553,#36554),
 .UNSPECIFIED.,.F.,.F.,(4,3,3,3,3,3,3,3,3,3,3,3,3,3,3,3,3,3,3,4),(0.,0.105002988004599,
0.155917176333588,0.250000000000014,0.344903197011831,0.374883793981179,
0.375000000000021,0.437500000000025,0.468750000000026,0.484375000000028,
0.49475363720318,0.50000000000003,0.589831227578696,0.605819254748115,0.693556036024795,
0.774340158848298,0.83459764802956,0.912184758108774,0.984866536115133,
1.),.UNSPECIFIED.);
#667=B_SPLINE_CURVE_WITH_KNOTS('',3,(#36594,#36595,#36596,#36597,#36598,
#36599,#36600),.UNSPECIFIED.,.F.,.F.,(4,3,4),(0.,0.5,1.),.UNSPECIFIED.);
#668=B_SPLINE_CURVE_WITH_KNOTS('',3,(#36601,#36602,#36603,#36604,#36605,
#36606,#36607,#36608,#36609,#36610,#36611,#36612,#36613,#36614,#36615,#36616,
#36617,#36618,#36619,#36620,#36621,#36622,#36623,#36624,#36625,#36626,#36627,
#36628,#36629,#36630,#36631,#36632,#36633,#36634,#36635,#36636,#36637,#36638,
#36639,#36640),.UNSPECIFIED.,.F.,.F.,(4,3,3,3,3,3,3,3,3,3,3,3,3,4),(0.,
0.0909082481788675,0.123952457010317,0.249999999999991,0.369498550498918,
0.437499999999988,0.466123466012437,0.495112348455061,0.499999999999986,
0.615780953250484,0.725499099793163,0.834738856311408,0.940690774028189,
0.999999999999981),.UNSPECIFIED.);
#669=B_SPLINE_CURVE_WITH_KNOTS('',3,(#36681,#36682,#36683,#36684,#36685,
#36686,#36687),.UNSPECIFIED.,.F.,.F.,(4,3,4),(0.,0.5,1.),.UNSPECIFIED.);
#670=B_SPLINE_CURVE_WITH_KNOTS('',3,(#36689,#36690,#36691,#36692,#36693,
#36694,#36695,#36696,#36697,#36698,#36699,#36700,#36701,#36702,#36703,#36704,
#36705,#36706,#36707,#36708,#36709,#36710,#36711,#36712,#36713,#36714,#36715,
#36716,#36717,#36718,#36719,#36720,#36721,#36722,#36723,#36724,#36725,#36726,
#36727,#36728),.UNSPECIFIED.,.F.,.F.,(4,3,3,3,3,3,3,3,3,3,3,3,3,4),(0.,
0.0902944655636358,0.118857317207941,0.249999999999996,0.363581344800914,
0.437499999999993,0.46615258320005,0.495170166317412,0.499999999999992,
0.615785321959331,0.718419711826768,0.827854048218974,0.933927706995318,
1.),.UNSPECIFIED.);
#671=B_SPLINE_CURVE_WITH_KNOTS('',3,(#36729,#36730,#36731,#36732,#36733,
#36734,#36735,#36736,#36737,#36738,#36739,#36740,#36741,#36742,#36743,#36744,
#36745,#36746,#36747,#36748,#36749,#36750,#36751,#36752,#36753,#36754,#36755,
#36756,#36757,#36758,#36759,#36760,#36761,#36762,#36763,#36764,#36765,#36766,
#36767,#36768,#36769,#36770,#36771,#36772,#36773,#36774,#36775,#36776,#36777,
#36778,#36779,#36780,#36781,#36782,#36783,#36784,#36785,#36786),
 .UNSPECIFIED.,.F.,.F.,(4,3,3,3,3,3,3,3,3,3,3,3,3,3,3,3,3,3,3,4),(0.,0.105552995127946,
0.150464219760517,0.249999999999963,0.345315720540772,0.371222911163473,
0.374999999999944,0.437499999999933,0.468749999999929,0.484374999999928,
0.494785177746841,0.499999999999927,0.589592294372024,0.602891943836453,
0.690489241102981,0.771089083019577,0.833649950322395,0.911000884560973,
0.983433730186261,1.),.UNSPECIFIED.);
#672=B_SPLINE_CURVE_WITH_KNOTS('',3,(#36832,#36833,#36834,#36835,#36836,
#36837,#36838,#36839,#36840,#36841,#36842,#36843,#36844,#36845,#36846,#36847,
#36848,#36849,#36850,#36851,#36852,#36853,#36854,#36855,#36856,#36857,#36858,
#36859,#36860,#36861,#36862,#36863,#36864,#36865,#36866,#36867,#36868,#36869,
#36870,#36871,#36872,#36873,#36874,#36875,#36876,#36877,#36878,#36879,#36880,
#36881,#36882,#36883,#36884,#36885,#36886,#36887,#36888,#36889,#36890,#36891,
#36892,#36893,#36894,#36895,#36896,#36897,#36898,#36899,#36900,#36901,#36902,
#36903,#36904),.UNSPECIFIED.,.F.,.F.,(4,3,3,3,3,3,3,3,3,3,3,3,3,3,3,3,3,
3,3,3,3,3,3,3,4),(0.,0.0458328892065342,0.0918178601818331,0.137727870818893,
0.1428571428571,0.14853659813261,0.203804992710247,0.259124754660749,0.2857142857143,
0.296137570174206,0.362354499372803,0.4285714285714,0.443717909280085,0.511006798168795,
0.5714285714286,0.591516277431312,0.658633939603418,0.7142857142857,0.739436741598557,
0.798289799370729,0.8571428571429,0.887213042156971,0.933524276500352,0.979590782779799,
1.),.UNSPECIFIED.);
#673=B_SPLINE_CURVE_WITH_KNOTS('',3,(#36907,#36908,#36909,#36910,#36911,
#36912,#36913,#36914,#36915,#36916,#36917,#36918,#36919,#36920,#36921,#36922,
#36923,#36924,#36925,#36926,#36927,#36928,#36929,#36930,#36931,#36932,#36933,
#36934,#36935,#36936,#36937,#36938,#36939,#36940,#36941,#36942,#36943,#36944,
#36945,#36946),.UNSPECIFIED.,.F.,.F.,(4,3,3,3,3,3,3,3,3,3,3,3,3,4),(0.,
0.13299060193257,0.15336958276858,0.288984804521056,0.306719318925449,0.443622689339626,
0.460361902078992,0.597256089920579,0.614811263003171,0.75,0.769627679195988,
0.90936404691236,0.924609578280667,0.999999999980555),.UNSPECIFIED.);
#674=B_SPLINE_CURVE_WITH_KNOTS('',3,(#36969,#36970,#36971,#36972,#36973,
#36974,#36975,#36976,#36977,#36978),.UNSPECIFIED.,.F.,.F.,(4,3,3,4),(0.,
0.3333333333333,0.6666666666667,1.),.UNSPECIFIED.);
#675=B_SPLINE_CURVE_WITH_KNOTS('',3,(#37114,#37115,#37116,#37117,#37118,
#37119,#37120,#37121,#37122,#37123,#37124,#37125,#37126,#37127,#37128,#37129,
#37130,#37131,#37132,#37133,#37134,#37135,#37136,#37137,#37138,#37139,#37140,
#37141,#37142,#37143,#37144,#37145,#37146,#37147,#37148,#37149,#37150,#37151,
#37152,#37153,#37154,#37155,#37156,#37157,#37158,#37159,#37160,#37161,#37162,
#37163,#37164,#37165,#37166,#37167,#37168,#37169,#37170,#37171,#37172,#37173,
#37174,#37175,#37176,#37177,#37178,#37179,#37180,#37181,#37182,#37183,#37184,
#37185,#37186,#37187,#37188,#37189,#37190,#37191,#37192,#37193,#37194,#37195,
#37196,#37197,#37198,#37199,#37200,#37201,#37202),.UNSPECIFIED.,.F.,.F.,
(4,2,2,1,2,2,2,2,1,1,2,2,2,2,1,1,1,2,2,2,2,2,2,2,2,2,1,2,2,2,1,1,2,2,2,
2,1,1,2,2,2,2,1,1,2,2,2,1,1,2,2,4),(0.,0.031249999999999,0.0468749999999985,
0.0546874999999983,0.0585937499999983,0.0624999999999984,0.0937499999999984,
0.109374999999998,0.117187499999999,0.121093749999999,0.123046874999999,
0.124999999999999,0.1875,0.21875,0.234375,0.2421875,0.24609375,0.248046875,
0.25,0.312500000000001,0.343750000000002,0.359375000000002,0.375000000000002,
0.437500000000003,0.468750000000003,0.484375000000004,0.492187500000004,
0.496093750000004,0.500000000000004,0.562500000000005,0.593750000000005,
0.609375000000006,0.617187500000006,0.625000000000006,0.687500000000006,
0.718750000000006,0.734375000000007,0.742187500000007,0.746093750000007,
0.750000000000007,0.812500000000008,0.843750000000008,0.859375000000009,
0.867187500000009,0.871093750000009,0.875000000000009,0.906250000000007,
0.921875000000006,0.929687500000006,0.933593750000006,0.937500000000006,
1.),.UNSPECIFIED.);
#676=B_SPLINE_CURVE_WITH_KNOTS('',3,(#37205,#37206,#37207,#37208,#37209,
#37210,#37211,#37212,#37213,#37214,#37215,#37216,#37217,#37218,#37219,#37220,
#37221,#37222,#37223,#37224,#37225,#37226,#37227,#37228,#37229,#37230,#37231,
#37232,#37233,#37234,#37235,#37236,#37237,#37238,#37239,#37240,#37241,#37242,
#37243,#37244,#37245,#37246,#37247,#37248,#37249,#37250,#37251,#37252,#37253,
#37254,#37255,#37256,#37257,#37258,#37259,#37260,#37261,#37262,#37263,#37264,
#37265,#37266,#37267,#37268,#37269,#37270,#37271,#37272,#37273,#37274,#37275,
#37276,#37277,#37278,#37279,#37280,#37281,#37282,#37283,#37284,#37285,#37286,
#37287,#37288,#37289,#37290,#37291,#37292,#37293,#37294,#37295,#37296,#37297,
#37298,#37299,#37300,#37301,#37302,#37303,#37304,#37305,#37306,#37307,#37308,
#37309,#37310,#37311,#37312,#37313,#37314,#37315,#37316,#37317,#37318,#37319,
#37320,#37321,#37322,#37323,#37324,#37325,#37326,#37327,#37328,#37329,#37330,
#37331,#37332,#37333,#37334,#37335,#37336,#37337,#37338,#37339,#37340,#37341,
#37342,#37343,#37344,#37345,#37346,#37347,#37348,#37349,#37350,#37351,#37352,
#37353,#37354,#37355,#37356,#37357,#37358,#37359,#37360,#37361,#37362,#37363,
#37364,#37365,#37366,#37367,#37368,#37369,#37370,#37371,#37372,#37373,#37374,
#37375,#37376,#37377,#37378,#37379,#37380,#37381,#37382,#37383,#37384,#37385,
#37386,#37387,#37388,#37389,#37390,#37391),.UNSPECIFIED.,.F.,.F.,(4,3,3,
3,3,3,3,3,3,3,3,3,3,3,3,3,3,3,3,3,3,3,3,3,3,3,3,3,3,3,3,3,3,3,3,3,3,3,3,
3,3,3,3,3,3,3,3,3,3,3,3,3,3,3,3,3,3,3,3,3,3,3,4),(7.50077097463719E-8,2.18347029427447E-7,
0.0229487856938132,0.0291139710122845,0.0509738189930032,0.0551840493051654,
0.0624999999999677,0.0795327477259671,0.100117077611303,0.102945273631019,
0.109374999999943,0.11718749999994,0.121093749999938,0.123046874999937,
0.124511718749936,0.124999999999936,0.126823302088405,0.154172312025519,
0.168540298053765,0.195094832668279,0.207814194056933,0.234374999999943,
0.243586029297769,0.245604724495927,0.249999999999944,0.286467474258032,
0.32318429611145,0.33538678826966,0.372228071632762,0.396071565286844,0.433033005791837,
0.468749999999958,0.471330308172129,0.484374999999959,0.49218749999996,
0.499325175973332,0.49999999999996,0.539362014881174,0.553208179067863,
0.592489117635982,0.619376295226936,0.658509964129895,0.6731316840546,0.711996821297296,
0.71672755379256,0.718749999999974,0.734374999999975,0.742187499999975,
0.746093749999976,0.749489018450129,0.749999999999976,0.753696520049675,
0.789783434716073,0.822480899844826,0.851890674726284,0.878120292282693,
0.901491656587809,0.922410562386568,0.941272552181438,0.958424197689089,
0.97402098939019,0.988170714014038,1.),.UNSPECIFIED.);
#677=B_SPLINE_CURVE_WITH_KNOTS('',3,(#37428,#37429,#37430,#37431,#37432,
#37433,#37434,#37435,#37436,#37437),.UNSPECIFIED.,.F.,.F.,(4,2,2,2,4),(2.21660088532052E-8,
0.25,0.5,0.75,1.),.UNSPECIFIED.);
#678=B_SPLINE_CURVE_WITH_KNOTS('',3,(#37438,#37439,#37440,#37441,#37442,
#37443,#37444,#37445,#37446,#37447,#37448,#37449,#37450,#37451,#37452,#37453,
#37454,#37455,#37456,#37457,#37458,#37459,#37460,#37461,#37462,#37463,#37464,
#37465,#37466,#37467,#37468,#37469,#37470,#37471,#37472,#37473,#37474,#37475,
#37476,#37477,#37478,#37479,#37480,#37481,#37482,#37483,#37484,#37485,#37486,
#37487,#37488,#37489,#37490,#37491,#37492,#37493,#37494,#37495,#37496,#37497,
#37498),.UNSPECIFIED.,.F.,.F.,(4,3,3,3,3,3,3,3,3,3,3,3,3,3,3,3,3,3,3,3,
4),(4.17868136098958E-11,0.100717583252596,0.175358791626298,0.238666052088337,
0.25,0.301434359568119,0.35111583137364,0.400012448249277,0.450006224124639,
0.497458126672331,0.5,0.500002161178376,0.547542422094837,0.598156816571128,
0.647554640521333,0.698777320260667,0.75,0.812847074588508,0.88799364390341,
0.987406860642747,0.999999999945156),.UNSPECIFIED.);
#679=B_SPLINE_CURVE_WITH_KNOTS('',3,(#37541,#37542,#37543,#37544,#37545,
#37546,#37547,#37548,#37549,#37550,#37551,#37552,#37553,#37554,#37555,#37556,
#37557,#37558,#37559,#37560,#37561,#37562,#37563,#37564,#37565,#37566,#37567,
#37568,#37569,#37570,#37571,#37572,#37573,#37574,#37575,#37576,#37577,#37578,
#37579,#37580,#37581,#37582,#37583,#37584,#37585,#37586,#37587,#37588,#37589,
#37590,#37591,#37592,#37593,#37594,#37595,#37596,#37597,#37598,#37599,#37600,
#37601,#37602,#37603,#37604,#37605,#37606,#37607,#37608,#37609,#37610,#37611,
#37612,#37613,#37614,#37615,#37616,#37617,#37618,#37619,#37620,#37621,#37622,
#37623,#37624,#37625,#37626,#37627,#37628,#37629,#37630,#37631,#37632,#37633,
#37634,#37635,#37636,#37637),.UNSPECIFIED.,.F.,.F.,(4,3,3,3,3,3,3,3,3,3,
3,3,3,3,3,3,3,3,3,3,3,3,3,3,3,3,3,3,3,3,3,3,4),(0.,0.0611399008016612,0.118912943243393,
0.122279801603322,0.125000000000001,0.18183766361929,0.187500000000002,
0.218750000000002,0.234375000000002,0.242187500000002,0.247821297884802,
0.250000000000002,0.273770686693072,0.341484900394223,0.40789775146333,
0.425473607482879,0.492297059906689,0.500000000000002,0.565514473352424,
0.574275766966002,0.625000000000002,0.687500000000002,0.718750000000001,
0.725971908159189,0.734375000000002,0.742187500000001,0.747865905418132,
0.750000000000001,0.805738424564014,0.862859242738749,0.877451482579203,
0.938725741289602,1.),.UNSPECIFIED.);
#680=B_SPLINE_CURVE_WITH_KNOTS('',3,(#37676,#37677,#37678,#37679,#37680,
#37681,#37682,#37683,#37684,#37685,#37686,#37687,#37688,#37689,#37690,#37691,
#37692,#37693,#37694,#37695,#37696,#37697,#37698,#37699,#37700,#37701,#37702,
#37703,#37704,#37705,#37706,#37707,#37708,#37709,#37710,#37711,#37712,#37713,
#37714,#37715,#37716,#37717,#37718,#37719,#37720,#37721,#37722,#37723,#37724),
 .UNSPECIFIED.,.F.,.F.,(4,3,3,3,3,3,3,3,3,3,3,3,3,3,3,3,4),(0.,0.0770829581399577,
0.115833104604136,0.19702880740101,0.250000000000003,0.333153117311277,
0.356333767066429,0.375000000000002,0.422947860378306,0.471329030291448,
0.500000000000002,0.606855024395177,0.708280894793895,0.713710048790352,
0.815228553321396,0.918005904150946,1.),.UNSPECIFIED.);
#681=B_SPLINE_CURVE_WITH_KNOTS('',3,(#37725,#37726,#37727,#37728,#37729,
#37730,#37731),.UNSPECIFIED.,.F.,.F.,(4,3,4),(0.,0.5,0.999999979800132),
 .UNSPECIFIED.);
#682=B_SPLINE_CURVE_WITH_KNOTS('',3,(#37732,#37733,#37734,#37735,#37736,
#37737,#37738,#37739,#37740,#37741,#37742,#37743,#37744,#37745,#37746,#37747,
#37748,#37749,#37750,#37751,#37752,#37753,#37754,#37755,#37756,#37757,#37758,
#37759,#37760,#37761,#37762,#37763,#37764,#37765,#37766,#37767,#37768,#37769,
#37770,#37771,#37772,#37773,#37774,#37775,#37776,#37777,#37778,#37779,#37780,
#37781,#37782,#37783,#37784,#37785,#37786,#37787,#37788,#37789),
 .UNSPECIFIED.,.F.,.F.,(4,3,3,3,3,3,3,3,3,3,3,3,3,3,3,3,3,3,3,4),(0.,0.0715674218076948,
0.147880597762145,0.168248115152606,0.25000000000001,0.335016575408999,
0.375000000000014,0.399721731097707,0.437500000000018,0.468750000000019,
0.48437500000002,0.49533836253787,0.50000000000002,0.59336847865171,0.631329959825261,
0.726440396785077,0.827653169575289,0.852289991333602,0.957929681900358,
1.),.UNSPECIFIED.);
#683=B_SPLINE_CURVE_WITH_KNOTS('',3,(#37832,#37833,#37834,#37835,#37836,
#37837,#37838,#37839,#37840,#37841,#37842,#37843,#37844,#37845,#37846,#37847,
#37848,#37849,#37850,#37851,#37852,#37853),.UNSPECIFIED.,.F.,.F.,(4,3,3,
3,3,3,3,4),(1.01036473954356E-7,0.1428571428571,0.2857142857143,0.4285714285714,
0.5714285714286,0.7142857142857,0.8571428571429,1.),.UNSPECIFIED.);
#684=B_SPLINE_CURVE_WITH_KNOTS('',3,(#37896,#37897,#37898,#37899,#37900,
#37901,#37902),.UNSPECIFIED.,.F.,.F.,(4,3,4),(2.15057445811703E-8,0.5,1.),
 .UNSPECIFIED.);
#685=B_SPLINE_CURVE_WITH_KNOTS('',3,(#37904,#37905,#37906,#37907,#37908,
#37909,#37910,#37911,#37912,#37913,#37914,#37915,#37916,#37917,#37918,#37919,
#37920,#37921,#37922,#37923,#37924,#37925,#37926,#37927,#37928,#37929,#37930,
#37931,#37932,#37933,#37934,#37935,#37936,#37937,#37938,#37939,#37940,#37941,
#37942,#37943,#37944,#37945,#37946),.UNSPECIFIED.,.F.,.F.,(4,3,3,3,3,3,
3,3,3,3,3,3,3,3,4),(0.,0.0900134680643692,0.1164031392641,0.243030188030943,
0.249999999999983,0.360148491907499,0.437499999999976,0.466161731423018,
0.495188458339603,0.499999999999975,0.615787821036494,0.712805741778485,
0.822400103490752,0.928574215008832,1.),.UNSPECIFIED.);
#686=B_SPLINE_CURVE_WITH_KNOTS('',3,(#37947,#37948,#37949,#37950,#37951,
#37952,#37953,#37954,#37955,#37956,#37957,#37958,#37959,#37960,#37961,#37962,
#37963,#37964,#37965,#37966,#37967,#37968,#37969,#37970,#37971,#37972,#37973,
#37974,#37975,#37976,#37977,#37978,#37979,#37980,#37981,#37982,#37983,#37984,
#37985,#37986,#37987,#37988,#37989,#37990,#37991,#37992,#37993,#37994,#37995,
#37996,#37997,#37998,#37999,#38000,#38001,#38002,#38003,#38004),
 .UNSPECIFIED.,.F.,.F.,(4,3,3,3,3,3,3,3,3,3,3,3,3,3,3,3,3,3,3,4),(0.,0.105620931649772,
0.147712761945928,0.249999999999997,0.345332751509973,0.368665278781871,
0.374999999999996,0.437499999999994,0.468749999999995,0.484374999999994,
0.494735172857366,0.499999999999994,0.589017276416335,0.600284492062021,
0.686110218149057,0.749999999999997,0.831760917477541,0.908457546686943,
0.980209191163759,1.),.UNSPECIFIED.);
#687=B_SPLINE_CURVE_WITH_KNOTS('',3,(#38046,#38047,#38048,#38049,#38050,
#38051,#38052,#38053,#38054,#38055,#38056,#38057,#38058,#38059,#38060,#38061,
#38062,#38063,#38064,#38065,#38066,#38067),.UNSPECIFIED.,.F.,.F.,(4,3,3,
3,3,3,3,4),(0.,0.1428571428571,0.2857142857143,0.4285714285714,0.5714285714286,
0.7142857142857,0.8571428571429,0.99999989893635),.UNSPECIFIED.);
#688=B_SPLINE_CURVE_WITH_KNOTS('',3,(#38070,#38071,#38072,#38073,#38074,
#38075,#38076,#38077,#38078,#38079),.UNSPECIFIED.,.F.,.F.,(4,2,2,2,4),(0.,
0.25,0.499999999999999,0.749999999999999,0.999999977827809),
 .UNSPECIFIED.);
#689=B_SPLINE_CURVE_WITH_KNOTS('',3,(#38109,#38110,#38111,#38112,#38113,
#38114,#38115,#38116,#38117,#38118,#38119,#38120,#38121),.UNSPECIFIED.,
 .F.,.F.,(4,3,3,3,4),(0.,0.0431918509065784,0.5,0.956806409099894,1.),
 .UNSPECIFIED.);
#690=B_SPLINE_CURVE_WITH_KNOTS('',3,(#38142,#38143,#38144,#38145,#38146,
#38147,#38148,#38149,#38150,#38151,#38152,#38153,#38154,#38155,#38156,#38157,
#38158,#38159,#38160,#38161,#38162,#38163,#38164,#38165,#38166,#38167,#38168,
#38169,#38170,#38171,#38172,#38173,#38174,#38175,#38176,#38177,#38178,#38179,
#38180,#38181,#38182,#38183,#38184,#38185,#38186,#38187,#38188,#38189,#38190,
#38191,#38192,#38193,#38194,#38195,#38196,#38197,#38198,#38199,#38200,#38201,
#38202,#38203,#38204,#38205,#38206,#38207,#38208,#38209,#38210,#38211,#38212,
#38213,#38214,#38215,#38216,#38217,#38218,#38219,#38220,#38221,#38222,#38223,
#38224,#38225,#38226,#38227,#38228,#38229,#38230,#38231,#38232,#38233,#38234,
#38235,#38236,#38237,#38238,#38239,#38240,#38241,#38242,#38243,#38244,#38245,
#38246,#38247,#38248,#38249,#38250,#38251,#38252,#38253,#38254,#38255,#38256,
#38257,#38258,#38259,#38260,#38261,#38262,#38263,#38264,#38265,#38266,#38267,
#38268,#38269,#38270,#38271,#38272,#38273,#38274,#38275,#38276,#38277,#38278,
#38279,#38280,#38281,#38282,#38283,#38284,#38285,#38286,#38287,#38288,#38289,
#38290,#38291,#38292,#38293,#38294,#38295,#38296,#38297,#38298,#38299,#38300,
#38301,#38302,#38303,#38304,#38305,#38306,#38307,#38308,#38309,#38310,#38311,
#38312,#38313,#38314,#38315,#38316,#38317,#38318,#38319,#38320,#38321,#38322,
#38323,#38324,#38325,#38326,#38327,#38328,#38329,#38330,#38331,#38332,#38333,
#38334,#38335,#38336,#38337,#38338,#38339,#38340,#38341,#38342,#38343,#38344,
#38345,#38346),.UNSPECIFIED.,.F.,.F.,(4,3,3,3,3,3,3,3,3,3,3,3,3,3,3,3,3,
3,3,3,3,3,3,3,3,3,3,3,3,3,3,3,3,3,3,3,3,3,3,3,3,3,3,3,3,3,3,3,3,3,3,3,3,
3,3,3,3,3,3,3,3,3,3,3,3,3,3,3,4),(0.,0.0249952040648666,0.0499029976050593,
0.0680454790691359,0.0924338447088906,0.107880913519564,0.131553995034703,
0.140984707740201,0.16395680048273,0.171035558612113,0.193345860441903,
0.199615480235769,0.218750000000002,0.227604280455894,0.234375000000003,
0.242187500000003,0.246093750000003,0.248046875000003,0.249023437500003,
0.250000000000003,0.254582622012608,0.280004563056784,0.307433325464391,
0.30946109206094,0.337151591946959,0.344194252878218,0.372025449866619,
0.384942334286463,0.412589612654437,0.429868562571756,0.457864931018828,
0.468749999999994,0.477270445734503,0.484374999999993,0.492187499999993,
0.496093749999992,0.498046874999992,0.499999999999992,0.531323458090248,
0.565671952103585,0.578524990186005,0.613136937556426,0.61640423603698,
0.648095328683626,0.674911251899195,0.697968240955163,0.718048375778514,
0.718749999999977,0.734374999999976,0.735668182771794,0.742187499999975,
0.746093749999975,0.748046874999975,0.749023437499975,0.749999999999975,
0.751820094958488,0.773837782688054,0.795119290834591,0.815755174137061,
0.835862819339601,0.855595765790536,0.874999999999987,0.875158502104443,
0.894772749621587,0.914585430706598,0.934770786003287,0.955587723025151,
0.977474708625959,0.999999988569583),.UNSPECIFIED.);
#691=B_SPLINE_CURVE_WITH_KNOTS('',3,(#38509,#38510,#38511,#38512,#38513,
#38514,#38515,#38516,#38517,#38518,#38519,#38520,#38521,#38522,#38523,#38524,
#38525,#38526,#38527,#38528,#38529,#38530,#38531,#38532,#38533,#38534,#38535,
#38536,#38537,#38538,#38539,#38540,#38541,#38542,#38543,#38544,#38545,#38546,
#38547,#38548,#38549,#38550,#38551,#38552,#38553,#38554,#38555,#38556,#38557,
#38558,#38559,#38560,#38561,#38562,#38563,#38564,#38565,#38566,#38567,#38568,
#38569,#38570,#38571,#38572,#38573,#38574,#38575,#38576,#38577,#38578,#38579,
#38580,#38581,#38582,#38583,#38584,#38585,#38586,#38587,#38588,#38589,#38590,
#38591,#38592,#38593,#38594,#38595,#38596,#38597,#38598,#38599,#38600,#38601,
#38602,#38603,#38604,#38605,#38606,#38607,#38608,#38609,#38610,#38611,#38612,
#38613,#38614,#38615,#38616,#38617,#38618,#38619,#38620,#38621,#38622,#38623,
#38624,#38625,#38626,#38627,#38628,#38629),.UNSPECIFIED.,.F.,.F.,(4,3,3,
3,3,3,3,3,3,3,3,3,3,3,3,3,3,3,3,3,3,3,3,3,3,3,3,3,3,3,3,3,3,3,3,3,3,3,3,
3,4),(7.98332897105801E-8,0.0312500598749729,0.0618422405072992,0.0934211202536609,
0.125000000000023,0.155569265149762,0.187159632574901,0.218750000000039,
0.234375000000042,0.242187500000044,0.246093750000044,0.248046875000045,
0.249023437500045,0.250000000000045,0.450377467746167,0.499981371599102,
0.500000000000075,0.625000000000089,0.687500000000097,0.718750000000101,
0.734375000000103,0.742187500000103,0.749511718750104,0.750000000000104,
0.765918986862788,0.781838152049637,0.79775750567844,0.813677171231473,
0.829597016624591,0.845517165313362,0.859375000000058,0.867187500000055,
0.871093750000053,0.873046875000052,0.874023437500052,0.875000000000052,
0.899836670682714,0.924877489292667,0.949727576111283,0.974863760616905,
0.999999945122527),.UNSPECIFIED.);
#692=B_SPLINE_CURVE_WITH_KNOTS('',3,(#38670,#38671,#38672,#38673,#38674,
#38675,#38676,#38677,#38678,#38679,#38680,#38681,#38682,#38683,#38684,#38685,
#38686,#38687,#38688,#38689,#38690,#38691,#38692,#38693,#38694,#38695,#38696,
#38697,#38698,#38699,#38700,#38701,#38702,#38703,#38704,#38705,#38706,#38707,
#38708,#38709,#38710,#38711,#38712,#38713,#38714,#38715,#38716,#38717,#38718),
 .UNSPECIFIED.,.F.,.F.,(4,3,3,3,3,3,3,3,3,3,3,3,3,3,3,3,4),(0.,0.0771288858376249,
0.118224466833141,0.199428832370291,0.25,0.333192391283466,0.35971949877537,
0.375000000000001,0.422997119033468,0.471428608082327,0.500000000000001,
0.602026122232166,0.703467968575276,0.719208889717013,0.820752755140426,
0.923561571449876,1.),.UNSPECIFIED.);
#693=B_SPLINE_CURVE_WITH_KNOTS('',3,(#38720,#38721,#38722,#38723,#38724,
#38725,#38726),.UNSPECIFIED.,.F.,.F.,(4,3,4),(0.,0.5,1.),.UNSPECIFIED.);
#694=B_SPLINE_CURVE_WITH_KNOTS('',3,(#38729,#38730,#38731,#38732,#38733,
#38734,#38735,#38736,#38737,#38738,#38739,#38740,#38741,#38742,#38743,#38744,
#38745,#38746,#38747,#38748,#38749,#38750,#38751,#38752,#38753,#38754,#38755,
#38756,#38757,#38758,#38759,#38760,#38761,#38762,#38763,#38764,#38765,#38766,
#38767,#38768,#38769,#38770,#38771,#38772,#38773,#38774,#38775,#38776,#38777,
#38778,#38779,#38780,#38781,#38782,#38783,#38784,#38785,#38786,#38787,#38788,
#38789),.UNSPECIFIED.,.F.,.F.,(4,3,3,3,3,3,3,3,3,3,3,3,3,3,3,3,3,3,3,3,
4),(0.,0.0723228733734608,0.149373740660938,0.166421151448187,0.245216396826458,
0.249999999999982,0.335716238671773,0.374999999999972,0.397180419852709,
0.437499999999968,0.468749999999969,0.48437499999997,0.495375830345444,
0.499999999999971,0.593362814881258,0.628795106216759,0.723805214627839,
0.824915510586949,0.849552874144399,0.955120141692627,1.),.UNSPECIFIED.);
#695=B_SPLINE_CURVE_WITH_KNOTS('',3,(#38830,#38831,#38832,#38833,#38834,
#38835,#38836,#38837,#38838,#38839,#38840,#38841,#38842,#38843,#38844,#38845,
#38846,#38847,#38848,#38849,#38850,#38851,#38852,#38853,#38854,#38855,#38856,
#38857,#38858,#38859,#38860,#38861,#38862,#38863,#38864,#38865,#38866,#38867,
#38868,#38869,#38870,#38871,#38872),.UNSPECIFIED.,.F.,.F.,(4,3,3,3,3,3,
3,3,3,3,3,3,3,3,4),(2.99705957294E-11,0.0832138091825946,0.218578168494638,
0.246109287965936,0.25,0.383459477745923,0.408370300217607,0.541180649747327,
0.570056216707183,0.702294204129991,0.731364949826117,0.75,0.881938317493617,
0.892442289989345,0.999999987394246),.UNSPECIFIED.);
#696=B_SPLINE_CURVE_WITH_KNOTS('',3,(#38873,#38874,#38875,#38876,#38877,
#38878,#38879,#38880,#38881,#38882,#38883,#38884,#38885,#38886,#38887,#38888,
#38889,#38890,#38891,#38892,#38893,#38894,#38895,#38896,#38897,#38898,#38899,
#38900,#38901,#38902,#38903,#38904,#38905,#38906,#38907,#38908,#38909,#38910,
#38911,#38912,#38913,#38914,#38915,#38916,#38917,#38918,#38919,#38920,#38921,
#38922,#38923,#38924,#38925,#38926,#38927,#38928,#38929,#38930,#38931,#38932,
#38933,#38934,#38935,#38936,#38937,#38938,#38939,#38940,#38941,#38942,#38943,
#38944,#38945,#38946,#38947,#38948,#38949,#38950,#38951),.UNSPECIFIED.,
 .F.,.F.,(4,3,3,3,3,3,3,3,3,3,3,3,3,3,3,3,3,3,3,3,3,3,3,3,3,3,4),(0.,0.0457810664062895,
0.0917889143914393,0.120317290917192,0.1428571428571,0.198222944257388,
0.253550325461388,0.275526256355529,0.2857142857143,0.349641048829855,0.41364518951731,
0.4285714285714,0.430597609456488,0.496176324090972,0.561795552687674,0.5714285714286,
0.585374526667744,0.649830120476722,0.7142857142857,0.740396273233819,0.795252877513523,
0.850177989920913,0.8571428571429,0.895765393026058,0.94186342671897,0.987754574481698,
0.999999797061768),.UNSPECIFIED.);
#697=B_SPLINE_CURVE_WITH_KNOTS('',3,(#38987,#38988,#38989,#38990,#38991,
#38992,#38993,#38994,#38995,#38996,#38997,#38998,#38999,#39000,#39001,#39002,
#39003,#39004,#39005,#39006,#39007,#39008,#39009,#39010,#39011,#39012,#39013,
#39014,#39015,#39016,#39017,#39018,#39019,#39020,#39021,#39022,#39023,#39024,
#39025,#39026,#39027,#39028,#39029,#39030,#39031,#39032,#39033,#39034,#39035,
#39036,#39037,#39038,#39039,#39040,#39041,#39042,#39043,#39044,#39045,#39046,
#39047),.UNSPECIFIED.,.F.,.F.,(4,3,3,3,3,3,3,3,3,3,3,3,3,3,3,3,3,3,3,3,
4),(5.6316964680001E-11,0.100718446959904,0.175359223479952,0.23866647207507,
0.25,0.301429678396237,0.351106896227335,0.399999481032942,0.449999740516471,
0.497447897994334,0.5,0.500001693682381,0.547538310465323,0.598153732848992,
0.647547504212216,0.698773752106108,0.75,0.812847820507721,0.887998910942513,
0.987406932145145,0.999999999944183),.UNSPECIFIED.);
#698=B_SPLINE_CURVE_WITH_KNOTS('',3,(#39088,#39089,#39090,#39091,#39092,
#39093,#39094,#39095,#39096,#39097,#39098,#39099,#39100,#39101,#39102,#39103,
#39104,#39105,#39106,#39107,#39108,#39109,#39110,#39111,#39112,#39113,#39114,
#39115,#39116,#39117,#39118,#39119,#39120,#39121,#39122,#39123,#39124,#39125,
#39126,#39127,#39128,#39129,#39130,#39131,#39132,#39133,#39134,#39135,#39136,
#39137,#39138,#39139,#39140,#39141,#39142,#39143,#39144,#39145,#39146,#39147,
#39148,#39149,#39150,#39151,#39152,#39153,#39154,#39155,#39156,#39157,#39158,
#39159,#39160,#39161,#39162,#39163,#39164,#39165,#39166,#39167,#39168,#39169,
#39170,#39171,#39172),.UNSPECIFIED.,.F.,.F.,(4,3,3,3,3,3,3,3,3,3,3,3,3,
3,3,3,3,3,3,3,3,3,3,3,3,3,3,3,4),(0.,0.0661535075836036,0.118578546619141,
0.125,0.187500000000001,0.218750000000001,0.234375000000001,0.243852058161108,
0.250000000000001,0.272481796236854,0.339700986415693,0.406654744578485,
0.424962283673657,0.491652042830103,0.500000000000001,0.565705494396537,
0.575150315587252,0.625000000000002,0.687500000000002,0.718750000000002,
0.727633374502205,0.734375000000002,0.743881940457977,0.750000000000002,
0.81217804106019,0.876338528453975,0.881522335850663,0.948429399218141,
1.),.UNSPECIFIED.);
#699=B_SPLINE_CURVE_WITH_KNOTS('',3,(#39213,#39214,#39215,#39216,#39217,
#39218,#39219),.UNSPECIFIED.,.F.,.F.,(4,3,4),(0.,0.5,0.999999999983266),
 .UNSPECIFIED.);
#700=B_SPLINE_CURVE_WITH_KNOTS('',3,(#39221,#39222,#39223,#39224,#39225,
#39226,#39227,#39228,#39229,#39230,#39231,#39232,#39233,#39234,#39235,#39236,
#39237,#39238,#39239,#39240,#39241,#39242,#39243,#39244,#39245,#39246,#39247,
#39248,#39249,#39250,#39251,#39252,#39253,#39254,#39255,#39256,#39257,#39258,
#39259,#39260),.UNSPECIFIED.,.F.,.F.,(4,3,3,3,3,3,3,3,3,3,3,3,3,4),(0.,
0.0902944655942792,0.118857317205525,0.250000000000005,0.363581344799241,
0.437500000000004,0.466152583196255,0.495170166310217,0.500000000000003,
0.615785321950757,0.718419711847765,0.827854048242836,0.933927707021626,
0.999999999999981),.UNSPECIFIED.);
#701=B_SPLINE_CURVE_WITH_KNOTS('',3,(#39261,#39262,#39263,#39264,#39265,
#39266,#39267,#39268,#39269,#39270,#39271,#39272,#39273,#39274,#39275,#39276,
#39277,#39278,#39279,#39280,#39281,#39282,#39283,#39284,#39285,#39286,#39287,
#39288,#39289,#39290,#39291,#39292,#39293,#39294,#39295,#39296,#39297,#39298,
#39299,#39300,#39301,#39302,#39303,#39304,#39305,#39306,#39307,#39308,#39309,
#39310,#39311,#39312,#39313,#39314,#39315,#39316,#39317,#39318),
 .UNSPECIFIED.,.F.,.F.,(4,3,3,3,3,3,3,3,3,3,3,3,3,3,3,3,3,3,3,4),(0.,0.105552984689735,
0.150464224794851,0.250000000000038,0.345315709929821,0.371222912678605,
0.375000000000057,0.437500000000066,0.468750000000071,0.484375000000072,
0.494785170063038,0.500000000000074,0.58959223919739,0.602892053414376,
0.690489305247616,0.771089123956182,0.833650045697548,0.911000967360328,
0.983433814593619,1.),.UNSPECIFIED.);
#702=B_SPLINE_CURVE_WITH_KNOTS('',3,(#39364,#39365,#39366,#39367,#39368,
#39369,#39370,#39371,#39372,#39373,#39374,#39375,#39376,#39377,#39378,#39379,
#39380,#39381,#39382,#39383,#39384,#39385,#39386,#39387,#39388,#39389,#39390,
#39391,#39392,#39393,#39394,#39395,#39396,#39397,#39398,#39399,#39400,#39401,
#39402,#39403,#39404,#39405,#39406,#39407,#39408,#39409,#39410,#39411,#39412,
#39413,#39414,#39415,#39416,#39417,#39418,#39419,#39420,#39421,#39422,#39423,
#39424,#39425,#39426,#39427,#39428,#39429,#39430,#39431,#39432,#39433,#39434,
#39435,#39436),.UNSPECIFIED.,.F.,.F.,(4,3,3,3,3,3,3,3,3,3,3,3,3,3,3,3,3,
3,3,3,3,3,3,3,4),(0.,0.0458328892178335,0.0918178602034833,0.137727870849418,
0.1428571428571,0.14853659813257,0.203804992723845,0.259124754689577,0.2857142857143,
0.296137570174493,0.362354499372946,0.4285714285714,0.443717909280358,0.511006798196711,
0.5714285714286,0.591516277431817,0.658633939614426,0.7142857142857,0.739436741598696,
0.798289799370798,0.8571428571429,0.887213042157008,0.9335242764972,0.979590782772933,
1.),.UNSPECIFIED.);
#703=B_SPLINE_CURVE_WITH_KNOTS('',3,(#39439,#39440,#39441,#39442,#39443,
#39444,#39445,#39446,#39447,#39448,#39449,#39450,#39451,#39452,#39453,#39454,
#39455,#39456,#39457,#39458,#39459,#39460,#39461,#39462,#39463,#39464,#39465,
#39466,#39467,#39468,#39469,#39470,#39471,#39472,#39473,#39474,#39475,#39476,
#39477,#39478),.UNSPECIFIED.,.F.,.F.,(4,3,3,3,3,3,3,3,3,3,3,3,3,4),(0.,
0.132990593054672,0.153369582492901,0.288984795668459,0.306719318472942,
0.443622679891926,0.460361901548923,0.597256080254731,0.614811262496377,
0.75,0.769627678792761,0.909364409081581,0.924609577548183,0.999999999966827),
 .UNSPECIFIED.);
#704=B_SPLINE_CURVE_WITH_KNOTS('',3,(#39501,#39502,#39503,#39504,#39505,
#39506,#39507,#39508,#39509,#39510),.UNSPECIFIED.,.F.,.F.,(4,3,3,4),(0.,
0.3333333333333,0.6666666666667,1.),.UNSPECIFIED.);
#705=B_SPLINE_CURVE_WITH_KNOTS('',3,(#39646,#39647,#39648,#39649,#39650,
#39651,#39652,#39653,#39654,#39655,#39656,#39657,#39658,#39659,#39660,#39661,
#39662,#39663,#39664,#39665,#39666,#39667,#39668,#39669,#39670,#39671,#39672,
#39673,#39674,#39675,#39676,#39677,#39678,#39679,#39680,#39681,#39682,#39683,
#39684,#39685,#39686,#39687,#39688,#39689,#39690,#39691,#39692,#39693,#39694,
#39695,#39696,#39697,#39698,#39699,#39700,#39701,#39702,#39703,#39704,#39705,
#39706,#39707,#39708,#39709,#39710,#39711,#39712,#39713,#39714,#39715,#39716,
#39717,#39718,#39719,#39720,#39721,#39722,#39723,#39724,#39725,#39726,#39727,
#39728,#39729,#39730,#39731,#39732),.UNSPECIFIED.,.F.,.F.,(4,2,2,1,2,2,
2,1,1,1,2,2,2,2,1,1,1,2,2,2,2,2,2,2,2,1,1,2,2,2,1,1,2,2,2,2,1,1,2,2,2,2,
1,1,2,2,2,1,1,2,2,4),(0.,0.0312500000000048,0.0468750000000071,0.0546875000000082,
0.0585937500000085,0.0625000000000087,0.0937500000000093,0.10937500000001,
0.11718750000001,0.12109375000001,0.12304687500001,0.12500000000001,0.187500000000013,
0.218750000000014,0.234375000000015,0.242187500000015,0.246093750000016,
0.248046875000016,0.250000000000016,0.312500000000016,0.343750000000015,
0.359375000000015,0.375000000000015,0.437500000000015,0.468750000000016,
0.484375000000016,0.492187500000016,0.496093750000016,0.500000000000016,
0.562500000000016,0.593750000000016,0.609375000000016,0.617187500000016,
0.625000000000016,0.687500000000016,0.718750000000016,0.734375000000016,
0.742187500000016,0.746093750000016,0.750000000000016,0.812500000000014,
0.843750000000013,0.859375000000013,0.867187500000013,0.871093750000012,
0.875000000000012,0.906250000000011,0.92187500000001,0.92968750000001,0.933593750000009,
0.937500000000009,1.),.UNSPECIFIED.);
#706=B_SPLINE_CURVE_WITH_KNOTS('',3,(#39735,#39736,#39737,#39738,#39739,
#39740,#39741,#39742,#39743,#39744,#39745,#39746,#39747,#39748,#39749,#39750,
#39751,#39752,#39753,#39754,#39755,#39756,#39757,#39758,#39759,#39760,#39761,
#39762,#39763,#39764,#39765,#39766,#39767,#39768,#39769,#39770,#39771,#39772,
#39773,#39774,#39775,#39776,#39777,#39778,#39779,#39780,#39781,#39782,#39783,
#39784,#39785,#39786,#39787,#39788,#39789,#39790,#39791,#39792,#39793,#39794,
#39795,#39796,#39797,#39798,#39799,#39800,#39801,#39802,#39803,#39804,#39805,
#39806,#39807,#39808,#39809,#39810,#39811,#39812,#39813,#39814,#39815,#39816,
#39817,#39818,#39819,#39820,#39821,#39822,#39823,#39824,#39825,#39826,#39827,
#39828,#39829,#39830,#39831,#39832,#39833,#39834,#39835,#39836,#39837,#39838,
#39839,#39840,#39841,#39842,#39843,#39844,#39845,#39846,#39847,#39848,#39849,
#39850,#39851,#39852,#39853,#39854,#39855,#39856,#39857,#39858,#39859,#39860,
#39861,#39862,#39863,#39864,#39865,#39866,#39867,#39868,#39869,#39870,#39871,
#39872,#39873,#39874,#39875,#39876,#39877,#39878,#39879,#39880,#39881,#39882,
#39883,#39884,#39885,#39886,#39887,#39888,#39889,#39890,#39891,#39892,#39893,
#39894,#39895,#39896,#39897,#39898,#39899,#39900,#39901,#39902,#39903,#39904,
#39905,#39906,#39907,#39908,#39909,#39910,#39911,#39912,#39913,#39914,#39915,
#39916,#39917,#39918,#39919,#39920,#39921),.UNSPECIFIED.,.F.,.F.,(4,3,3,
3,3,3,3,3,3,3,3,3,3,3,3,3,3,3,3,3,3,3,3,3,3,3,3,3,3,3,3,3,3,3,3,3,3,3,3,
3,3,3,3,3,3,3,3,3,3,3,3,3,3,3,3,3,3,3,3,3,3,3,4),(7.50078281829221E-8,2.18347309079937E-7,
0.0229487363769535,0.0291144599814069,0.0509742552696368,0.0551846684308731,
0.062499999999996,0.0795332519016023,0.100117540398566,0.102945588654808,
0.109374999999993,0.117187499999992,0.121093749999992,0.123046874999992,
0.124511718749992,0.124999999999992,0.126823526748048,0.154172375961179,
0.168540269274348,0.195094650684728,0.207813798624315,0.234374999999993,
0.243585986145407,0.245603686859174,0.249999999999993,0.28646503409748,
0.323181702761501,0.335381864186567,0.372223006657599,0.396063887874889,
0.433025218886611,0.468749999999996,0.471320710204426,0.484374999999996,
0.492187499999996,0.499324683781458,0.499999999999996,0.539362467141619,
0.553200429548843,0.592481915029558,0.619371300972094,0.65850546985717,
0.673128963060043,0.711994605162659,0.716726220534974,0.718749999999999,
0.734374999999999,0.742187499999999,0.746093749999999,0.749489064792616,
0.749999999999999,0.753696015195325,0.789783408896454,0.822481143086698,
0.851891042285857,0.878120703107442,0.901492063881429,0.9224109344836,0.941272872505627,
0.958424456266756,0.974021159408361,0.988170760125037,1.),.UNSPECIFIED.);
#707=B_SPLINE_CURVE_WITH_KNOTS('',3,(#39958,#39959,#39960,#39961,#39962,
#39963,#39964,#39965,#39966,#39967),.UNSPECIFIED.,.F.,.F.,(4,2,2,2,4),(2.21660101455866E-8,
0.25,0.5,0.75,1.),.UNSPECIFIED.);
#708=B_SPLINE_CURVE_WITH_KNOTS('',3,(#39968,#39969,#39970,#39971,#39972,
#39973,#39974,#39975,#39976,#39977,#39978,#39979,#39980,#39981,#39982,#39983,
#39984,#39985,#39986,#39987,#39988,#39989,#39990,#39991,#39992,#39993,#39994,
#39995,#39996,#39997,#39998,#39999,#40000,#40001,#40002,#40003,#40004,#40005,
#40006,#40007,#40008,#40009,#40010,#40011,#40012,#40013,#40014,#40015,#40016,
#40017,#40018,#40019,#40020,#40021,#40022,#40023,#40024,#40025,#40026,#40027,
#40028),.UNSPECIFIED.,.F.,.F.,(4,3,3,3,3,3,3,3,3,3,3,3,3,3,3,3,3,3,3,3,
4),(5.84282689630331E-11,0.10071860689625,0.175359303448125,0.238666822178488,
0.25,0.30143097883946,0.35110935564115,0.400003027959161,0.450001513979581,
0.497450659112773,0.5,0.500002157722716,0.547539602846247,0.598154702134685,
0.647549372595313,0.698774686297657,0.75,0.812847367231791,0.887996855249994,
0.987406130706481,0.99999999994403),.UNSPECIFIED.);
#709=B_SPLINE_CURVE_WITH_KNOTS('',3,(#40071,#40072,#40073,#40074,#40075,
#40076,#40077,#40078,#40079,#40080,#40081,#40082,#40083,#40084,#40085,#40086,
#40087,#40088,#40089,#40090,#40091,#40092,#40093,#40094,#40095,#40096,#40097,
#40098,#40099,#40100,#40101,#40102,#40103,#40104,#40105,#40106,#40107,#40108,
#40109,#40110,#40111,#40112,#40113,#40114,#40115,#40116,#40117,#40118,#40119,
#40120,#40121,#40122,#40123,#40124,#40125,#40126,#40127,#40128,#40129,#40130,
#40131,#40132,#40133,#40134,#40135,#40136,#40137,#40138,#40139,#40140,#40141,
#40142,#40143,#40144,#40145,#40146,#40147,#40148,#40149,#40150,#40151,#40152,
#40153,#40154,#40155,#40156,#40157,#40158,#40159,#40160,#40161,#40162,#40163,
#40164,#40165,#40166,#40167,#40168,#40169,#40170,#40171,#40172,#40173,#40174,
#40175,#40176),.UNSPECIFIED.,.F.,.F.,(4,3,3,3,3,3,3,3,3,3,3,3,3,3,3,3,3,
3,3,3,3,3,3,3,3,3,3,3,3,3,3,3,3,3,3,4),(0.,0.0534073021192575,0.105850843534235,
0.121448216935405,0.124999999999998,0.17639020141179,0.187499999999997,
0.218749999999996,0.234374999999996,0.242187499999996,0.246093749999996,
0.249763585925269,0.249999999999996,0.272897684871302,0.338775824548075,
0.402712273103291,0.425593601158696,0.490426704513184,0.499999999999998,
0.564257404599829,0.574134006701701,0.624999999999999,0.6875,0.71875,0.726818737615628,
0.734375,0.7421875,0.74609375,0.749803046606295,0.75,0.80028432490764,0.851651062187545,
0.878254012626795,0.931592833707594,0.986051689536171,1.),.UNSPECIFIED.);
#710=B_SPLINE_CURVE_WITH_KNOTS('',3,(#40215,#40216,#40217,#40218,#40219,
#40220,#40221,#40222,#40223,#40224,#40225,#40226,#40227,#40228,#40229,#40230,
#40231,#40232,#40233,#40234,#40235,#40236,#40237,#40238,#40239,#40240,#40241,
#40242,#40243,#40244,#40245,#40246,#40247,#40248,#40249,#40250,#40251,#40252,
#40253,#40254,#40255,#40256,#40257,#40258,#40259,#40260,#40261,#40262,#40263),
 .UNSPECIFIED.,.F.,.F.,(4,3,3,3,3,3,3,3,3,3,3,3,3,3,3,3,4),(0.,0.0770829582185647,
0.115833104658598,0.197028807512659,0.249999999999993,0.333153117361608,
0.356333767149255,0.374999999999989,0.422947860085873,0.471329029702914,
0.499999999999989,0.606855024408351,0.708280894829689,0.713710048816712,
0.815228553348316,0.918005904185723,1.),.UNSPECIFIED.);
#711=B_SPLINE_CURVE_WITH_KNOTS('',3,(#40264,#40265,#40266,#40267,#40268,
#40269,#40270),.UNSPECIFIED.,.F.,.F.,(4,3,4),(2.44821180092488E-11,0.5,
0.999999979802023),.UNSPECIFIED.);
#712=B_SPLINE_CURVE_WITH_KNOTS('',3,(#40271,#40272,#40273,#40274,#40275,
#40276,#40277,#40278,#40279,#40280,#40281,#40282,#40283,#40284,#40285,#40286,
#40287,#40288,#40289,#40290,#40291,#40292,#40293,#40294,#40295,#40296,#40297,
#40298,#40299,#40300,#40301,#40302,#40303,#40304,#40305,#40306,#40307,#40308,
#40309,#40310,#40311,#40312,#40313,#40314,#40315,#40316,#40317,#40318,#40319,
#40320,#40321,#40322,#40323,#40324,#40325,#40326,#40327,#40328),
 .UNSPECIFIED.,.F.,.F.,(4,3,3,3,3,3,3,3,3,3,3,3,3,3,3,3,3,3,3,4),(0.,0.0715675761621514,
0.147880847450542,0.168247999802698,0.250000000000023,0.335016489680616,
0.375000000000033,0.399721616125445,0.437500000000038,0.468750000000039,
0.48437500000004,0.49533835708464,0.500000000000041,0.593368467641783,0.631329958382462,
0.726440385039814,0.827653147299548,0.852289986581864,0.957929667074719,
1.),.UNSPECIFIED.);
#713=B_SPLINE_CURVE_WITH_KNOTS('',3,(#40371,#40372,#40373,#40374,#40375,
#40376,#40377,#40378,#40379,#40380,#40381,#40382,#40383,#40384,#40385,#40386,
#40387,#40388,#40389,#40390,#40391,#40392),.UNSPECIFIED.,.F.,.F.,(4,3,3,
3,3,3,3,4),(1.01036450470102E-7,0.1428571428571,0.2857142857143,0.4285714285714,
0.5714285714286,0.7142857142857,0.8571428571429,1.),.UNSPECIFIED.);
#714=B_SPLINE_CURVE_WITH_KNOTS('',3,(#40435,#40436,#40437,#40438,#40439,
#40440,#40441),.UNSPECIFIED.,.F.,.F.,(4,3,4),(2.1506060516552E-8,0.5,0.99999999998187),
 .UNSPECIFIED.);
#715=B_SPLINE_CURVE_WITH_KNOTS('',3,(#40443,#40444,#40445,#40446,#40447,
#40448,#40449,#40450,#40451,#40452,#40453,#40454,#40455,#40456,#40457,#40458,
#40459,#40460,#40461,#40462,#40463,#40464,#40465,#40466,#40467,#40468,#40469,
#40470,#40471,#40472,#40473,#40474,#40475,#40476,#40477,#40478,#40479,#40480,
#40481,#40482,#40483,#40484,#40485),.UNSPECIFIED.,.F.,.F.,(4,3,3,3,3,3,
3,3,3,3,3,3,3,3,4),(0.,0.0900137143300672,0.116403415329186,0.243030893620983,
0.25,0.360149316915376,0.4375,0.466162190612914,0.495189352431254,0.5,0.615787612830892,
0.712806427318202,0.822400533667193,0.928574394609824,1.),.UNSPECIFIED.);
#716=B_SPLINE_CURVE_WITH_KNOTS('',3,(#40486,#40487,#40488,#40489,#40490,
#40491,#40492,#40493,#40494,#40495,#40496,#40497,#40498,#40499,#40500,#40501,
#40502,#40503,#40504,#40505,#40506,#40507,#40508,#40509,#40510,#40511,#40512,
#40513,#40514,#40515,#40516,#40517,#40518,#40519,#40520,#40521,#40522,#40523,
#40524,#40525,#40526,#40527,#40528,#40529,#40530,#40531,#40532,#40533,#40534,
#40535,#40536,#40537,#40538,#40539,#40540,#40541,#40542,#40543),
 .UNSPECIFIED.,.F.,.F.,(4,3,3,3,3,3,3,3,3,3,3,3,3,3,3,3,3,3,3,4),(0.,0.105620946107267,
0.147712755041571,0.250000000000056,0.345332766185357,0.368665276576495,
0.375000000000084,0.437500000000099,0.468750000000106,0.484375000000107,
0.494735183221286,0.500000000000108,0.589017398444796,0.600284329803979,
0.686110181738736,0.750000000000054,0.831760754742984,0.908457269195526,
0.980208706438598,1.),.UNSPECIFIED.);
#717=B_SPLINE_CURVE_WITH_KNOTS('',3,(#40585,#40586,#40587,#40588,#40589,
#40590,#40591,#40592,#40593,#40594,#40595,#40596,#40597,#40598,#40599,#40600,
#40601,#40602,#40603,#40604,#40605,#40606),.UNSPECIFIED.,.F.,.F.,(4,3,3,
3,3,3,3,4),(0.,0.1428571428571,0.2857142857143,0.4285714285714,0.5714285714286,
0.7142857142857,0.8571428571429,0.999999898936422),.UNSPECIFIED.);
#718=B_SPLINE_CURVE_WITH_KNOTS('',3,(#40609,#40610,#40611,#40612,#40613,
#40614,#40615,#40616,#40617,#40618),.UNSPECIFIED.,.F.,.F.,(4,2,2,2,4),(0.,
0.25,0.5,0.75,0.999999977827818),.UNSPECIFIED.);
#719=B_SPLINE_CURVE_WITH_KNOTS('',3,(#40648,#40649,#40650,#40651,#40652,
#40653,#40654,#40655,#40656,#40657,#40658,#40659,#40660),.UNSPECIFIED.,
 .F.,.F.,(4,3,3,3,4),(0.,0.0431918509093698,0.5,0.956806409091625,1.),
 .UNSPECIFIED.);
#720=B_SPLINE_CURVE_WITH_KNOTS('',3,(#40681,#40682,#40683,#40684,#40685,
#40686,#40687,#40688,#40689,#40690,#40691,#40692,#40693,#40694,#40695,#40696,
#40697,#40698,#40699,#40700,#40701,#40702,#40703,#40704,#40705,#40706,#40707,
#40708,#40709,#40710,#40711,#40712,#40713,#40714,#40715,#40716,#40717,#40718,
#40719,#40720,#40721,#40722,#40723,#40724,#40725,#40726,#40727,#40728,#40729,
#40730,#40731,#40732,#40733,#40734,#40735,#40736,#40737,#40738,#40739,#40740,
#40741,#40742,#40743,#40744,#40745,#40746,#40747,#40748,#40749,#40750,#40751,
#40752,#40753,#40754,#40755,#40756,#40757,#40758,#40759,#40760,#40761,#40762,
#40763,#40764,#40765,#40766,#40767,#40768,#40769,#40770,#40771,#40772,#40773,
#40774,#40775,#40776,#40777,#40778,#40779,#40780,#40781,#40782,#40783,#40784,
#40785,#40786,#40787,#40788,#40789,#40790,#40791,#40792,#40793,#40794,#40795,
#40796,#40797,#40798,#40799,#40800,#40801,#40802,#40803,#40804,#40805,#40806,
#40807,#40808,#40809,#40810,#40811,#40812,#40813,#40814,#40815,#40816,#40817,
#40818,#40819,#40820,#40821,#40822,#40823,#40824,#40825,#40826,#40827,#40828,
#40829,#40830,#40831,#40832,#40833,#40834,#40835,#40836,#40837,#40838,#40839,
#40840,#40841,#40842,#40843,#40844,#40845,#40846,#40847,#40848,#40849,#40850,
#40851,#40852,#40853,#40854,#40855,#40856,#40857,#40858,#40859,#40860,#40861,
#40862,#40863,#40864,#40865,#40866,#40867,#40868,#40869,#40870,#40871,#40872,
#40873,#40874,#40875,#40876,#40877,#40878,#40879,#40880,#40881,#40882,#40883,
#40884,#40885),.UNSPECIFIED.,.F.,.F.,(4,3,3,3,3,3,3,3,3,3,3,3,3,3,3,3,3,
3,3,3,3,3,3,3,3,3,3,3,3,3,3,3,3,3,3,3,3,3,3,3,3,3,3,3,3,3,3,3,3,3,3,3,3,
3,3,3,3,3,3,3,3,3,3,3,3,3,3,3,4),(0.,0.0249899757898509,0.0498925985927389,
0.0680547145672805,0.0924380116089264,0.107884502821677,0.131552669723352,
0.140982390017907,0.163949714740866,0.171027459458805,0.19333313068864,
0.199601692626754,0.218749999999987,0.227584804003973,0.234374999999986,
0.242187499999986,0.246093749999986,0.248046874999986,0.249023437499986,
0.249999999999986,0.254563033347897,0.279986528061362,0.307418668000935,
0.309444125572636,0.337138172534275,0.344177504666389,0.372012337381321,
0.384925968447627,0.41257692077012,0.429852529706512,0.457852628540933,
0.468749999999996,0.477253131218569,0.484374999999997,0.492187499999998,
0.496093749999998,0.498046874999998,0.499999999999998,0.531304980715094,
0.565655536933447,0.578514455459115,0.613128561202045,0.616399033761582,
0.648094081067902,0.674913002638068,0.697972341505022,0.718054360421838,
0.718750000000008,0.734375000000008,0.735675698049429,0.742187500000009,
0.746093750000009,0.748046875000009,0.749023437500009,0.750000000000009,
0.75183323557947,0.773849534001207,0.795129686077898,0.815764243845486,
0.835870588208117,0.855602251914255,0.875000000000005,0.875163715889217,
0.894776692921227,0.914588112884019,0.93477223603792,0.955588003084658,
0.977473939702512,0.999999988549721),.UNSPECIFIED.);
#721=B_SPLINE_CURVE_WITH_KNOTS('',3,(#41048,#41049,#41050,#41051,#41052,
#41053,#41054,#41055,#41056,#41057,#41058,#41059,#41060,#41061,#41062,#41063,
#41064,#41065,#41066,#41067,#41068,#41069,#41070,#41071,#41072,#41073,#41074,
#41075,#41076,#41077,#41078,#41079,#41080,#41081,#41082,#41083,#41084,#41085,
#41086,#41087,#41088,#41089,#41090,#41091,#41092,#41093,#41094,#41095,#41096,
#41097,#41098,#41099,#41100,#41101,#41102,#41103,#41104,#41105,#41106,#41107,
#41108,#41109,#41110,#41111,#41112,#41113,#41114,#41115,#41116,#41117,#41118,
#41119,#41120,#41121,#41122,#41123,#41124,#41125,#41126,#41127,#41128,#41129,
#41130,#41131,#41132,#41133,#41134,#41135,#41136,#41137,#41138,#41139,#41140,
#41141,#41142,#41143,#41144,#41145,#41146,#41147,#41148,#41149,#41150,#41151,
#41152,#41153,#41154,#41155,#41156,#41157,#41158,#41159,#41160,#41161,#41162,
#41163,#41164,#41165,#41166,#41167,#41168),.UNSPECIFIED.,.F.,.F.,(4,3,3,
3,3,3,3,3,3,3,3,3,3,3,3,3,3,3,3,3,3,3,3,3,3,3,3,3,3,3,3,3,3,3,3,3,3,3,3,
3,4),(7.98332591227906E-8,0.0312500598749484,0.0618422377334466,0.0934211188667314,
0.125000000000016,0.155569262381823,0.187159631190926,0.218750000000029,
0.234375000000031,0.242187500000032,0.246093750000032,0.248046875000032,
0.249023437500033,0.250000000000033,0.450348688189998,0.499981342333456,
0.500000000000063,0.625000000000078,0.687500000000086,0.71875000000009,
0.734375000000092,0.742187500000092,0.749511718750093,0.750000000000093,
0.76591902426714,0.781838226860177,0.797757617896502,0.813677320857265,
0.829597203658077,0.845517389752812,0.859375000000061,0.867187500000059,
0.871093750000058,0.873046875000057,0.874023437500057,0.875000000000056,
0.899836748384693,0.924877547569079,0.949727712244665,0.974863828683451,
0.999999945122236),.UNSPECIFIED.);
#722=B_SPLINE_CURVE_WITH_KNOTS('',3,(#41209,#41210,#41211,#41212,#41213,
#41214,#41215,#41216,#41217,#41218,#41219,#41220,#41221,#41222,#41223,#41224,
#41225,#41226,#41227,#41228,#41229,#41230,#41231,#41232,#41233,#41234,#41235,
#41236,#41237,#41238,#41239,#41240,#41241,#41242,#41243,#41244,#41245,#41246,
#41247,#41248,#41249,#41250,#41251,#41252,#41253,#41254,#41255,#41256,#41257),
 .UNSPECIFIED.,.F.,.F.,(4,3,3,3,3,3,3,3,3,3,3,3,3,3,3,3,4),(0.,0.0771290273449875,
0.118224704472258,0.199429219826042,0.250000000000003,0.333192555504809,
0.359720294597202,0.375000000000003,0.422998467267463,0.471431284351993,
0.500000000000003,0.602025867947538,0.703467460959905,0.719209589455199,
0.820753199246495,0.923561758329389,1.),.UNSPECIFIED.);
#723=B_SPLINE_CURVE_WITH_KNOTS('',3,(#41259,#41260,#41261,#41262,#41263,
#41264,#41265),.UNSPECIFIED.,.F.,.F.,(4,3,4),(2.58811215489952E-11,0.5,
1.),.UNSPECIFIED.);
#724=B_SPLINE_CURVE_WITH_KNOTS('',3,(#41268,#41269,#41270,#41271,#41272,
#41273,#41274,#41275,#41276,#41277,#41278,#41279,#41280,#41281,#41282,#41283,
#41284,#41285,#41286,#41287,#41288,#41289,#41290,#41291,#41292,#41293,#41294,
#41295,#41296,#41297,#41298,#41299,#41300,#41301,#41302,#41303,#41304,#41305,
#41306,#41307,#41308,#41309,#41310,#41311,#41312,#41313,#41314,#41315,#41316,
#41317,#41318,#41319,#41320,#41321,#41322,#41323,#41324,#41325,#41326,#41327,
#41328),.UNSPECIFIED.,.F.,.F.,(4,3,3,3,3,3,3,3,3,3,3,3,3,3,3,3,3,3,3,3,
4),(0.,0.0723226571286148,0.149373391393564,0.166421306541277,0.245216470047908,
0.249999999999981,0.335716357982209,0.374999999999975,0.397180576939525,
0.437499999999972,0.468749999999974,0.484374999999974,0.495375838037244,
0.499999999999974,0.593362829860859,0.628795108092315,0.723805230530685,
0.824915540841586,0.849552880666,0.955120161906881,1.),.UNSPECIFIED.);
#725=B_SPLINE_CURVE_WITH_KNOTS('',3,(#41369,#41370,#41371,#41372,#41373,
#41374,#41375,#41376,#41377,#41378,#41379,#41380,#41381,#41382,#41383,#41384,
#41385,#41386,#41387,#41388,#41389,#41390,#41391,#41392,#41393,#41394,#41395,
#41396,#41397,#41398,#41399,#41400,#41401,#41402,#41403,#41404,#41405,#41406,
#41407,#41408,#41409,#41410,#41411),.UNSPECIFIED.,.F.,.F.,(4,3,3,3,3,3,
3,3,3,3,3,3,3,3,4),(1.98991421892558E-11,0.0832138081695056,0.218577781387173,
0.246109287404286,0.25,0.383459488805014,0.408370299490802,0.541180660031661,
0.570056215972447,0.702294214224038,0.731364949239141,0.75,0.881938328104128,
0.892442289703727,0.999999987394212),.UNSPECIFIED.);
#726=B_SPLINE_CURVE_WITH_KNOTS('',3,(#41412,#41413,#41414,#41415,#41416,
#41417,#41418,#41419,#41420,#41421,#41422,#41423,#41424,#41425,#41426,#41427,
#41428,#41429,#41430,#41431,#41432,#41433,#41434,#41435,#41436,#41437,#41438,
#41439,#41440,#41441,#41442,#41443,#41444,#41445,#41446,#41447,#41448,#41449,
#41450,#41451,#41452,#41453,#41454,#41455,#41456,#41457,#41458,#41459,#41460,
#41461,#41462,#41463,#41464,#41465,#41466,#41467,#41468,#41469,#41470,#41471,
#41472,#41473,#41474,#41475,#41476,#41477,#41478,#41479,#41480,#41481,#41482,
#41483,#41484,#41485,#41486,#41487,#41488,#41489,#41490),.UNSPECIFIED.,
 .F.,.F.,(4,3,3,3,3,3,3,3,3,3,3,3,3,3,3,3,3,3,3,3,3,3,3,3,3,3,4),(0.,0.0457810663886033,
0.0917889143557284,0.120317290916942,0.1428571428571,0.198222944263035,
0.253550325472813,0.275526256355525,0.2857142857143,0.349641048844645,0.413645189546886,
0.4285714285714,0.43059760945638,0.496176324094908,0.561795552695129,0.5714285714286,
0.585374526667842,0.649830120476771,0.7142857142857,0.740396273234167,0.795252877507973,
0.850177989909437,0.8571428571429,0.895765393025868,0.941863426735384,0.987754574515315,
0.999999797061845),.UNSPECIFIED.);
#727=B_SPLINE_CURVE_WITH_KNOTS('',3,(#41526,#41527,#41528,#41529,#41530,
#41531,#41532,#41533,#41534,#41535,#41536,#41537,#41538,#41539,#41540,#41541,
#41542,#41543,#41544,#41545,#41546,#41547,#41548,#41549,#41550,#41551,#41552,
#41553,#41554,#41555,#41556,#41557,#41558,#41559,#41560,#41561,#41562,#41563,
#41564,#41565,#41566,#41567,#41568,#41569,#41570,#41571,#41572,#41573,#41574,
#41575,#41576,#41577,#41578,#41579,#41580,#41581,#41582,#41583,#41584,#41585,
#41586),.UNSPECIFIED.,.F.,.F.,(4,3,3,3,3,3,3,3,3,3,3,3,3,3,3,3,3,3,3,3,
4),(5.47317109184868E-11,0.100716841584173,0.175358420792086,0.238665162138364,
0.25,0.301434484455404,0.351116096330567,0.400012858909411,0.450006429454706,
0.497458494136093,0.5,0.500001657323632,0.547542156254057,0.598156617190543,
0.647554747965031,0.698777373982516,0.75,0.812847460886534,0.887994716881443,
0.987407949822264,0.999999999957208),.UNSPECIFIED.);
#728=B_SPLINE_CURVE_WITH_KNOTS('',3,(#41627,#41628,#41629,#41630,#41631,
#41632,#41633,#41634,#41635,#41636,#41637,#41638,#41639,#41640,#41641,#41642,
#41643,#41644,#41645,#41646,#41647,#41648,#41649,#41650,#41651,#41652,#41653,
#41654,#41655,#41656,#41657,#41658,#41659,#41660,#41661,#41662,#41663,#41664,
#41665,#41666,#41667,#41668,#41669,#41670,#41671,#41672,#41673,#41674,#41675,
#41676,#41677,#41678,#41679,#41680,#41681,#41682,#41683,#41684,#41685,#41686,
#41687,#41688,#41689,#41690,#41691,#41692,#41693,#41694,#41695,#41696,#41697,
#41698,#41699,#41700,#41701,#41702,#41703,#41704,#41705,#41706,#41707,#41708,
#41709,#41710,#41711,#41712,#41713,#41714,#41715,#41716,#41717,#41718,#41719,
#41720,#41721,#41722,#41723,#41724,#41725,#41726,#41727,#41728,#41729,#41730,
#41731,#41732),.UNSPECIFIED.,.F.,.F.,(4,3,3,3,3,3,3,3,3,3,3,3,3,3,3,3,3,
3,3,3,3,3,3,3,3,3,3,3,3,3,3,3,3,3,3,4),(0.,0.053257050465951,0.105540886337049,
0.12396561413214,0.124999999999997,0.176282843367685,0.187499999999996,
0.218749999999995,0.234374999999995,0.242187499999994,0.246093749999994,
0.249704840463526,0.249999999999994,0.274255888483978,0.340144308274661,
0.404109232423276,0.426142645440888,0.490995077175135,0.499999999999994,
0.564437556258508,0.574120495681384,0.624999999999994,0.687499999999994,
0.718749999999994,0.726015446468681,0.734374999999994,0.742187499999994,
0.746093749999994,0.749746192108767,0.749999999999994,0.800189142872996,
0.851447051024866,0.876295161158848,0.929482782934934,0.983795496276306,
1.),.UNSPECIFIED.);
#729=B_SPLINE_CURVE_WITH_KNOTS('',3,(#41773,#41774,#41775,#41776,#41777,
#41778,#41779),.UNSPECIFIED.,.F.,.F.,(4,3,4),(0.,0.5,1.),.UNSPECIFIED.);
#730=B_SPLINE_CURVE_WITH_KNOTS('',3,(#41781,#41782,#41783,#41784,#41785,
#41786,#41787,#41788,#41789,#41790,#41791,#41792,#41793,#41794,#41795,#41796,
#41797,#41798,#41799,#41800,#41801,#41802,#41803,#41804,#41805,#41806,#41807,
#41808,#41809,#41810,#41811,#41812,#41813,#41814,#41815,#41816,#41817,#41818,
#41819,#41820),.UNSPECIFIED.,.F.,.F.,(4,3,3,3,3,3,3,3,3,3,3,3,3,4),(0.,
0.0902369168203611,0.118370167438031,0.25,0.36295411350154,0.4375,0.466154710754423,
0.495174404959947,0.499999999999999,0.615785132678318,0.717634497424337,
0.827090029722756,0.933176968893971,1.),.UNSPECIFIED.);
#731=B_SPLINE_CURVE_WITH_KNOTS('',3,(#41821,#41822,#41823,#41824,#41825,
#41826,#41827,#41828,#41829,#41830,#41831,#41832,#41833,#41834,#41835,#41836,
#41837,#41838,#41839,#41840,#41841,#41842,#41843,#41844,#41845,#41846,#41847,
#41848,#41849,#41850,#41851,#41852,#41853,#41854,#41855,#41856,#41857,#41858,
#41859,#41860,#41861,#41862,#41863,#41864,#41865,#41866,#41867,#41868,#41869,
#41870,#41871,#41872,#41873,#41874,#41875,#41876,#41877,#41878),
 .UNSPECIFIED.,.F.,.F.,(4,3,3,3,3,3,3,3,3,3,3,3,3,3,3,3,3,3,3,4),(0.,0.105589045184164,
0.149929520074555,0.249999999999981,0.345340162396845,0.370793467763536,
0.374999999999975,0.437499999999971,0.46874999999997,0.484374999999968,
0.494783657022549,0.499999999999967,0.589543647990068,0.60253603942224,
0.690095556674877,0.770652073013828,0.833509297677349,0.91080736609718,
0.983185422022552,1.),.UNSPECIFIED.);
#732=B_SPLINE_CURVE_WITH_KNOTS('',3,(#41924,#41925,#41926,#41927,#41928,
#41929,#41930,#41931,#41932,#41933,#41934,#41935,#41936,#41937,#41938,#41939,
#41940,#41941,#41942,#41943,#41944,#41945,#41946,#41947,#41948,#41949,#41950,
#41951,#41952,#41953,#41954,#41955,#41956,#41957,#41958,#41959,#41960,#41961,
#41962,#41963,#41964,#41965,#41966,#41967,#41968,#41969,#41970,#41971,#41972,
#41973,#41974,#41975,#41976,#41977,#41978,#41979,#41980,#41981,#41982,#41983,
#41984,#41985,#41986,#41987,#41988,#41989,#41990,#41991,#41992,#41993,#41994,
#41995,#41996),.UNSPECIFIED.,.F.,.F.,(4,3,3,3,3,3,3,3,3,3,3,3,3,3,3,3,3,
3,3,3,3,3,3,3,4),(0.,0.0458328892255905,0.0918178602187016,0.137727870872198,
0.1428571428571,0.148536598132459,0.203804992720327,0.259124754682715,0.2857142857143,
0.296137570174044,0.362354499372722,0.4285714285714,0.443717909280033,0.511006798196311,
0.5714285714286,0.591516277431717,0.658633939622798,0.7142857142857,0.739436741599132,
0.798289799371016,0.8571428571429,0.88721304215739,0.933524276536456,0.979590782851303,
1.),.UNSPECIFIED.);
#733=B_SPLINE_CURVE_WITH_KNOTS('',3,(#41999,#42000,#42001,#42002,#42003,
#42004,#42005,#42006,#42007,#42008,#42009,#42010,#42011,#42012,#42013,#42014,
#42015,#42016,#42017,#42018,#42019,#42020,#42021,#42022,#42023,#42024,#42025,
#42026,#42027,#42028,#42029,#42030,#42031,#42032,#42033,#42034,#42035,#42036,
#42037,#42038),.UNSPECIFIED.,.F.,.F.,(4,3,3,3,3,3,3,3,3,3,3,3,3,4),(0.,
0.132990604309484,0.153369582850421,0.28898480733553,0.306719319059886,
0.443622692112419,0.460361902236848,0.597256092732825,0.614811263154823,
0.75,0.769627679030996,0.909368696860574,0.924609571052109,0.999999999960875),
 .UNSPECIFIED.);
#734=B_SPLINE_CURVE_WITH_KNOTS('',3,(#42061,#42062,#42063,#42064,#42065,
#42066,#42067,#42068,#42069,#42070),.UNSPECIFIED.,.F.,.F.,(4,3,3,4),(0.,
0.3333333333333,0.6666666666667,1.),.UNSPECIFIED.);
#735=B_SPLINE_CURVE_WITH_KNOTS('',3,(#42206,#42207,#42208,#42209,#42210,
#42211,#42212,#42213,#42214,#42215,#42216,#42217,#42218,#42219,#42220,#42221,
#42222,#42223,#42224,#42225,#42226,#42227,#42228,#42229,#42230,#42231,#42232,
#42233,#42234,#42235,#42236,#42237,#42238,#42239,#42240,#42241,#42242,#42243,
#42244,#42245,#42246,#42247,#42248,#42249,#42250,#42251,#42252,#42253,#42254,
#42255,#42256,#42257,#42258,#42259,#42260,#42261,#42262,#42263,#42264,#42265,
#42266,#42267,#42268,#42269,#42270,#42271,#42272,#42273,#42274,#42275,#42276,
#42277,#42278,#42279,#42280,#42281,#42282,#42283,#42284,#42285,#42286,#42287,
#42288,#42289,#42290,#42291,#42292,#42293),.UNSPECIFIED.,.F.,.F.,(4,2,2,
1,2,2,2,1,1,1,2,2,2,2,1,1,1,2,2,2,2,2,2,2,2,2,1,2,2,2,1,1,2,2,2,2,1,1,2,
2,2,2,1,1,2,2,2,1,1,2,2,4),(0.,0.03125,0.046875,0.0546874999999999,0.0585937499999999,
0.0624999999999999,0.0937499999999991,0.109374999999999,0.117187499999998,
0.121093749999998,0.123046874999998,0.124999999999998,0.187499999999997,
0.218749999999997,0.234374999999997,0.242187499999997,0.246093749999997,
0.248046874999997,0.249999999999997,0.312500000000001,0.343750000000002,
0.359375000000003,0.375000000000004,0.437500000000007,0.468750000000008,
0.484375000000009,0.49218750000001,0.49609375000001,0.50000000000001,0.562500000000013,
0.593750000000014,0.609375000000015,0.617187500000016,0.625000000000016,
0.687500000000019,0.71875000000002,0.734375000000021,0.742187500000021,
0.746093750000021,0.750000000000021,0.812500000000022,0.843750000000022,
0.859375000000022,0.867187500000022,0.871093750000022,0.875000000000021,
0.906250000000017,0.921875000000014,0.929687500000013,0.933593750000012,
0.937500000000011,1.),.UNSPECIFIED.);
#736=B_SPLINE_CURVE_WITH_KNOTS('',3,(#42296,#42297,#42298,#42299,#42300,
#42301,#42302,#42303,#42304,#42305,#42306,#42307,#42308,#42309,#42310,#42311,
#42312,#42313,#42314,#42315,#42316,#42317,#42318,#42319,#42320,#42321,#42322,
#42323,#42324,#42325,#42326,#42327,#42328,#42329,#42330,#42331,#42332,#42333,
#42334,#42335,#42336,#42337,#42338,#42339,#42340,#42341,#42342,#42343,#42344,
#42345,#42346,#42347,#42348,#42349,#42350,#42351,#42352,#42353,#42354,#42355,
#42356,#42357,#42358,#42359,#42360,#42361,#42362,#42363,#42364,#42365,#42366,
#42367,#42368,#42369,#42370,#42371,#42372,#42373,#42374,#42375,#42376,#42377,
#42378,#42379,#42380,#42381,#42382,#42383,#42384,#42385,#42386,#42387,#42388,
#42389,#42390,#42391,#42392,#42393,#42394,#42395,#42396,#42397,#42398,#42399,
#42400,#42401,#42402,#42403,#42404,#42405,#42406,#42407,#42408,#42409,#42410,
#42411,#42412,#42413,#42414,#42415,#42416,#42417,#42418,#42419,#42420,#42421,
#42422,#42423,#42424,#42425,#42426,#42427,#42428,#42429,#42430,#42431,#42432,
#42433,#42434,#42435,#42436,#42437,#42438,#42439,#42440,#42441,#42442,#42443,
#42444,#42445,#42446,#42447,#42448,#42449,#42450,#42451,#42452,#42453,#42454,
#42455,#42456,#42457,#42458,#42459,#42460,#42461,#42462,#42463,#42464,#42465,
#42466,#42467,#42468,#42469,#42470,#42471,#42472,#42473,#42474,#42475,#42476,
#42477,#42478,#42479,#42480,#42481,#42482),.UNSPECIFIED.,.F.,.F.,(4,3,3,
3,3,3,3,3,3,3,3,3,3,3,3,3,3,3,3,3,3,3,3,3,3,3,3,3,3,3,3,3,3,3,3,3,3,3,3,
3,3,3,3,3,3,3,3,3,3,3,3,3,3,3,3,3,3,3,3,3,3,3,4),(7.50080231389504E-8,2.18347877829989E-7,
0.0229487004070204,0.0291148588785608,0.0509746146692638,0.0551851739629441,
0.0625000000000166,0.0795336635547587,0.100117921827564,0.102945846128966,
0.109375000000029,0.117187500000031,0.121093750000032,0.123046875000033,
0.124511718750033,0.125000000000033,0.126823712684557,0.154172414242767,
0.168540255145738,0.195094495105245,0.207813480733301,0.234375000000029,
0.243585926132158,0.24560283163885,0.250000000000028,0.286463023045781,
0.323179567483026,0.335377806100086,0.372218834583004,0.396057559740644,
0.433018802754509,0.46875000000002,0.47131279681658,0.484375000000019,0.492187500000019,
0.499324279379621,0.500000000000018,0.539362840686631,0.553194038309196,
0.592475975376577,0.619367181733849,0.658501763493894,0.673126718677383,
0.711992777641369,0.716725120819943,0.718750000000009,0.734375000000009,
0.742187500000009,0.746093750000008,0.749489103071601,0.750000000000008,
0.753695598866092,0.789783387614058,0.822481343688618,0.851891345405229,
0.87812104190446,0.901492399765885,0.922411241342964,0.941273136670307,
0.958424669511547,0.974021299622459,0.988170798160383,1.),.UNSPECIFIED.);
#737=B_SPLINE_CURVE_WITH_KNOTS('',3,(#42519,#42520,#42521,#42522,#42523,
#42524,#42525,#42526,#42527,#42528),.UNSPECIFIED.,.F.,.F.,(4,2,2,2,4),(2.2166076873242E-8,
0.25,0.5,0.75,1.),.UNSPECIFIED.);
#738=B_SPLINE_CURVE_WITH_KNOTS('',3,(#42529,#42530,#42531,#42532,#42533,
#42534,#42535,#42536,#42537,#42538,#42539,#42540,#42541,#42542,#42543,#42544,
#42545,#42546,#42547,#42548,#42549,#42550,#42551,#42552,#42553,#42554,#42555,
#42556,#42557,#42558,#42559,#42560,#42561,#42562,#42563,#42564,#42565,#42566,
#42567,#42568,#42569,#42570,#42571,#42572,#42573,#42574,#42575,#42576,#42577,
#42578,#42579,#42580,#42581,#42582,#42583,#42584,#42585,#42586,#42587,#42588,
#42589),.UNSPECIFIED.,.F.,.F.,(4,3,3,3,3,3,3,3,3,3,3,3,3,3,3,3,3,3,3,3,
4),(7.25467506948197E-11,0.100714571809277,0.175357285904639,0.238677150602764,
0.25,0.301434921986588,0.351121064526266,0.400024066781372,0.450012033390686,
0.497473671964868,0.5,0.500002027333907,0.547551851798238,0.598163888848679,
0.647567147211436,0.698783573605718,0.75,0.812861036075596,0.888030478108711,
0.987429614109391,0.999999999930326),.UNSPECIFIED.);
#739=B_SPLINE_CURVE_WITH_KNOTS('',3,(#42636,#42637,#42638,#42639,#42640,
#42641,#42642,#42643,#42644,#42645,#42646,#42647,#42648,#42649,#42650,#42651,
#42652,#42653,#42654,#42655,#42656,#42657,#42658,#42659,#42660,#42661,#42662,
#42663,#42664,#42665,#42666,#42667,#42668,#42669,#42670,#42671,#42672,#42673,
#42674,#42675,#42676,#42677,#42678,#42679,#42680,#42681,#42682,#42683,#42684,
#42685,#42686,#42687,#42688,#42689,#42690,#42691,#42692,#42693,#42694,#42695,
#42696,#42697,#42698,#42699,#42700,#42701,#42702,#42703,#42704,#42705,#42706,
#42707,#42708,#42709,#42710,#42711,#42712,#42713,#42714,#42715,#42716,#42717),
 .UNSPECIFIED.,.F.,.F.,(4,3,3,3,3,3,3,3,3,3,3,3,3,3,3,3,3,3,3,3,3,3,3,3,
3,3,3,4),(0.,0.0598753172964264,0.125,0.1875,0.208388761471869,0.21875,
0.234375,0.244077550301959,0.25,0.317441934267976,0.355226492165471,0.421839748974101,
0.488155247822196,0.499851881816781,0.499999999999999,0.564309740464253,
0.624999999999999,0.644482028662084,0.687499999999999,0.718749999999999,
0.734374999999999,0.744118095785684,0.749999999999999,0.791308742059749,
0.855329516807886,0.921469561084981,0.939826496901372,0.999999999999963),
 .UNSPECIFIED.);
#740=B_SPLINE_CURVE_WITH_KNOTS('',3,(#42756,#42757,#42758,#42759,#42760,
#42761,#42762,#42763,#42764,#42765,#42766,#42767,#42768,#42769,#42770,#42771,
#42772,#42773,#42774,#42775,#42776,#42777,#42778,#42779,#42780,#42781,#42782,
#42783,#42784,#42785,#42786,#42787,#42788,#42789,#42790,#42791,#42792,#42793,
#42794,#42795,#42796,#42797,#42798,#42799,#42800,#42801),.UNSPECIFIED.,
 .F.,.F.,(4,3,3,3,3,3,3,3,3,3,3,3,3,3,3,4),(0.,0.0770736690795171,0.11540458327814,
0.19659836676276,0.249999999999999,0.333146148439707,0.355774863218928,
0.374999999999999,0.422940018737277,0.471313219975339,0.499999999999999,
0.606506586343226,0.713013172686453,0.814528961412497,0.917302819950146,
1.),.UNSPECIFIED.);
#741=B_SPLINE_CURVE_WITH_KNOTS('',3,(#42802,#42803,#42804,#42805,#42806,
#42807,#42808),.UNSPECIFIED.,.F.,.F.,(4,3,4),(0.,0.5,0.999999975355396),
 .UNSPECIFIED.);
#742=B_SPLINE_CURVE_WITH_KNOTS('',3,(#42809,#42810,#42811,#42812,#42813,
#42814,#42815,#42816,#42817,#42818,#42819,#42820,#42821,#42822,#42823,#42824,
#42825,#42826,#42827,#42828,#42829,#42830,#42831,#42832,#42833,#42834,#42835,
#42836,#42837,#42838,#42839,#42840,#42841,#42842,#42843,#42844,#42845,#42846,
#42847,#42848,#42849,#42850,#42851,#42852,#42853,#42854,#42855,#42856,#42857,
#42858,#42859,#42860,#42861,#42862,#42863,#42864,#42865,#42866),
 .UNSPECIFIED.,.F.,.F.,(4,3,3,3,3,3,3,3,3,3,3,3,3,3,3,3,3,3,3,4),(0.,0.0715177076076025,
0.147781603164113,0.168373690108482,0.25000000000002,0.334962898290653,
0.375000000000031,0.400046415107386,0.437500000000033,0.468750000000035,
0.484375000000036,0.495337496274554,0.500000000000038,0.593386942558541,
0.631716791369734,0.726860228272911,0.828107710230089,0.852770844187471,
0.958441713256798,1.),.UNSPECIFIED.);
#743=B_SPLINE_CURVE_WITH_KNOTS('',3,(#42909,#42910,#42911,#42912,#42913,
#42914,#42915,#42916,#42917,#42918,#42919,#42920,#42921,#42922,#42923,#42924,
#42925,#42926,#42927,#42928,#42929,#42930),.UNSPECIFIED.,.F.,.F.,(4,3,3,
3,3,3,3,4),(1.01038589610438E-7,0.1428571428571,0.2857142857143,0.4285714285714,
0.5714285714286,0.7142857142857,0.8571428571429,1.),.UNSPECIFIED.);
#744=B_SPLINE_CURVE_WITH_KNOTS('',3,(#42973,#42974,#42975,#42976,#42977,
#42978,#42979),.UNSPECIFIED.,.F.,.F.,(4,3,4),(2.15062665969218E-8,0.5,0.999999999974515),
 .UNSPECIFIED.);
#745=B_SPLINE_CURVE_WITH_KNOTS('',3,(#42981,#42982,#42983,#42984,#42985,
#42986,#42987,#42988,#42989,#42990,#42991,#42992,#42993,#42994,#42995,#42996,
#42997,#42998,#42999,#43000,#43001,#43002,#43003,#43004,#43005,#43006,#43007,
#43008,#43009,#43010,#43011,#43012,#43013,#43014,#43015,#43016,#43017,#43018,
#43019,#43020,#43021,#43022,#43023),.UNSPECIFIED.,.F.,.F.,(4,3,3,3,3,3,
3,3,3,3,3,3,3,3,4),(0.,0.0900140533241843,0.116403794824626,0.243031863324909,
0.250000000000001,0.360150451046764,0.437499999999997,0.466162821938923,
0.495190581692203,0.499999999999996,0.615787326593693,0.712807369725428,
0.822401125042849,0.928574641518961,1.),.UNSPECIFIED.);
#746=B_SPLINE_CURVE_WITH_KNOTS('',3,(#43024,#43025,#43026,#43027,#43028,
#43029,#43030,#43031,#43032,#43033,#43034,#43035,#43036,#43037,#43038,#43039,
#43040,#43041,#43042,#43043,#43044,#43045,#43046,#43047,#43048,#43049,#43050,
#43051,#43052,#43053,#43054,#43055,#43056,#43057,#43058,#43059,#43060,#43061,
#43062,#43063,#43064,#43065,#43066,#43067,#43068,#43069,#43070,#43071,#43072,
#43073,#43074,#43075,#43076,#43077,#43078,#43079,#43080,#43081),
 .UNSPECIFIED.,.F.,.F.,(4,3,3,3,3,3,3,3,3,3,3,3,3,3,3,3,3,3,3,4),(0.,0.105620942331472,
0.147712756907025,0.250000000000027,0.345332762315205,0.368665277226416,
0.375000000000042,0.437500000000047,0.468750000000048,0.484375000000051,
0.49473518058623,0.500000000000054,0.589017367505976,0.600284370952884,
0.686110190968832,0.750000000000027,0.831760796016761,0.908457339360646,
0.980208828865569,1.),.UNSPECIFIED.);
#747=B_SPLINE_CURVE_WITH_KNOTS('',3,(#43123,#43124,#43125,#43126,#43127,
#43128,#43129,#43130,#43131,#43132,#43133,#43134,#43135,#43136,#43137,#43138,
#43139,#43140,#43141,#43142,#43143,#43144),.UNSPECIFIED.,.F.,.F.,(4,3,3,
3,3,3,3,4),(0.,0.1428571428571,0.2857142857143,0.4285714285714,0.5714285714286,
0.7142857142857,0.8571428571429,0.99999989893428),.UNSPECIFIED.);
#748=B_SPLINE_CURVE_WITH_KNOTS('',3,(#43147,#43148,#43149,#43150,#43151,
#43152,#43153,#43154,#43155,#43156),.UNSPECIFIED.,.F.,.F.,(4,2,2,2,4),(0.,
0.25,0.5,0.75,0.999999977827856),.UNSPECIFIED.);
#749=B_SPLINE_CURVE_WITH_KNOTS('',3,(#43186,#43187,#43188,#43189,#43190,
#43191,#43192,#43193,#43194,#43195,#43196,#43197,#43198),.UNSPECIFIED.,
 .F.,.F.,(4,3,3,3,4),(0.,0.0431918505797328,0.5,0.956806409420606,1.),
 .UNSPECIFIED.);
#750=B_SPLINE_CURVE_WITH_KNOTS('',3,(#43219,#43220,#43221,#43222,#43223,
#43224,#43225,#43226,#43227,#43228,#43229,#43230,#43231,#43232,#43233,#43234,
#43235,#43236,#43237,#43238,#43239,#43240,#43241,#43242,#43243,#43244,#43245,
#43246,#43247,#43248,#43249,#43250,#43251,#43252,#43253,#43254,#43255,#43256,
#43257,#43258,#43259,#43260,#43261,#43262,#43263,#43264,#43265,#43266,#43267,
#43268,#43269,#43270,#43271,#43272,#43273,#43274,#43275,#43276,#43277,#43278,
#43279,#43280,#43281,#43282,#43283,#43284,#43285,#43286,#43287,#43288,#43289,
#43290,#43291,#43292,#43293,#43294,#43295,#43296,#43297,#43298,#43299,#43300,
#43301,#43302,#43303,#43304,#43305,#43306,#43307,#43308,#43309,#43310,#43311,
#43312,#43313,#43314,#43315,#43316,#43317,#43318,#43319,#43320,#43321,#43322,
#43323,#43324,#43325,#43326,#43327,#43328,#43329,#43330,#43331,#43332,#43333,
#43334,#43335,#43336,#43337,#43338,#43339,#43340,#43341,#43342,#43343,#43344,
#43345,#43346,#43347,#43348,#43349,#43350,#43351,#43352,#43353,#43354,#43355,
#43356,#43357,#43358,#43359,#43360,#43361,#43362,#43363,#43364,#43365,#43366,
#43367,#43368,#43369,#43370,#43371,#43372,#43373,#43374,#43375,#43376,#43377,
#43378,#43379,#43380,#43381,#43382,#43383,#43384,#43385,#43386,#43387,#43388,
#43389,#43390,#43391,#43392,#43393,#43394,#43395,#43396,#43397,#43398,#43399,
#43400,#43401,#43402,#43403,#43404,#43405,#43406,#43407,#43408,#43409,#43410,
#43411,#43412,#43413,#43414,#43415,#43416,#43417,#43418,#43419,#43420,#43421,
#43422,#43423),.UNSPECIFIED.,.F.,.F.,(4,3,3,3,3,3,3,3,3,3,3,3,3,3,3,3,3,
3,3,3,3,3,3,3,3,3,3,3,3,3,3,3,3,3,3,3,3,3,3,3,3,3,3,3,3,3,3,3,3,3,3,3,3,
3,3,3,3,3,3,3,3,3,3,3,3,3,3,3,4),(0.,0.02498566546768,0.049884025399438,
0.0680623311189957,0.0924414494617866,0.107887461956563,0.131551576955674,
0.140980478002927,0.163943871857324,0.171020780322756,0.193322633875285,
0.199590323256334,0.218750000000002,0.227568744214109,0.234375000000002,
0.242187500000002,0.246093750000002,0.248046875000002,0.249023437500002,
0.250000000000002,0.254546871473152,0.279971649656408,0.307406578415395,
0.309430130689131,0.337127106350482,0.344163692255729,0.37200152680762,
0.384912473573474,0.412566459342994,0.429839311238586,0.457842489942603,
0.46874999999999,0.477238857091961,0.484374999999989,0.492187499999988,
0.496093749999988,0.498046874999988,0.499999999999988,0.531289746912242,
0.56564199746469,0.578505777121612,0.613121656810267,0.616394754523827,
0.648093063112125,0.674914456580065,0.697975732163873,0.718059303584619,
0.718749999999981,0.73437499999998,0.735681902185849,0.74218749999998,0.74609374999998,
0.748046874999979,0.749023437499979,0.749999999999979,0.751844076693351,
0.773859225168292,0.79513825511006,0.815771716334843,0.835876984948117,
0.855607588286063,0.87499999999999,0.875168000986653,0.894779928887882,
0.914590308239194,0.934773415781677,0.955588220120383,0.977473296500908,
0.999999988534214),.UNSPECIFIED.);
#751=B_SPLINE_CURVE_WITH_KNOTS('',3,(#43586,#43587,#43588,#43589,#43590,
#43591,#43592,#43593,#43594,#43595,#43596,#43597,#43598,#43599,#43600,#43601,
#43602,#43603,#43604,#43605,#43606,#43607,#43608,#43609,#43610,#43611,#43612,
#43613,#43614,#43615,#43616,#43617,#43618,#43619,#43620,#43621,#43622,#43623,
#43624,#43625,#43626,#43627,#43628,#43629,#43630,#43631,#43632,#43633,#43634,
#43635,#43636,#43637,#43638,#43639,#43640,#43641,#43642,#43643,#43644,#43645,
#43646,#43647,#43648,#43649,#43650,#43651,#43652,#43653,#43654,#43655,#43656,
#43657,#43658,#43659,#43660,#43661,#43662,#43663,#43664,#43665,#43666,#43667,
#43668,#43669,#43670,#43671,#43672,#43673,#43674,#43675,#43676,#43677,#43678,
#43679,#43680,#43681,#43682,#43683,#43684,#43685,#43686,#43687,#43688,#43689,
#43690,#43691,#43692,#43693,#43694,#43695,#43696,#43697,#43698,#43699,#43700,
#43701,#43702,#43703,#43704,#43705,#43706),.UNSPECIFIED.,.F.,.F.,(4,3,3,
3,3,3,3,3,3,3,3,3,3,3,3,3,3,3,3,3,3,3,3,3,3,3,3,3,3,3,3,3,3,3,3,3,3,3,3,
3,4),(7.98332310068083E-8,0.0312500598749252,0.0618422367860364,0.0934211183930221,
0.125000000000008,0.155569261434962,0.187159630717487,0.218750000000013,
0.234375000000014,0.242187500000015,0.246093750000015,0.248046875000015,
0.249023437500015,0.250000000000015,0.450324982651065,0.49998131820124,
0.500000000000021,0.625000000000023,0.687500000000025,0.718750000000025,
0.734375000000026,0.742187500000026,0.749511718750026,0.750000000000026,
0.765919055600215,0.781838289527891,0.797757711899691,0.813677446196644,
0.829597360333286,0.845517577762525,0.859375000000007,0.867187500000006,
0.871093750000005,0.873046875000005,0.874023437500005,0.875000000000005,
0.899836811730506,0.924877595078578,0.949727823226582,0.974863884174689,
0.999999945122795),.UNSPECIFIED.);
#752=B_SPLINE_CURVE_WITH_KNOTS('',3,(#43747,#43748,#43749,#43750,#43751,
#43752,#43753,#43754,#43755,#43756,#43757,#43758,#43759,#43760,#43761,#43762,
#43763,#43764,#43765,#43766,#43767,#43768,#43769,#43770,#43771,#43772,#43773,
#43774,#43775,#43776,#43777,#43778,#43779,#43780,#43781,#43782,#43783,#43784,
#43785,#43786,#43787,#43788,#43789,#43790,#43791,#43792,#43793,#43794,#43795),
 .UNSPECIFIED.,.F.,.F.,(4,3,3,3,3,3,3,3,3,3,3,3,3,3,3,3,4),(0.,0.077129221718004,
0.118225031062465,0.199429752236532,0.249999999999997,0.333192781133113,
0.359721388485999,0.374999999999996,0.423000321495183,0.471434965050803,
0.499999999999995,0.602025518392161,0.703466763159088,0.719210551366323,
0.820753809715136,0.923562015178621,1.),.UNSPECIFIED.);
#753=B_SPLINE_CURVE_WITH_KNOTS('',3,(#43797,#43798,#43799,#43800,#43801,
#43802,#43803),.UNSPECIFIED.,.F.,.F.,(4,3,4),(0.,0.5,1.),.UNSPECIFIED.);
#754=B_SPLINE_CURVE_WITH_KNOTS('',3,(#43806,#43807,#43808,#43809,#43810,
#43811,#43812,#43813,#43814,#43815,#43816,#43817,#43818,#43819,#43820,#43821,
#43822,#43823,#43824,#43825,#43826,#43827,#43828,#43829,#43830,#43831,#43832,
#43833,#43834,#43835,#43836,#43837,#43838,#43839,#43840,#43841,#43842,#43843,
#43844,#43845,#43846,#43847,#43848,#43849,#43850,#43851,#43852,#43853,#43854,
#43855,#43856,#43857,#43858,#43859,#43860,#43861,#43862,#43863,#43864,#43865,
#43866),.UNSPECIFIED.,.F.,.F.,(4,3,3,3,3,3,3,3,3,3,3,3,3,3,3,3,3,3,3,3,
4),(0.,0.0723227135726931,0.149373482450991,0.166421265554989,0.245216450281879,
0.24999999999999,0.335716326463502,0.374999999999983,0.397180535434601,
0.437499999999978,0.468749999999973,0.484374999999972,0.495375835992438,
0.499999999999971,0.593362825587567,0.628795107419847,0.723805225870199,
0.824915532107725,0.849552878717866,0.955120156071517,1.),.UNSPECIFIED.);
#755=B_SPLINE_CURVE_WITH_KNOTS('',3,(#43907,#43908,#43909,#43910,#43911,
#43912,#43913,#43914,#43915,#43916,#43917,#43918,#43919,#43920,#43921,#43922,
#43923,#43924,#43925,#43926,#43927,#43928,#43929,#43930,#43931,#43932,#43933,
#43934,#43935,#43936,#43937,#43938,#43939,#43940,#43941,#43942,#43943,#43944,
#43945,#43946,#43947,#43948,#43949),.UNSPECIFIED.,.F.,.F.,(4,3,3,3,3,3,
3,3,3,3,3,3,3,3,4),(2.99160140262836E-11,0.0832138083944097,0.218577885005784,
0.246109287452998,0.25,0.383459487824275,0.408370299553468,0.541180659138591,
0.570056216035696,0.702294213347345,0.731364949289518,0.75,0.881938327221045,
0.892442289727949,0.999999987394256),.UNSPECIFIED.);
#756=B_SPLINE_CURVE_WITH_KNOTS('',3,(#43950,#43951,#43952,#43953,#43954,
#43955,#43956,#43957,#43958,#43959,#43960,#43961,#43962,#43963,#43964,#43965,
#43966,#43967,#43968,#43969,#43970,#43971,#43972,#43973,#43974,#43975,#43976,
#43977,#43978,#43979,#43980,#43981,#43982,#43983,#43984,#43985,#43986,#43987,
#43988,#43989,#43990,#43991,#43992,#43993,#43994,#43995,#43996,#43997,#43998,
#43999,#44000,#44001,#44002,#44003,#44004,#44005,#44006,#44007,#44008,#44009,
#44010,#44011,#44012,#44013,#44014,#44015,#44016,#44017,#44018,#44019,#44020,
#44021,#44022,#44023,#44024,#44025,#44026,#44027,#44028),.UNSPECIFIED.,
 .F.,.F.,(4,3,3,3,3,3,3,3,3,3,3,3,3,3,3,3,3,3,3,3,3,3,3,3,3,3,4),(0.,0.0457810663232214,
0.0917889142262468,0.120317290917319,0.1428571428571,0.198222944211764,
0.253550325370331,0.275526256355539,0.2857142857143,0.349641048789147,0.413645189435696,
0.4285714285714,0.430597609456793,0.49617632407596,0.561795552657668,0.5714285714286,
0.585374526668123,0.649830120476911,0.7142857142857,0.7403962732342,0.795252877501319,
0.850177989897438,0.8571428571429,0.895765393025997,0.941863426709497,0.987754574459855,
0.999999797061878),.UNSPECIFIED.);
#757=B_SPLINE_CURVE_WITH_KNOTS('',3,(#44064,#44065,#44066,#44067,#44068,
#44069,#44070,#44071,#44072,#44073,#44074,#44075,#44076,#44077,#44078,#44079,
#44080,#44081,#44082,#44083,#44084,#44085,#44086,#44087,#44088,#44089,#44090,
#44091,#44092,#44093,#44094,#44095,#44096,#44097,#44098,#44099,#44100,#44101,
#44102,#44103,#44104,#44105,#44106,#44107,#44108,#44109,#44110,#44111,#44112,
#44113,#44114,#44115,#44116,#44117,#44118,#44119,#44120,#44121,#44122,#44123,
#44124),.UNSPECIFIED.,.F.,.F.,(4,3,3,3,3,3,3,3,3,3,3,3,3,3,3,3,3,3,3,3,
4),(5.51331975023469E-11,0.100729568242541,0.175364784121271,0.238681770721503,
0.25,0.301425913559992,0.351100073817221,0.399989929903429,0.449994964951714,
0.497440910286256,0.5,0.500001662220487,0.54753591343043,0.598151935072823,
0.647542568098908,0.698771284049454,0.75,0.812858492196759,0.888031547366612,
0.98742976017277,0.99999999994457),.UNSPECIFIED.);
#758=B_SPLINE_CURVE_WITH_KNOTS('',3,(#44165,#44166,#44167,#44168,#44169,
#44170,#44171,#44172,#44173,#44174,#44175,#44176,#44177,#44178,#44179,#44180,
#44181,#44182,#44183,#44184,#44185,#44186,#44187,#44188,#44189,#44190,#44191,
#44192,#44193,#44194,#44195,#44196,#44197,#44198,#44199,#44200,#44201,#44202,
#44203,#44204,#44205,#44206,#44207,#44208,#44209,#44210,#44211,#44212,#44213,
#44214,#44215,#44216,#44217,#44218,#44219,#44220,#44221,#44222,#44223,#44224,
#44225,#44226,#44227,#44228,#44229,#44230,#44231,#44232,#44233,#44234,#44235,
#44236,#44237,#44238,#44239,#44240,#44241,#44242,#44243,#44244,#44245,#44246,
#44247,#44248,#44249,#44250,#44251,#44252,#44253,#44254,#44255,#44256,#44257,
#44258),.UNSPECIFIED.,.F.,.F.,(4,3,3,3,3,3,3,3,3,3,3,3,3,3,3,3,3,3,3,3,
3,3,3,3,3,3,3,3,3,3,3,4),(0.,0.0608427785031114,0.121685557006223,0.125000000000001,
0.182031019624917,0.187500000000002,0.218750000000002,0.234375000000003,
0.242187500000002,0.247942132015918,0.250000000000002,0.273617827471563,
0.341050580590077,0.407249199298602,0.425682324109709,0.492217475541122,
0.500000000000002,0.565400091710283,0.574576838490885,0.625000000000001,
0.687500000000001,0.718750000000001,0.726647659500348,0.734375000000001,
0.742187500000001,0.747984593859013,0.750000000000001,0.805925774071174,
0.863236880411379,0.878574885619189,0.939287442809595,1.),.UNSPECIFIED.);
#759=B_SPLINE_CURVE_WITH_KNOTS('',3,(#44299,#44300,#44301,#44302,#44303,
#44304,#44305),.UNSPECIFIED.,.F.,.F.,(4,3,4),(0.,0.5,0.999999999992773),
 .UNSPECIFIED.);
#760=B_SPLINE_CURVE_WITH_KNOTS('',3,(#44307,#44308,#44309,#44310,#44311,
#44312,#44313,#44314,#44315,#44316,#44317,#44318,#44319,#44320,#44321,#44322,
#44323,#44324,#44325,#44326,#44327,#44328,#44329,#44330,#44331,#44332,#44333,
#44334,#44335,#44336,#44337,#44338,#44339,#44340,#44341,#44342,#44343,#44344,
#44345,#44346,#44347,#44348,#44349),.UNSPECIFIED.,.F.,.F.,(4,3,3,3,3,3,
3,3,3,3,3,3,3,3,4),(0.,0.0899680658841344,0.116138968898349,0.242390930404426,
0.25000000000001,0.363401837080852,0.437500000000014,0.466169905219584,
0.495204599768524,0.500000000000013,0.615774222962765,0.721520585496806,
0.830869548090939,0.936889486863146,1.),.UNSPECIFIED.);
#761=B_SPLINE_CURVE_WITH_KNOTS('',3,(#44350,#44351,#44352,#44353,#44354,
#44355,#44356,#44357,#44358,#44359,#44360,#44361,#44362,#44363,#44364,#44365,
#44366,#44367,#44368,#44369,#44370,#44371,#44372,#44373,#44374,#44375,#44376,
#44377,#44378,#44379,#44380,#44381,#44382,#44383,#44384,#44385,#44386,#44387,
#44388,#44389,#44390,#44391,#44392,#44393,#44394,#44395,#44396,#44397,#44398,
#44399,#44400,#44401,#44402,#44403,#44404,#44405,#44406,#44407),
 .UNSPECIFIED.,.F.,.F.,(4,3,3,3,3,3,3,3,3,3,3,3,3,3,3,3,3,3,3,4),(0.,0.104831354904759,
0.146359487096874,0.25000000000003,0.344476853378971,0.368351209780046,
0.375000000000043,0.43750000000005,0.468750000000052,0.484375000000053,
0.49465917516026,0.500000000000053,0.58999972691812,0.600572762837569,0.688690709817914,
0.769751602688375,0.832826399321062,0.910573005906539,0.983365812451633,
1.),.UNSPECIFIED.);
#762=B_SPLINE_CURVE_WITH_KNOTS('',3,(#44453,#44454,#44455,#44456,#44457,
#44458,#44459,#44460,#44461,#44462,#44463,#44464,#44465,#44466,#44467,#44468,
#44469,#44470,#44471,#44472,#44473,#44474,#44475,#44476,#44477,#44478,#44479,
#44480,#44481,#44482,#44483,#44484,#44485,#44486,#44487,#44488,#44489,#44490,
#44491,#44492,#44493,#44494,#44495,#44496,#44497,#44498,#44499,#44500,#44501,
#44502,#44503,#44504,#44505,#44506,#44507,#44508,#44509,#44510,#44511,#44512,
#44513,#44514,#44515,#44516,#44517,#44518,#44519,#44520,#44521,#44522,#44523,
#44524,#44525),.UNSPECIFIED.,.F.,.F.,(4,3,3,3,3,3,3,3,3,3,3,3,3,3,3,3,3,
3,3,3,3,3,3,3,4),(0.,0.0458328812420613,0.0918178429902138,0.137727842668992,
0.1428571428571,0.148537109984561,0.203805441054238,0.259125141492703,0.2857142857143,
0.296138265592348,0.362354847081874,0.4285714285714,0.443718112661787,0.511007039375829,
0.5714285714286,0.591515929737013,0.658633627441551,0.7142857142857,0.739436118157717,
0.798289487650309,0.8571428571429,0.887212493478405,0.933523714257452,0.979590210065679,
1.),.UNSPECIFIED.);
#763=B_SPLINE_CURVE_WITH_KNOTS('',3,(#44528,#44529,#44530,#44531,#44532,
#44533,#44534,#44535,#44536,#44537,#44538,#44539,#44540,#44541,#44542,#44543,
#44544,#44545,#44546,#44547,#44548,#44549,#44550,#44551,#44552,#44553,#44554,
#44555,#44556,#44557,#44558,#44559,#44560,#44561,#44562,#44563,#44564,#44565,
#44566,#44567),.UNSPECIFIED.,.F.,.F.,(4,3,3,3,3,3,3,3,3,3,3,3,3,4),(0.,
0.132990593304601,0.153370100778055,0.288985327651276,0.306720031714283,
0.443623442712682,0.460362108909032,0.597256308685064,0.614810898821594,
0.75,0.769627028952669,0.909362273050122,0.924609010238514,0.999999999982405),
 .UNSPECIFIED.);
#764=B_SPLINE_CURVE_WITH_KNOTS('',3,(#44590,#44591,#44592,#44593,#44594,
#44595,#44596,#44597,#44598,#44599),.UNSPECIFIED.,.F.,.F.,(4,3,3,4),(0.,
0.3333333333333,0.6666666666667,1.),.UNSPECIFIED.);
#765=B_SPLINE_CURVE_WITH_KNOTS('',3,(#44735,#44736,#44737,#44738,#44739,
#44740,#44741,#44742,#44743,#44744,#44745,#44746,#44747,#44748,#44749,#44750,
#44751,#44752,#44753,#44754,#44755,#44756,#44757,#44758,#44759,#44760,#44761,
#44762,#44763,#44764,#44765,#44766,#44767,#44768,#44769,#44770,#44771,#44772,
#44773,#44774,#44775,#44776,#44777,#44778,#44779,#44780,#44781,#44782,#44783,
#44784,#44785,#44786,#44787,#44788,#44789,#44790,#44791,#44792,#44793,#44794,
#44795,#44796,#44797,#44798,#44799,#44800,#44801,#44802,#44803,#44804,#44805,
#44806,#44807,#44808,#44809,#44810,#44811,#44812,#44813,#44814,#44815,#44816,
#44817,#44818,#44819,#44820,#44821,#44822,#44823),.UNSPECIFIED.,.F.,.F.,
(4,2,2,1,2,2,2,2,1,1,2,2,2,2,1,1,1,2,2,2,2,2,2,2,2,2,1,2,2,2,1,1,2,2,2,
2,1,1,2,2,2,2,1,1,2,2,2,1,1,2,2,4),(0.,0.0312499999999994,0.046874999999999,
0.0546874999999987,0.0585937499999986,0.0624999999999985,0.0937499999999971,
0.109374999999996,0.117187499999996,0.121093749999996,0.123046874999996,
0.124999999999996,0.187499999999999,0.21875,0.234375000000001,0.242187500000001,
0.246093750000002,0.248046875000002,0.250000000000002,0.312500000000002,
0.343750000000003,0.359375000000003,0.375000000000003,0.437500000000004,
0.468750000000004,0.484375000000004,0.492187500000004,0.496093750000004,
0.500000000000004,0.562500000000005,0.593750000000005,0.609375000000005,
0.617187500000005,0.625000000000005,0.687500000000005,0.718750000000005,
0.734375000000005,0.742187500000005,0.746093750000005,0.750000000000005,
0.812500000000005,0.843750000000006,0.859375000000005,0.867187500000005,
0.871093750000005,0.875000000000005,0.906250000000004,0.921875000000003,
0.929687500000003,0.933593750000003,0.937500000000003,1.),.UNSPECIFIED.);
#766=B_SPLINE_CURVE_WITH_KNOTS('',3,(#44826,#44827,#44828,#44829,#44830,
#44831,#44832,#44833,#44834,#44835,#44836,#44837,#44838,#44839,#44840,#44841,
#44842,#44843,#44844,#44845,#44846,#44847,#44848,#44849,#44850,#44851,#44852,
#44853,#44854,#44855,#44856,#44857,#44858,#44859,#44860,#44861,#44862,#44863,
#44864,#44865,#44866,#44867,#44868,#44869,#44870,#44871,#44872,#44873,#44874,
#44875,#44876,#44877,#44878,#44879,#44880,#44881,#44882,#44883,#44884,#44885,
#44886,#44887,#44888,#44889,#44890,#44891,#44892,#44893,#44894,#44895,#44896,
#44897,#44898,#44899,#44900,#44901,#44902,#44903,#44904,#44905,#44906,#44907,
#44908,#44909,#44910,#44911,#44912,#44913,#44914,#44915,#44916,#44917,#44918,
#44919,#44920,#44921,#44922,#44923,#44924,#44925,#44926,#44927,#44928,#44929,
#44930,#44931,#44932,#44933,#44934,#44935,#44936,#44937,#44938,#44939,#44940,
#44941,#44942,#44943,#44944,#44945,#44946,#44947,#44948,#44949,#44950,#44951,
#44952,#44953,#44954,#44955,#44956,#44957,#44958,#44959,#44960,#44961,#44962,
#44963,#44964,#44965,#44966,#44967,#44968,#44969,#44970,#44971,#44972,#44973,
#44974,#44975,#44976,#44977,#44978,#44979,#44980,#44981,#44982,#44983,#44984,
#44985,#44986,#44987,#44988,#44989,#44990,#44991,#44992,#44993,#44994,#44995,
#44996,#44997,#44998,#44999,#45000,#45001,#45002,#45003,#45004,#45005,#45006,
#45007,#45008,#45009,#45010,#45011,#45012),.UNSPECIFIED.,.F.,.F.,(4,3,3,
3,3,3,3,3,3,3,3,3,3,3,3,3,3,3,3,3,3,3,3,3,3,3,3,3,3,3,3,3,3,3,3,3,3,3,3,
3,3,3,3,3,3,3,3,3,3,3,3,3,3,3,3,3,3,3,3,3,3,3,4),(7.50077744408458E-8,2.18347065731793E-7,
0.0229486992448132,0.0291148599209922,0.0509746147885199,0.0551851751703622,
0.0624999999999753,0.0795336645402833,0.100117921833713,0.102945846679325,
0.109374999999957,0.117187499999954,0.121093749999952,0.123046874999952,
0.124511718749951,0.124999999999951,0.126823713026409,0.154172407482107,
0.168540259620717,0.195094492624172,0.207813484550183,0.234374999999958,
0.243585913496471,0.245602831811104,0.249999999999959,0.286463024092484,
0.32317957057371,0.335377808175913,0.372218838783674,0.396057562301687,
0.433018807503827,0.468749999999972,0.471312798122102,0.484374999999973,
0.492187499999974,0.499324281709741,0.499999999999974,0.539362839729169,
0.553194039019897,0.592475975164342,0.619367182653107,0.65850176352843,
0.673126719387982,0.711992777523277,0.716725121178675,0.718749999999988,
0.734374999999989,0.742187499999989,0.746093749999989,0.749489102970321,
0.74999999999999,0.753695598868588,0.789783387615562,0.822481343689209,
0.851891345405311,0.878121041904186,0.90149239976546,0.922411241342462,
0.941273136669776,0.958424669511218,0.974021299622255,0.988170798160314,
1.),.UNSPECIFIED.);
#767=B_SPLINE_CURVE_WITH_KNOTS('',3,(#45049,#45050,#45051,#45052,#45053,
#45054,#45055,#45056,#45057,#45058),.UNSPECIFIED.,.F.,.F.,(4,2,2,2,4),(2.21660018633822E-8,
0.25,0.5,0.75,1.),.UNSPECIFIED.);
#768=B_SPLINE_CURVE_WITH_KNOTS('',3,(#45059,#45060,#45061,#45062,#45063,
#45064,#45065,#45066,#45067,#45068,#45069,#45070,#45071,#45072,#45073,#45074,
#45075,#45076,#45077,#45078,#45079,#45080,#45081,#45082,#45083,#45084,#45085,
#45086,#45087,#45088,#45089,#45090,#45091,#45092,#45093,#45094,#45095,#45096,
#45097,#45098,#45099,#45100,#45101,#45102,#45103,#45104,#45105,#45106,#45107,
#45108,#45109,#45110,#45111,#45112,#45113,#45114,#45115,#45116,#45117,#45118,
#45119),.UNSPECIFIED.,.F.,.F.,(4,3,3,3,3,3,3,3,3,3,3,3,3,3,3,3,3,3,3,3,
4),(3.71092975531932E-11,0.10075796569964,0.17537898284982,0.238719107558443,
0.25,0.301412310165757,0.351074976513478,0.399954340676608,0.449977170338304,
0.497414131176893,0.5,0.50000257236142,0.547527734549922,0.598145800912442,
0.647524947458811,0.698762473729406,0.75,0.812880663949358,0.888102663575457,
0.987477736473804,0.99999999995342),.UNSPECIFIED.);
#769=B_SPLINE_CURVE_WITH_KNOTS('',3,(#45162,#45163,#45164,#45165,#45166,
#45167,#45168,#45169,#45170,#45171,#45172,#45173,#45174,#45175,#45176,#45177,
#45178,#45179,#45180,#45181,#45182,#45183,#45184,#45185,#45186,#45187,#45188,
#45189,#45190,#45191,#45192,#45193,#45194,#45195,#45196,#45197,#45198,#45199,
#45200,#45201,#45202,#45203,#45204,#45205,#45206,#45207,#45208,#45209,#45210,
#45211,#45212,#45213,#45214,#45215,#45216,#45217,#45218,#45219,#45220,#45221,
#45222,#45223,#45224,#45225,#45226,#45227,#45228,#45229,#45230,#45231,#45232,
#45233,#45234,#45235,#45236,#45237,#45238,#45239,#45240,#45241,#45242,#45243,
#45244,#45245,#45246,#45247,#45248,#45249),.UNSPECIFIED.,.F.,.F.,(4,3,3,
3,3,3,3,3,3,3,3,3,3,3,3,3,3,3,3,3,3,3,3,3,3,3,3,3,3,4),(0.,0.0590919852588188,
0.11700786268473,0.124999999999999,0.131471991461492,0.187499999999999,
0.218749999999999,0.234374999999998,0.243548805830801,0.249999999999998,
0.280266149608354,0.347497113067735,0.413420413834471,0.427679421923862,
0.494017799351283,0.499999999999998,0.564689257159006,0.571457994333151,
0.624999999999998,0.687499999999998,0.718749999999998,0.718850415436541,
0.734374999999998,0.743575440506396,0.749999999999998,0.808807839857273,
0.867615679714548,0.926690041742276,0.987210740295307,1.),.UNSPECIFIED.);
#770=B_SPLINE_CURVE_WITH_KNOTS('',3,(#45288,#45289,#45290,#45291,#45292,
#45293,#45294,#45295,#45296,#45297,#45298,#45299,#45300,#45301,#45302,#45303,
#45304,#45305,#45306,#45307,#45308,#45309,#45310,#45311,#45312,#45313,#45314,
#45315,#45316,#45317,#45318,#45319,#45320,#45321,#45322,#45323,#45324,#45325,
#45326,#45327,#45328,#45329,#45330,#45331,#45332,#45333,#45334,#45335,#45336),
 .UNSPECIFIED.,.F.,.F.,(4,3,3,3,3,3,3,3,3,3,3,3,3,3,3,3,4),(0.,0.0770534094112941,
0.113178684151245,0.194390251507181,0.250000000000004,0.333175386735155,
0.356184877277791,0.375000000000004,0.422808196248102,0.471047643121825,
0.500000000000004,0.602035527258785,0.703481183539205,0.716723706355646,
0.818257118256476,0.921054244078466,1.),.UNSPECIFIED.);
#771=B_SPLINE_CURVE_WITH_KNOTS('',3,(#45337,#45338,#45339,#45340,#45341,
#45342,#45343),.UNSPECIFIED.,.F.,.F.,(4,3,4),(0.,0.5,1.),.UNSPECIFIED.);
#772=B_SPLINE_CURVE_WITH_KNOTS('',3,(#45344,#45345,#45346,#45347,#45348,
#45349,#45350,#45351,#45352,#45353,#45354,#45355,#45356,#45357,#45358,#45359,
#45360,#45361,#45362,#45363,#45364,#45365,#45366,#45367,#45368,#45369,#45370,
#45371,#45372,#45373,#45374,#45375,#45376,#45377,#45378,#45379,#45380,#45381,
#45382,#45383,#45384,#45385,#45386,#45387,#45388,#45389,#45390,#45391,#45392,
#45393,#45394,#45395,#45396,#45397,#45398,#45399,#45400,#45401),
 .UNSPECIFIED.,.F.,.F.,(4,3,3,3,3,3,3,3,3,3,3,3,3,3,3,3,3,3,3,4),(0.,0.0719184804286781,
0.148618114776114,0.169128486210845,0.249999999999983,0.335388721840469,
0.374999999999972,0.402161385818952,0.437499999999966,0.468749999999962,
0.484374999999962,0.495231216441581,0.499999999999961,0.592539932569911,
0.634235212438464,0.728584906446939,0.829025201759185,0.856412790238199,
0.961308327777253,1.),.UNSPECIFIED.);
#773=B_SPLINE_CURVE_WITH_KNOTS('',3,(#45444,#45445,#45446,#45447,#45448,
#45449,#45450,#45451,#45452,#45453,#45454,#45455,#45456,#45457,#45458,#45459,
#45460,#45461,#45462,#45463,#45464,#45465),.UNSPECIFIED.,.F.,.F.,(4,3,3,
3,3,3,3,4),(1.01036188073728E-7,0.1428571428571,0.2857142857143,0.4285714285714,
0.5714285714286,0.7142857142857,0.8571428571429,1.),.UNSPECIFIED.);
#774=B_SPLINE_CURVE_WITH_KNOTS('',3,(#45504,#45505,#45506,#45507,#45508,
#45509,#45510,#45511,#45512,#45513,#45514,#45515,#45516,#45517,#45518,#45519),
 .UNSPECIFIED.,.F.,.F.,(4,3,3,3,3,4),(0.,0.269796418766363,0.446837155942232,
0.5,0.767870847367721,0.999999999967383),.UNSPECIFIED.);
#775=B_SPLINE_CURVE_WITH_KNOTS('',3,(#45521,#45522,#45523,#45524,#45525,
#45526,#45527,#45528,#45529,#45530,#45531,#45532,#45533,#45534,#45535,#45536,
#45537,#45538,#45539,#45540,#45541,#45542,#45543,#45544,#45545,#45546,#45547,
#45548,#45549,#45550,#45551,#45552,#45553,#45554,#45555,#45556,#45557,#45558,
#45559,#45560,#45561,#45562,#45563),.UNSPECIFIED.,.F.,.F.,(4,3,3,3,3,3,
3,3,3,3,3,3,3,3,4),(0.,0.0918948483207178,0.132863053438045,0.249999999999997,
0.389695921194281,0.437499999999998,0.466122318206124,0.495108641874883,
0.499999999999999,0.616165726887126,0.729387146575313,0.772201865170694,
0.880137531088479,0.985278722839219,1.),.UNSPECIFIED.);
#776=B_SPLINE_CURVE_WITH_KNOTS('',3,(#45564,#45565,#45566,#45567,#45568,
#45569,#45570,#45571,#45572,#45573,#45574,#45575,#45576,#45577,#45578,#45579,
#45580,#45581,#45582,#45583,#45584,#45585,#45586,#45587,#45588,#45589,#45590,
#45591,#45592,#45593,#45594,#45595,#45596,#45597,#45598,#45599,#45600,#45601,
#45602,#45603,#45604,#45605,#45606,#45607,#45608,#45609,#45610,#45611,#45612,
#45613,#45614,#45615),.UNSPECIFIED.,.F.,.F.,(4,3,3,3,3,3,3,3,3,3,3,3,3,
3,3,3,3,4),(0.,0.105512176586077,0.166506332434029,0.249999999999994,0.346021730220121,
0.37499999999999,0.391545484010592,0.437499999999987,0.468749999999988,
0.484391044121635,0.499999999999989,0.595751032836016,0.626515006508435,
0.720124709531476,0.807105535962062,0.857083639881126,0.93982049409868,
1.),.UNSPECIFIED.);
#777=B_SPLINE_CURVE_WITH_KNOTS('',3,(#45657,#45658,#45659,#45660,#45661,
#45662,#45663,#45664,#45665,#45666,#45667,#45668,#45669,#45670,#45671,#45672,
#45673,#45674,#45675,#45676,#45677,#45678),.UNSPECIFIED.,.F.,.F.,(4,3,3,
3,3,3,3,4),(0.,0.1428571428571,0.2857142857143,0.4285714285714,0.5714285714286,
0.7142857142857,0.8571428571429,0.999999898936753),.UNSPECIFIED.);
#778=B_SPLINE_CURVE_WITH_KNOTS('',3,(#45681,#45682,#45683,#45684,#45685,
#45686,#45687,#45688,#45689,#45690),.UNSPECIFIED.,.F.,.F.,(4,2,2,2,4),(0.,
0.25,0.5,0.75,0.999999977827887),.UNSPECIFIED.);
#779=B_SPLINE_CURVE_WITH_KNOTS('',3,(#45720,#45721,#45722,#45723,#45724,
#45725,#45726,#45727,#45728,#45729,#45730,#45731,#45732),.UNSPECIFIED.,
 .F.,.F.,(4,3,3,3,4),(0.,0.0431918509658033,0.5,0.956806409055318,1.),
 .UNSPECIFIED.);
#780=B_SPLINE_CURVE_WITH_KNOTS('',3,(#45753,#45754,#45755,#45756,#45757,
#45758,#45759,#45760,#45761,#45762,#45763,#45764,#45765,#45766,#45767,#45768,
#45769,#45770,#45771,#45772,#45773,#45774,#45775,#45776,#45777,#45778,#45779,
#45780,#45781,#45782,#45783,#45784,#45785,#45786,#45787,#45788,#45789,#45790,
#45791,#45792,#45793,#45794,#45795,#45796,#45797,#45798,#45799,#45800,#45801,
#45802,#45803,#45804,#45805,#45806,#45807,#45808,#45809,#45810,#45811,#45812,
#45813,#45814,#45815,#45816,#45817,#45818,#45819,#45820,#45821,#45822,#45823,
#45824,#45825,#45826,#45827,#45828,#45829,#45830,#45831,#45832,#45833,#45834,
#45835,#45836,#45837,#45838,#45839,#45840,#45841,#45842,#45843,#45844,#45845,
#45846,#45847,#45848,#45849,#45850,#45851,#45852,#45853,#45854,#45855,#45856,
#45857,#45858,#45859,#45860,#45861,#45862,#45863,#45864,#45865,#45866,#45867,
#45868,#45869,#45870,#45871,#45872,#45873,#45874,#45875,#45876,#45877,#45878,
#45879,#45880,#45881,#45882,#45883,#45884,#45885,#45886,#45887,#45888,#45889,
#45890,#45891,#45892,#45893,#45894,#45895,#45896,#45897,#45898,#45899,#45900,
#45901,#45902,#45903,#45904,#45905,#45906,#45907,#45908,#45909,#45910,#45911,
#45912,#45913,#45914,#45915,#45916,#45917,#45918,#45919,#45920,#45921,#45922,
#45923,#45924,#45925,#45926,#45927,#45928,#45929,#45930,#45931,#45932,#45933,
#45934,#45935,#45936,#45937,#45938,#45939,#45940,#45941,#45942,#45943,#45944,
#45945,#45946,#45947,#45948,#45949,#45950,#45951,#45952,#45953,#45954,#45955,
#45956,#45957),.UNSPECIFIED.,.F.,.F.,(4,3,3,3,3,3,3,3,3,3,3,3,3,3,3,3,3,
3,3,3,3,3,3,3,3,3,3,3,3,3,3,3,3,3,3,3,3,3,3,3,3,3,3,3,3,3,3,3,3,3,3,3,3,
3,3,3,3,3,3,3,3,3,3,3,3,3,3,3,4),(0.,0.0249856653057896,0.0498840250895596,
0.0680623319906546,0.0924414501656426,0.107887462717563,0.131551577536791,
0.140980478615626,0.163943872360021,0.171020780779603,0.193322634140233,
0.19959032355363,0.218750000000014,0.22756874434828,0.234375000000015,0.242187500000016,
0.246093750000016,0.248046875000016,0.249023437500016,0.250000000000016,
0.254546871436753,0.279971649431658,0.307406577861317,0.309430130279663,
0.337127105577854,0.344163691684047,0.372001525912439,0.384912472908073,
0.412566458291854,0.429839310630959,0.457842489000878,0.468750000000014,
0.477238856805736,0.484375000000014,0.492187500000014,0.496093750000014,
0.498046875000014,0.500000000000014,0.531289744877457,0.565641998369439,
0.578505773627244,0.613121656100364,0.616394750861499,0.648093059813583,
0.674914453874227,0.697975730141801,0.718059302271027,0.718750000000014,
0.734375000000014,0.735681901570784,0.742187500000014,0.746093750000014,
0.748046875000014,0.749023437500014,0.750000000000014,0.75184407675242,
0.773859225905082,0.795138256456607,0.815771718220529,0.8358769872991,0.855607591022799,
0.875000000000007,0.875168004019054,0.89477993210703,0.914590311502922,
0.934773418892348,0.955588222783837,0.977473298233141,0.999999988534264),
 .UNSPECIFIED.);
#781=B_SPLINE_CURVE_WITH_KNOTS('',3,(#46120,#46121,#46122,#46123,#46124,
#46125,#46126,#46127,#46128,#46129,#46130,#46131,#46132,#46133,#46134,#46135,
#46136,#46137,#46138,#46139,#46140,#46141,#46142,#46143,#46144,#46145,#46146,
#46147,#46148,#46149,#46150,#46151,#46152,#46153,#46154,#46155,#46156,#46157,
#46158,#46159,#46160,#46161,#46162,#46163,#46164,#46165,#46166,#46167,#46168,
#46169,#46170,#46171,#46172,#46173,#46174,#46175,#46176,#46177,#46178,#46179,
#46180,#46181,#46182,#46183,#46184,#46185,#46186,#46187,#46188,#46189,#46190,
#46191,#46192,#46193,#46194,#46195,#46196,#46197,#46198,#46199,#46200,#46201,
#46202,#46203,#46204,#46205,#46206,#46207,#46208,#46209,#46210,#46211,#46212,
#46213,#46214,#46215,#46216,#46217,#46218,#46219,#46220,#46221,#46222,#46223,
#46224,#46225,#46226,#46227,#46228,#46229,#46230,#46231,#46232,#46233,#46234,
#46235,#46236,#46237,#46238,#46239,#46240),.UNSPECIFIED.,.F.,.F.,(4,3,3,
3,3,3,3,3,3,3,3,3,3,3,3,3,3,3,3,3,3,3,3,3,3,3,3,3,3,3,3,3,3,3,3,3,3,3,3,
3,4),(7.98330076221588E-8,0.031250059874758,0.0618422366267454,0.0934211183133773,
0.125000000000009,0.155569261276705,0.187159630638361,0.218750000000016,
0.234375000000017,0.242187500000018,0.246093750000018,0.248046875000018,
0.249023437500018,0.250000000000018,0.450324981199179,0.499981318201029,
0.500000000000023,0.625000000000025,0.687500000000026,0.718750000000026,
0.734375000000026,0.742187500000027,0.749511718750026,0.750000000000026,
0.765919054620212,0.781838287567876,0.797757708959856,0.81367744227693,
0.829597355433741,0.845517571883335,0.859375000000014,0.867187500000013,
0.871093750000013,0.873046875000013,0.874023437500013,0.875000000000013,
0.899836813687984,0.924877596546642,0.949727826656971,0.974863885889794,
0.999999945122618),.UNSPECIFIED.);
#782=B_SPLINE_CURVE_WITH_KNOTS('',3,(#46277,#46278,#46279,#46280,#46281,
#46282,#46283,#46284,#46285,#46286,#46287,#46288,#46289,#46290,#46291,#46292,
#46293,#46294,#46295,#46296,#46297,#46298,#46299,#46300,#46301,#46302,#46303,
#46304,#46305,#46306,#46307,#46308,#46309,#46310,#46311,#46312,#46313,#46314,
#46315,#46316,#46317,#46318,#46319,#46320,#46321,#46322,#46323,#46324,#46325),
 .UNSPECIFIED.,.F.,.F.,(4,3,3,3,3,3,3,3,3,3,3,3,3,3,3,3,4),(0.,0.077478098023877,
0.135874094516151,0.217128639935507,0.25,0.33343704912886,0.374999999999998,
0.392068058960876,0.440389336306725,0.489414520804398,0.499999999999996,
0.601853270166522,0.703313489677787,0.783418260834186,0.885329497471594,
0.988564571994781,0.999999999998388),.UNSPECIFIED.);
#783=B_SPLINE_CURVE_WITH_KNOTS('',3,(#46327,#46328,#46329,#46330,#46331,
#46332,#46333,#46334,#46335,#46336,#46337,#46338,#46339,#46340,#46341,#46342),
 .UNSPECIFIED.,.F.,.F.,(4,3,3,3,3,4),(0.,0.267749500822812,0.5,0.532448232691873,
0.802237959956232,1.),.UNSPECIFIED.);
#784=B_SPLINE_CURVE_WITH_KNOTS('',3,(#46345,#46346,#46347,#46348,#46349,
#46350,#46351,#46352,#46353,#46354,#46355,#46356,#46357,#46358,#46359,#46360,
#46361,#46362,#46363,#46364,#46365,#46366,#46367,#46368,#46369,#46370,#46371,
#46372,#46373,#46374,#46375,#46376,#46377,#46378,#46379,#46380,#46381,#46382,
#46383,#46384,#46385,#46386,#46387,#46388,#46389,#46390,#46391,#46392,#46393),
 .UNSPECIFIED.,.F.,.F.,(4,3,3,3,3,3,3,3,3,3,3,3,3,3,3,3,4),(0.,0.0744713783998642,
0.150804301319361,0.230306545116836,0.250000000000007,0.336435447589264,
0.375000000000008,0.437500000000008,0.468750000000007,0.485132844005362,
0.500000000000006,0.5872348585764,0.676833467819857,0.770825792057067,0.867637831307337,
0.969202827667639,1.),.UNSPECIFIED.);
#785=B_SPLINE_CURVE_WITH_KNOTS('',3,(#46434,#46435,#46436,#46437,#46438,
#46439,#46440,#46441,#46442,#46443,#46444,#46445,#46446,#46447,#46448,#46449,
#46450,#46451,#46452,#46453,#46454,#46455,#46456,#46457,#46458,#46459,#46460,
#46461,#46462,#46463,#46464,#46465,#46466,#46467,#46468,#46469,#46470,#46471,
#46472,#46473,#46474,#46475,#46476),.UNSPECIFIED.,.F.,.F.,(4,3,3,3,3,3,
3,3,3,3,3,3,3,3,4),(4.64734132034318E-12,0.083213773511874,0.218574767489085,
0.246109194308012,0.25,0.383459560668354,0.408370349991552,0.541180765413226,
0.570056405676159,0.702294512896255,0.731364773860962,0.75,0.881938378821876,
0.892442186051743,0.999999987394215),.UNSPECIFIED.);
#786=B_SPLINE_CURVE_WITH_KNOTS('',3,(#46477,#46478,#46479,#46480,#46481,
#46482,#46483,#46484,#46485,#46486,#46487,#46488,#46489,#46490,#46491,#46492,
#46493,#46494,#46495,#46496,#46497,#46498,#46499,#46500,#46501,#46502,#46503,
#46504,#46505,#46506,#46507,#46508,#46509,#46510,#46511,#46512,#46513,#46514,
#46515,#46516,#46517,#46518,#46519,#46520,#46521,#46522,#46523,#46524,#46525,
#46526,#46527,#46528,#46529,#46530,#46531,#46532,#46533,#46534,#46535,#46536,
#46537,#46538,#46539,#46540,#46541,#46542,#46543,#46544,#46545,#46546,#46547,
#46548,#46549,#46550,#46551,#46552,#46553,#46554,#46555),.UNSPECIFIED.,
 .F.,.F.,(4,3,3,3,3,3,3,3,3,3,3,3,3,3,3,3,3,3,3,3,3,3,3,3,3,3,4),(0.,0.0457027398302697,
0.0916124646568031,0.120396457889583,0.1428571428571,0.197268351864743,
0.251639643768668,0.275598313608457,0.2857142857143,0.349088877065947,0.412548015414617,
0.4285714285714,0.430653820896832,0.496062938448994,0.561513727370746,0.5714285714286,
0.585415481341103,0.649850597813402,0.7142857142857,0.740421636160008,0.795269302788479,
0.850185494204953,0.8571428571429,0.895775578845262,0.941868729299644,0.987754979081763,
0.999999797081979),.UNSPECIFIED.);
#787=B_SPLINE_CURVE_WITH_KNOTS('',3,(#46591,#46592,#46593,#46594,#46595,
#46596,#46597,#46598,#46599,#46600,#46601,#46602,#46603,#46604,#46605,#46606,
#46607,#46608,#46609,#46610,#46611,#46612,#46613,#46614,#46615,#46616,#46617,
#46618,#46619,#46620,#46621,#46622,#46623,#46624,#46625,#46626,#46627,#46628,
#46629,#46630,#46631,#46632,#46633,#46634,#46635,#46636,#46637,#46638,#46639,
#46640,#46641,#46642,#46643,#46644,#46645,#46646,#46647,#46648,#46649,#46650,
#46651),.UNSPECIFIED.,.F.,.F.,(4,3,3,3,3,3,3,3,3,3,3,3,3,3,3,3,3,3,3,3,
4),(8.7034819132607E-11,0.100686132890676,0.175343066445338,0.23862704943103,
0.25,0.301428394363909,0.351104884437592,0.39999698373092,0.44999849186546,
0.497446586143753,0.5,0.500001665638562,0.547538082380572,0.598153561785429,
0.647546551590073,0.698773275795036,0.75,0.812823294069069,0.887911054136799,
0.987361330124032,0.999999999998726),.UNSPECIFIED.);
#788=B_SPLINE_CURVE_WITH_KNOTS('',3,(#46692,#46693,#46694,#46695,#46696,
#46697,#46698,#46699,#46700,#46701,#46702,#46703,#46704,#46705,#46706,#46707,
#46708,#46709,#46710,#46711,#46712,#46713,#46714,#46715,#46716,#46717,#46718,
#46719,#46720,#46721,#46722,#46723,#46724,#46725,#46726,#46727,#46728,#46729,
#46730,#46731,#46732,#46733,#46734,#46735,#46736,#46737,#46738,#46739,#46740,
#46741,#46742,#46743,#46744,#46745,#46746,#46747,#46748,#46749,#46750,#46751,
#46752,#46753,#46754,#46755,#46756,#46757,#46758,#46759,#46760,#46761,#46762,
#46763,#46764,#46765,#46766,#46767,#46768,#46769,#46770,#46771,#46772,#46773,
#46774,#46775,#46776,#46777,#46778,#46779),.UNSPECIFIED.,.F.,.F.,(4,3,3,
3,3,3,3,3,3,3,3,3,3,3,3,3,3,3,3,3,3,3,3,3,3,3,3,3,3,4),(0.,0.0669970386142676,
0.120382710412332,0.125000000000001,0.187500000000001,0.218750000000001,
0.234375000000001,0.242187500000001,0.248477936970486,0.250000000000001,
0.272887810025426,0.34017169545409,0.407404427623042,0.425042432395696,
0.491875641585318,0.500000000000001,0.566167202439539,0.575220629187228,
0.625000000000001,0.687500000000002,0.718750000000001,0.727380078328301,
0.734375000000001,0.742187500000001,0.74851347129672,0.750000000000001,
0.814942759651571,0.87988551930314,0.947512676699537,1.),.UNSPECIFIED.);
#789=B_SPLINE_CURVE_WITH_KNOTS('',3,(#46807,#46808,#46809,#46810,#46811,
#46812,#46813,#46814,#46815,#46816),.UNSPECIFIED.,.F.,.F.,(4,3,3,4),(0.,
0.3333333333333,0.6666666666667,1.),.UNSPECIFIED.);
#790=B_SPLINE_CURVE_WITH_KNOTS('',3,(#46866,#46867,#46868,#46869,#46870,
#46871,#46872,#46873,#46874,#46875,#46876,#46877,#46878,#46879,#46880,#46881,
#46882,#46883,#46884,#46885,#46886,#46887,#46888,#46889,#46890,#46891,#46892,
#46893,#46894,#46895,#46896,#46897,#46898,#46899,#46900,#46901,#46902,#46903,
#46904,#46905,#46906,#46907,#46908,#46909,#46910,#46911,#46912,#46913,#46914,
#46915,#46916,#46917,#46918,#46919,#46920,#46921,#46922,#46923,#46924,#46925,
#46926,#46927,#46928,#46929,#46930,#46931,#46932,#46933,#46934,#46935,#46936,
#46937,#46938),.UNSPECIFIED.,.F.,.F.,(4,3,3,3,3,3,3,3,3,3,3,3,3,3,3,3,3,
3,3,3,3,3,3,3,4),(0.,0.0458328892270865,0.0918178602216913,0.137727870876666,
0.1428571428571,0.148536598132325,0.203804992721712,0.259124754685508,0.2857142857143,
0.296137570173946,0.362354499372673,0.4285714285714,0.443717909279761,0.51100679814713,
0.5714285714286,0.591516277430998,0.658633939571757,0.7142857142857,0.739436741598742,
0.798289799370821,0.8571428571429,0.887213042157107,0.933524276499682,0.979590782777999,
1.),.UNSPECIFIED.);
#791=B_SPLINE_CURVE_WITH_KNOTS('',3,(#46940,#46941,#46942,#46943,#46944,
#46945,#46946,#46947,#46948,#46949,#46950,#46951,#46952,#46953,#46954,#46955,
#46956,#46957,#46958,#46959,#46960,#46961,#46962,#46963,#46964,#46965,#46966,
#46967,#46968,#46969,#46970,#46971,#46972,#46973,#46974,#46975,#46976,#46977,
#46978,#46979),.UNSPECIFIED.,.F.,.F.,(4,3,3,3,3,3,3,3,3,3,3,3,3,4),(0.,
0.132990595149974,0.153369582561691,0.288984797962432,0.306719318585581,
0.443622682221199,0.460361901680837,0.597256082674871,0.614811262622601,
0.75,0.769627678904013,0.909364143399665,0.92460957800544,1.),
 .UNSPECIFIED.);
#792=B_SPLINE_CURVE_WITH_KNOTS('',3,(#46980,#46981,#46982,#46983,#46984,
#46985,#46986,#46987,#46988,#46989,#46990,#46991,#46992,#46993,#46994,#46995,
#46996,#46997,#46998,#46999,#47000,#47001,#47002,#47003,#47004,#47005,#47006,
#47007,#47008,#47009,#47010,#47011,#47012,#47013,#47014,#47015,#47016,#47017,
#47018,#47019,#47020,#47021,#47022,#47023,#47024,#47025,#47026,#47027,#47028,
#47029,#47030,#47031),.UNSPECIFIED.,.F.,.F.,(4,3,3,3,3,3,3,3,3,3,3,3,3,
3,3,3,3,4),(0.,0.0996458179615122,0.194999931615914,0.249999999999888,0.342098757858286,
0.374999999999833,0.437499999999808,0.468749999999796,0.484374999999795,
0.494788821211196,0.499999999999793,0.582568432156327,0.661614822642106,
0.737537010890375,0.809528033495748,0.879516105785263,0.946950744268271,
1.),.UNSPECIFIED.);
#793=B_SPLINE_CURVE_WITH_KNOTS('',3,(#47071,#47072,#47073,#47074,#47075,
#47076,#47077),.UNSPECIFIED.,.F.,.F.,(4,3,4),(0.,0.5,0.999999999974384),
 .UNSPECIFIED.);
#794=B_SPLINE_CURVE_WITH_KNOTS('',3,(#47078,#47079,#47080,#47081,#47082,
#47083,#47084,#47085,#47086,#47087,#47088,#47089,#47090,#47091,#47092,#47093,
#47094,#47095,#47096,#47097,#47098,#47099,#47100,#47101,#47102,#47103,#47104,
#47105,#47106,#47107,#47108,#47109,#47110,#47111,#47112,#47113,#47114,#47115,
#47116,#47117),.UNSPECIFIED.,.F.,.F.,(4,3,3,3,3,3,3,3,3,3,3,3,3,4),(0.,
0.0902944655579604,0.118857317209722,0.250000000000003,0.363581344801778,
0.437500000000005,0.466152583203494,0.495170166324027,0.500000000000006,
0.615785321962388,0.718419711808763,0.827854048198698,0.933927706970455,
1.),.UNSPECIFIED.);
#795=B_SPLINE_CURVE_WITH_KNOTS('',3,(#47161,#47162,#47163,#47164,#47165,
#47166,#47167,#47168,#47169,#47170,#47171,#47172,#47173,#47174,#47175,#47176,
#47177,#47178,#47179,#47180,#47181,#47182,#47183,#47184,#47185,#47186,#47187,
#47188,#47189,#47190,#47191,#47192,#47193,#47194,#47195,#47196,#47197,#47198,
#47199,#47200,#47201,#47202,#47203,#47204,#47205,#47206,#47207,#47208,#47209,
#47210,#47211,#47212,#47213,#47214,#47215,#47216,#47217,#47218,#47219,#47220,
#47221,#47222,#47223,#47224,#47225,#47226,#47227,#47228,#47229,#47230,#47231,
#47232,#47233,#47234,#47235,#47236,#47237,#47238,#47239,#47240,#47241,#47242),
 .UNSPECIFIED.,.F.,.F.,(4,3,3,3,3,3,3,3,3,3,3,3,3,3,3,3,3,3,3,3,3,3,3,3,
3,3,3,4),(0.,0.0670666130844619,0.12030178167153,0.125,0.1875,0.21875,0.234375,
0.243836099690824,0.25,0.273217637634883,0.340387408247809,0.407458049097731,
0.42502958529848,0.491732958316918,0.5,0.56585106029968,0.574716454972842,
0.625,0.6875,0.71875,0.726524647119784,0.734375,0.743877173835152,0.75,
0.814715983346842,0.879431966693684,0.947069143523809,1.),.UNSPECIFIED.);
#796=B_SPLINE_CURVE_WITH_KNOTS('',3,(#47243,#47244,#47245,#47246,#47247,
#47248,#47249,#47250,#47251,#47252,#47253,#47254,#47255,#47256,#47257,#47258,
#47259,#47260,#47261,#47262,#47263,#47264,#47265,#47266,#47267,#47268,#47269,
#47270,#47271,#47272,#47273,#47274,#47275,#47276,#47277,#47278,#47279,#47280,
#47281,#47282,#47283,#47284,#47285),.UNSPECIFIED.,.F.,.F.,(4,3,3,3,3,3,
3,3,3,3,3,3,3,3,4),(0.,0.120531524854355,0.242397124478255,0.25,0.27549375772157,
0.398768379129118,0.425841349187489,0.549212605428686,0.573906646855301,
0.697195745258833,0.724246467936576,0.75,0.871872563813813,0.879199606827093,
0.99999999999059),.UNSPECIFIED.);
#797=B_SPLINE_CURVE_WITH_KNOTS('',3,(#47322,#47323,#47324,#47325,#47326,
#47327,#47328,#47329,#47330,#47331,#47332,#47333,#47334,#47335,#47336,#47337,
#47338,#47339,#47340,#47341,#47342,#47343,#47344,#47345,#47346,#47347,#47348,
#47349,#47350,#47351,#47352,#47353,#47354,#47355,#47356,#47357,#47358,#47359,
#47360,#47361,#47362,#47363,#47364,#47365,#47366,#47367,#47368,#47369,#47370,
#47371,#47372,#47373,#47374,#47375,#47376,#47377,#47378,#47379,#47380,#47381,
#47382,#47383,#47384,#47385,#47386,#47387,#47388,#47389,#47390,#47391,#47392,
#47393,#47394,#47395,#47396,#47397,#47398,#47399,#47400,#47401,#47402,#47403,
#47404,#47405,#47406,#47407,#47408,#47409,#47410,#47411,#47412,#47413,#47414,
#47415,#47416,#47417,#47418,#47419,#47420,#47421,#47422,#47423,#47424,#47425,
#47426,#47427,#47428,#47429,#47430,#47431,#47432,#47433,#47434,#47435,#47436,
#47437,#47438,#47439,#47440,#47441,#47442,#47443,#47444,#47445,#47446,#47447,
#47448,#47449,#47450,#47451,#47452,#47453,#47454),.UNSPECIFIED.,.F.,.F.,
(4,3,3,3,3,3,3,3,3,3,3,3,3,3,3,3,3,3,3,3,3,3,3,3,3,3,3,3,3,3,3,3,3,3,3,
3,3,3,3,3,3,3,3,3,4),(7.5007832586842E-8,0.0217670658682142,0.0431895788594497,
0.0625000000000103,0.0832736756201858,0.0937500000000153,0.109375000000018,
0.117187500000019,0.12109375000002,0.12304687500002,0.12451171875002,0.12500000000002,
0.152494864340801,0.179650433481905,0.187500000000019,0.214360095933258,
0.218750000000018,0.234375000000018,0.24351577464818,0.250000000000018,
0.312500000000017,0.365427443838984,0.375000000000015,0.416806169790061,
0.437500000000014,0.468750000000014,0.484375000000013,0.492187500000013,
0.499677511217752,0.500000000000013,0.544190340299808,0.589518547111297,
0.625000000000011,0.684246463305914,0.687500000000009,0.718750000000009,
0.734375000000008,0.742187500000008,0.746093750000008,0.749474899577793,
0.750000000000008,0.815485730321359,0.881497052371249,0.948535357396417,
1.),.UNSPECIFIED.);
#798=B_SPLINE_CURVE_WITH_KNOTS('',3,(#47455,#47456,#47457,#47458,#47459,
#47460,#47461,#47462,#47463,#47464),.UNSPECIFIED.,.F.,.F.,(4,2,2,2,4),(2.21660080701014E-8,
0.25,0.5,0.75,1.),.UNSPECIFIED.);
#799=B_SPLINE_CURVE_WITH_KNOTS('',3,(#47598,#47599,#47600,#47601,#47602,
#47603,#47604,#47605,#47606,#47607,#47608,#47609,#47610,#47611,#47612,#47613,
#47614,#47615,#47616,#47617,#47618,#47619,#47620,#47621,#47622,#47623,#47624,
#47625,#47626,#47627,#47628,#47629,#47630,#47631,#47632,#47633,#47634,#47635,
#47636,#47637,#47638,#47639,#47640,#47641,#47642,#47643,#47644,#47645,#47646,
#47647,#47648,#47649,#47650,#47651,#47652,#47653,#47654,#47655,#47656,#47657,
#47658,#47659,#47660,#47661,#47662,#47663,#47664,#47665,#47666,#47667,#47668,
#47669,#47670,#47671,#47672,#47673,#47674,#47675,#47676,#47677,#47678,#47679,
#47680,#47681,#47682,#47683,#47684,#47685),.UNSPECIFIED.,.F.,.F.,(4,2,2,
1,2,2,2,1,1,1,2,2,2,2,1,1,1,2,2,2,2,2,2,2,2,2,1,2,2,2,1,1,2,2,2,2,1,1,2,
2,2,2,1,1,2,2,2,1,1,2,2,4),(0.,0.0312500000000003,0.0468750000000006,0.0546875000000004,
0.0585937500000001,0.0624999999999998,0.0937499999999988,0.109374999999998,
0.117187499999998,0.121093749999998,0.123046874999998,0.124999999999998,
0.187499999999995,0.218749999999994,0.234374999999994,0.242187499999994,
0.246093749999994,0.248046874999994,0.249999999999994,0.312499999999996,
0.343749999999997,0.359374999999998,0.374999999999998,0.4375,0.468750000000001,
0.484375000000002,0.492187500000002,0.496093750000002,0.500000000000003,
0.562500000000005,0.593750000000006,0.609375000000007,0.617187500000007,
0.625000000000007,0.687500000000008,0.718750000000009,0.734375000000009,
0.742187500000009,0.746093750000009,0.750000000000009,0.812500000000006,
0.843750000000005,0.859375000000004,0.867187500000004,0.871093750000004,
0.875000000000004,0.906250000000002,0.921875000000002,0.929687500000001,
0.933593750000001,0.937500000000001,1.),.UNSPECIFIED.);
#800=B_SPLINE_CURVE_WITH_KNOTS('',3,(#47732,#47733,#47734,#47735,#47736,
#47737,#47738,#47739,#47740,#47741,#47742,#47743,#47744,#47745,#47746,#47747,
#47748,#47749,#47750,#47751,#47752,#47753),.UNSPECIFIED.,.F.,.F.,(4,3,3,
3,3,3,3,4),(1.01038572354475E-7,0.1428571428571,0.2857142857143,0.4285714285714,
0.5714285714286,0.7142857142857,0.8571428571429,1.),.UNSPECIFIED.);
#801=B_SPLINE_CURVE_WITH_KNOTS('',3,(#47754,#47755,#47756,#47757,#47758,
#47759,#47760,#47761,#47762,#47763,#47764,#47765,#47766,#47767,#47768,#47769,
#47770,#47771,#47772,#47773,#47774,#47775,#47776,#47777,#47778,#47779,#47780,
#47781,#47782,#47783,#47784,#47785,#47786,#47787,#47788,#47789,#47790,#47791,
#47792,#47793,#47794,#47795,#47796,#47797,#47798,#47799,#47800,#47801,#47802,
#47803,#47804,#47805),.UNSPECIFIED.,.F.,.F.,(4,3,3,3,3,3,3,3,3,3,3,3,3,
3,3,3,3,4),(0.,0.065830358537903,0.133277278734282,0.203793753321675,0.25000000000003,
0.328519758658406,0.375000000000045,0.437500000000051,0.468750000000049,
0.48437500000005,0.495342149468993,0.50000000000005,0.586653387589681,0.675658006518003,
0.76905306807574,0.865255834852487,0.966232492263845,1.),.UNSPECIFIED.);
#802=B_SPLINE_CURVE_WITH_KNOTS('',3,(#47843,#47844,#47845,#47846,#47847,
#47848,#47849,#47850,#47851,#47852,#47853,#47854,#47855,#47856,#47857,#47858,
#47859,#47860,#47861,#47862,#47863,#47864,#47865,#47866,#47867,#47868,#47869,
#47870,#47871,#47872,#47873,#47874,#47875,#47876,#47877,#47878,#47879,#47880,
#47881,#47882,#47883,#47884,#47885,#47886,#47887,#47888,#47889,#47890,#47891),
 .UNSPECIFIED.,.F.,.F.,(4,3,3,3,3,3,3,3,3,3,3,3,3,3,3,3,4),(0.,0.0770829581291472,
0.115833104594291,0.197028807380885,0.250000000000002,0.333153117301368,
0.356333767049974,0.375000000000002,0.422947860458973,0.471329030452833,
0.500000000000003,0.606855024376987,0.708280894756902,0.713710048753971,
0.815228553265648,0.918005904080637,1.),.UNSPECIFIED.);
#803=B_SPLINE_CURVE_WITH_KNOTS('',3,(#47892,#47893,#47894,#47895,#47896,
#47897,#47898),.UNSPECIFIED.,.F.,.F.,(4,3,4),(1.79043455598195E-11,0.5,
0.999999979798419),.UNSPECIFIED.);
#804=B_SPLINE_CURVE_WITH_KNOTS('',3,(#47939,#47940,#47941,#47942,#47943,
#47944,#47945),.UNSPECIFIED.,.F.,.F.,(4,3,4),(0.,0.5,1.),.UNSPECIFIED.);
#805=B_SPLINE_CURVE_WITH_KNOTS('',3,(#47947,#47948,#47949,#47950,#47951,
#47952,#47953,#47954,#47955,#47956,#47957,#47958,#47959,#47960,#47961,#47962,
#47963,#47964,#47965,#47966,#47967,#47968,#47969,#47970,#47971,#47972,#47973,
#47974,#47975,#47976,#47977,#47978,#47979,#47980,#47981,#47982,#47983,#47984,
#47985,#47986,#47987,#47988,#47989),.UNSPECIFIED.,.F.,.F.,(4,3,3,3,3,3,
3,3,3,3,3,3,3,3,4),(0.,0.0912182191841853,0.112406184524464,0.234107463982405,
0.249999999999994,0.356823512053016,0.437499999999994,0.466379266642358,
0.495620975073898,0.499999999999994,0.61567283621949,0.711311199443657,
0.820914964356108,0.927083278900066,1.),.UNSPECIFIED.);
#806=B_SPLINE_CURVE_WITH_KNOTS('',3,(#47990,#47991,#47992,#47993,#47994,
#47995,#47996,#47997,#47998,#47999,#48000,#48001,#48002,#48003,#48004,#48005,
#48006,#48007,#48008,#48009,#48010,#48011,#48012,#48013,#48014,#48015,#48016,
#48017,#48018,#48019,#48020,#48021,#48022,#48023,#48024,#48025,#48026,#48027,
#48028,#48029,#48030,#48031,#48032,#48033,#48034,#48035,#48036,#48037,#48038,
#48039,#48040,#48041,#48042,#48043,#48044,#48045,#48046,#48047),
 .UNSPECIFIED.,.F.,.F.,(4,3,3,3,3,3,3,3,3,3,3,3,3,3,3,3,3,3,3,4),(0.,0.103649568295827,
0.142660071316879,0.249999999999991,0.34718853504273,0.365815758592943,
0.374999999999986,0.437499999999983,0.468749999999981,0.48437499999998,
0.494825109892429,0.49999999999998,0.589167146235496,0.599109405757341,
0.685328701907224,0.74999999999999,0.831438322732351,0.908502174159926,
0.980614281843201,1.),.UNSPECIFIED.);
#807=B_SPLINE_CURVE_WITH_KNOTS('',3,(#48093,#48094,#48095,#48096,#48097,
#48098,#48099,#48100,#48101,#48102,#48103,#48104,#48105,#48106,#48107,#48108,
#48109,#48110,#48111,#48112,#48113,#48114,#48115,#48116,#48117,#48118,#48119,
#48120,#48121,#48122,#48123,#48124,#48125,#48126,#48127,#48128,#48129,#48130,
#48131,#48132,#48133,#48134,#48135,#48136,#48137,#48138,#48139,#48140,#48141,
#48142,#48143,#48144,#48145,#48146,#48147,#48148,#48149,#48150,#48151,#48152,
#48153,#48154,#48155,#48156,#48157,#48158,#48159,#48160,#48161,#48162,#48163,
#48164,#48165),.UNSPECIFIED.,.F.,.F.,(4,3,3,3,3,3,3,3,3,3,3,3,3,3,3,3,3,
3,3,3,3,3,3,3,4),(0.,0.045832881241204,0.0918178429888426,0.137727842667475,
0.1428571428571,0.148537109981302,0.203805441048692,0.259125141483677,0.2857142857143,
0.296138265585979,0.362354847078689,0.4285714285714,0.443718112652216,0.511007039282419,
0.5714285714286,0.591515929724954,0.658633627239864,0.7142857142857,0.739436118141299,
0.7982894876421,0.8571428571429,0.887212493461699,0.933523713871146,0.979590209317017,
1.),.UNSPECIFIED.);
#808=B_SPLINE_CURVE_WITH_KNOTS('',3,(#48168,#48169,#48170,#48171,#48172,
#48173,#48174,#48175,#48176,#48177,#48178,#48179,#48180,#48181,#48182,#48183,
#48184,#48185,#48186,#48187,#48188,#48189,#48190,#48191,#48192,#48193,#48194,
#48195,#48196,#48197,#48198,#48199,#48200,#48201,#48202,#48203,#48204,#48205,
#48206,#48207),.UNSPECIFIED.,.F.,.F.,(4,3,3,3,3,3,3,3,3,3,3,3,3,4),(0.,
0.132990611297914,0.153370101342381,0.288985346045089,0.306720032640923,
0.443623462076149,0.460362109994673,0.597256328470644,0.614810899859838,
0.75,0.769627029706129,0.909362740892189,0.924609009850741,0.999999999982011),
 .UNSPECIFIED.);
#809=B_SPLINE_CURVE_WITH_KNOTS('',3,(#48230,#48231,#48232,#48233,#48234,
#48235,#48236,#48237,#48238,#48239),.UNSPECIFIED.,.F.,.F.,(4,3,3,4),(0.,
0.3333333333333,0.6666666666667,1.),.UNSPECIFIED.);
#810=B_SPLINE_CURVE_WITH_KNOTS('',3,(#48375,#48376,#48377,#48378,#48379,
#48380,#48381,#48382,#48383,#48384,#48385,#48386,#48387,#48388,#48389,#48390,
#48391,#48392,#48393,#48394,#48395,#48396,#48397,#48398,#48399,#48400,#48401,
#48402,#48403,#48404,#48405,#48406,#48407,#48408,#48409,#48410,#48411,#48412,
#48413,#48414,#48415,#48416,#48417,#48418,#48419,#48420,#48421,#48422,#48423,
#48424,#48425,#48426,#48427,#48428,#48429,#48430,#48431,#48432,#48433,#48434,
#48435,#48436,#48437,#48438,#48439,#48440,#48441,#48442,#48443,#48444,#48445,
#48446,#48447,#48448,#48449,#48450,#48451,#48452,#48453,#48454,#48455,#48456,
#48457,#48458,#48459,#48460,#48461),.UNSPECIFIED.,.F.,.F.,(4,2,2,1,2,2,
2,1,1,1,2,2,2,2,1,1,1,2,2,2,2,2,2,2,2,1,1,2,2,2,1,1,2,2,2,2,1,1,2,2,2,2,
1,1,2,2,2,1,1,2,2,4),(0.,0.0312499999999956,0.0468749999999935,0.0546874999999927,
0.0585937499999926,0.0624999999999925,0.0937499999999921,0.109374999999992,
0.117187499999992,0.121093749999992,0.123046874999992,0.124999999999992,
0.187499999999993,0.218749999999993,0.234374999999993,0.242187499999993,
0.246093749999993,0.248046874999993,0.249999999999993,0.312499999999994,
0.343749999999994,0.359374999999994,0.374999999999994,0.437499999999994,
0.468749999999994,0.484374999999994,0.492187499999994,0.496093749999994,
0.499999999999994,0.562499999999994,0.593749999999994,0.609374999999994,
0.617187499999994,0.624999999999994,0.687499999999994,0.718749999999995,
0.734374999999995,0.742187499999995,0.746093749999995,0.749999999999995,
0.812499999999997,0.843749999999998,0.859374999999998,0.867187499999998,
0.871093749999998,0.874999999999998,0.906249999999999,0.921874999999999,
0.9296875,0.93359375,0.9375,1.),.UNSPECIFIED.);
#811=B_SPLINE_CURVE_WITH_KNOTS('',3,(#48464,#48465,#48466,#48467,#48468,
#48469,#48470,#48471,#48472,#48473,#48474,#48475,#48476,#48477,#48478,#48479,
#48480,#48481,#48482,#48483,#48484,#48485,#48486,#48487,#48488,#48489,#48490,
#48491,#48492,#48493,#48494,#48495,#48496,#48497,#48498,#48499,#48500,#48501,
#48502,#48503,#48504,#48505,#48506,#48507,#48508,#48509,#48510,#48511,#48512,
#48513,#48514,#48515,#48516,#48517,#48518,#48519,#48520,#48521,#48522,#48523,
#48524,#48525,#48526,#48527,#48528,#48529,#48530,#48531,#48532,#48533,#48534,
#48535,#48536,#48537,#48538,#48539,#48540,#48541,#48542,#48543,#48544,#48545,
#48546,#48547,#48548,#48549,#48550,#48551,#48552,#48553,#48554,#48555,#48556,
#48557,#48558,#48559,#48560,#48561,#48562,#48563,#48564,#48565,#48566,#48567,
#48568,#48569,#48570,#48571,#48572,#48573,#48574,#48575,#48576,#48577,#48578,
#48579,#48580,#48581,#48582,#48583,#48584,#48585,#48586,#48587,#48588,#48589,
#48590,#48591,#48592,#48593,#48594,#48595,#48596,#48597,#48598,#48599,#48600,
#48601,#48602,#48603,#48604,#48605,#48606,#48607,#48608,#48609,#48610,#48611,
#48612,#48613,#48614,#48615,#48616,#48617,#48618,#48619,#48620,#48621,#48622,
#48623,#48624,#48625,#48626,#48627,#48628,#48629,#48630,#48631,#48632,#48633,
#48634,#48635,#48636,#48637,#48638,#48639,#48640,#48641,#48642,#48643,#48644,
#48645,#48646,#48647,#48648,#48649,#48650),.UNSPECIFIED.,.F.,.F.,(4,3,3,
3,3,3,3,3,3,3,3,3,3,3,3,3,3,3,3,3,3,3,3,3,3,3,3,3,3,3,3,3,3,3,3,3,3,3,3,
3,3,3,3,3,3,3,3,3,3,3,3,3,3,3,3,3,3,3,3,3,3,3,4),(7.50077796095116E-8,2.1834712232905E-7,
0.0229486522988532,0.029115344241334,0.0509750486302945,0.0551857885997794,
0.0625000000000054,0.0795341640465225,0.100118382040926,0.102946158886626,
0.109375000000009,0.11718750000001,0.12109375000001,0.123046875000011,0.124511718750011,
0.125000000000011,0.126823937250289,0.154172453479257,0.168540242544379,
0.195094304959414,0.207813101074959,0.23437500000001,0.243585841679061,
0.245601800237161,0.25000000000001,0.286460598154731,0.323176994279279,
0.335372913036784,0.372213805675533,0.396049928737796,0.433011067267819,
0.468750000000008,0.471303252420127,0.484375000000008,0.492187500000008,
0.499323792057643,0.500000000000007,0.539363292696495,0.553186327532695,
0.592468810689562,0.619362211295797,0.658497292358972,0.673124010224558,
0.711990573304192,0.716723793723807,0.718750000000005,0.734375000000005,
0.742187500000005,0.746093750000005,0.749489149398016,0.750000000000005,
0.75369509666723,0.78978336194932,0.822481585671004,0.85189171104547,0.878121450578709,
0.901492804926207,0.922411611492371,0.941273455320735,0.958424926741568,
0.974021468761295,0.988170844049958,1.),.UNSPECIFIED.);
#812=B_SPLINE_CURVE_WITH_KNOTS('',3,(#48687,#48688,#48689,#48690,#48691,
#48692,#48693,#48694,#48695,#48696),.UNSPECIFIED.,.F.,.F.,(4,2,2,2,4),(2.21659726367817E-8,
0.25,0.5,0.75,1.),.UNSPECIFIED.);
#813=B_SPLINE_CURVE_WITH_KNOTS('',3,(#48697,#48698,#48699,#48700,#48701,
#48702,#48703,#48704,#48705,#48706,#48707,#48708,#48709,#48710,#48711,#48712,
#48713,#48714,#48715,#48716,#48717,#48718,#48719,#48720,#48721,#48722,#48723,
#48724,#48725,#48726,#48727,#48728,#48729,#48730,#48731,#48732,#48733,#48734,
#48735,#48736,#48737,#48738,#48739,#48740,#48741,#48742,#48743,#48744,#48745,
#48746,#48747,#48748,#48749,#48750,#48751,#48752,#48753,#48754,#48755,#48756,
#48757),.UNSPECIFIED.,.F.,.F.,(4,3,3,3,3,3,3,3,3,3,3,3,3,3,3,3,3,3,3,3,
4),(3.81864810483332E-11,0.100941758984912,0.175470879492456,0.239253214458431,
0.25,0.301331982929159,0.350998987196869,0.399809398891569,0.449904699445784,
0.497278586630275,0.5,0.500002028503135,0.54746307741508,0.595562936975098,
0.644828923272954,0.697414461636477,0.75,0.813347304646379,0.889651753803061,
0.988069371159003,0.999999999951421),.UNSPECIFIED.);
#814=B_SPLINE_CURVE_WITH_KNOTS('',3,(#48812,#48813,#48814,#48815,#48816,
#48817,#48818,#48819,#48820,#48821,#48822,#48823,#48824,#48825,#48826,#48827,
#48828,#48829,#48830,#48831,#48832,#48833,#48834,#48835,#48836,#48837,#48838,
#48839,#48840,#48841,#48842,#48843,#48844,#48845,#48846,#48847,#48848,#48849,
#48850,#48851,#48852,#48853,#48854,#48855,#48856,#48857,#48858,#48859,#48860,
#48861,#48862,#48863,#48864,#48865,#48866,#48867,#48868,#48869,#48870,#48871,
#48872,#48873,#48874,#48875,#48876,#48877,#48878,#48879,#48880,#48881,#48882,
#48883,#48884,#48885,#48886,#48887,#48888,#48889,#48890,#48891,#48892,#48893,
#48894,#48895,#48896,#48897,#48898,#48899,#48900,#48901,#48902,#48903,#48904,
#48905,#48906,#48907,#48908,#48909,#48910,#48911,#48912,#48913,#48914,#48915,
#48916,#48917,#48918,#48919,#48920),.UNSPECIFIED.,.F.,.F.,(4,3,3,3,3,3,
3,3,3,3,3,3,3,3,3,3,3,3,3,3,3,3,3,3,3,3,3,3,3,3,3,3,3,3,3,3,4),(0.,0.0469750755483397,
0.107013261195238,0.125000000000003,0.158323162137369,0.187500000000005,
0.218750000000006,0.234375000000006,0.242187500000006,0.246093750000006,
0.248046875000006,0.250000000000006,0.272270513448122,0.328769794302826,
0.380131831410091,0.436169931231429,0.490512436112259,0.500000000000005,
0.500020141526524,0.552994048955501,0.607576031489257,0.619923874724667,
0.625000000000005,0.682586167998106,0.687500000000005,0.718750000000005,
0.727765077201715,0.734375000000005,0.742187500000005,0.746093750000005,
0.748046875000005,0.750000000000005,0.808692100492686,0.841709576216595,
0.902639581263564,0.953058336704736,0.999999999999993),.UNSPECIFIED.);
#815=B_SPLINE_CURVE_WITH_KNOTS('',3,(#48959,#48960,#48961,#48962,#48963,
#48964,#48965,#48966,#48967,#48968,#48969,#48970,#48971,#48972,#48973,#48974,
#48975,#48976,#48977,#48978,#48979,#48980,#48981,#48982,#48983,#48984,#48985,
#48986,#48987,#48988,#48989,#48990,#48991,#48992,#48993,#48994,#48995,#48996,
#48997,#48998,#48999,#49000,#49001,#49002,#49003,#49004),.UNSPECIFIED.,
 .F.,.F.,(4,3,3,3,3,3,3,3,3,3,3,3,3,3,3,4),(0.,0.0782430522660074,0.11197985752849,
0.1933350730998,0.249999999999997,0.333365304872076,0.352554727932383,0.374999999999995,
0.421439760445618,0.468291981355138,0.499999999999995,0.60472551068549,
0.709451021370985,0.81095438778007,0.913715460883307,1.),.UNSPECIFIED.);
#816=B_SPLINE_CURVE_WITH_KNOTS('',3,(#49005,#49006,#49007,#49008,#49009,
#49010,#49011),.UNSPECIFIED.,.F.,.F.,(4,3,4),(0.,0.5,1.),.UNSPECIFIED.);
#817=B_SPLINE_CURVE_WITH_KNOTS('',3,(#49012,#49013,#49014,#49015,#49016,
#49017,#49018,#49019,#49020,#49021,#49022,#49023,#49024,#49025,#49026,#49027,
#49028,#49029,#49030,#49031,#49032,#49033,#49034,#49035,#49036,#49037,#49038,
#49039,#49040,#49041,#49042,#49043,#49044,#49045,#49046,#49047,#49048,#49049,
#49050,#49051,#49052,#49053,#49054,#49055,#49056,#49057,#49058,#49059,#49060,
#49061,#49062,#49063,#49064,#49065,#49066,#49067,#49068,#49069),
 .UNSPECIFIED.,.F.,.F.,(4,3,3,3,3,3,3,3,3,3,3,3,3,3,3,3,3,3,3,4),(0.,0.0713925938266771,
0.147548684834906,0.169708372945268,0.249999999999987,0.33487881468383,
0.374999999999981,0.402047408896451,0.43749999999998,0.468749999999982,
0.484374999999984,0.49538572687912,0.499999999999986,0.594440192107133,
0.635063053479894,0.732129617709673,0.835445829871013,0.857807936589943,
0.961497480103932,1.),.UNSPECIFIED.);
#818=B_SPLINE_CURVE_WITH_KNOTS('',3,(#49112,#49113,#49114,#49115,#49116,
#49117,#49118,#49119,#49120,#49121,#49122,#49123,#49124,#49125,#49126,#49127,
#49128,#49129,#49130,#49131,#49132,#49133),.UNSPECIFIED.,.F.,.F.,(4,3,3,
3,3,3,3,4),(1.01038257746567E-7,0.1428571428571,0.2857142857143,0.4285714285714,
0.5714285714286,0.7142857142857,0.8571428571429,1.),.UNSPECIFIED.);
#819=B_SPLINE_CURVE_WITH_KNOTS('',3,(#49176,#49177,#49178,#49179,#49180,
#49181,#49182),.UNSPECIFIED.,.F.,.F.,(4,3,4),(0.,0.5,1.),.UNSPECIFIED.);
#820=B_SPLINE_CURVE_WITH_KNOTS('',3,(#49184,#49185,#49186,#49187,#49188,
#49189,#49190,#49191,#49192,#49193,#49194,#49195,#49196,#49197,#49198,#49199,
#49200,#49201,#49202,#49203,#49204,#49205,#49206,#49207,#49208,#49209,#49210,
#49211,#49212,#49213,#49214,#49215,#49216,#49217,#49218,#49219,#49220,#49221,
#49222,#49223,#49224,#49225,#49226),.UNSPECIFIED.,.F.,.F.,(4,3,3,3,3,3,
3,3,3,3,3,3,3,3,4),(0.,0.0911164890363828,0.111478099373908,0.233136812955381,
0.250000000000001,0.35510274217642,0.437500000000001,0.466389059279721,
0.495640200714861,0.500000000000002,0.615671350380528,0.707817213420784,
0.817519612891894,0.923748890587099,1.),.UNSPECIFIED.);
#821=B_SPLINE_CURVE_WITH_KNOTS('',3,(#49227,#49228,#49229,#49230,#49231,
#49232,#49233,#49234,#49235,#49236,#49237,#49238,#49239,#49240,#49241,#49242,
#49243,#49244,#49245,#49246,#49247,#49248,#49249,#49250,#49251,#49252,#49253,
#49254,#49255,#49256,#49257,#49258,#49259,#49260,#49261,#49262,#49263,#49264,
#49265,#49266,#49267,#49268,#49269,#49270,#49271,#49272,#49273,#49274,#49275,
#49276,#49277,#49278,#49279,#49280,#49281,#49282,#49283,#49284),
 .UNSPECIFIED.,.F.,.F.,(4,3,3,3,3,3,3,3,3,3,3,3,3,3,3,3,3,3,3,4),(0.,0.103631820601983,
0.141618933845124,0.249999999999985,0.347157432574721,0.364507186385042,
0.374999999999978,0.437499999999977,0.46874999999998,0.484374999999984,
0.494780989963732,0.499999999999987,0.588702567953257,0.597579109022073,
0.683307469833132,0.749999999999994,0.830117206554479,0.906641913854849,
0.978194795254131,1.),.UNSPECIFIED.);
#822=B_SPLINE_CURVE_WITH_KNOTS('',3,(#49326,#49327,#49328,#49329,#49330,
#49331,#49332,#49333,#49334,#49335,#49336,#49337,#49338,#49339,#49340,#49341,
#49342,#49343,#49344,#49345,#49346,#49347),.UNSPECIFIED.,.F.,.F.,(4,3,3,
3,3,3,3,4),(0.,0.1428571428571,0.2857142857143,0.4285714285714,0.5714285714286,
0.7142857142857,0.8571428571429,0.999999898934671),.UNSPECIFIED.);
#823=B_SPLINE_CURVE_WITH_KNOTS('',3,(#49350,#49351,#49352,#49353,#49354,
#49355,#49356,#49357,#49358,#49359),.UNSPECIFIED.,.F.,.F.,(4,2,2,2,4),(0.,
0.25,0.5,0.75,0.999999977827931),.UNSPECIFIED.);
#824=B_SPLINE_CURVE_WITH_KNOTS('',3,(#49389,#49390,#49391,#49392,#49393,
#49394,#49395,#49396,#49397,#49398,#49399,#49400,#49401),.UNSPECIFIED.,
 .F.,.F.,(4,3,3,3,4),(0.,0.0431918506380903,0.5,0.956806409374189,1.),
 .UNSPECIFIED.);
#825=B_SPLINE_CURVE_WITH_KNOTS('',3,(#49422,#49423,#49424,#49425,#49426,
#49427,#49428,#49429,#49430,#49431,#49432,#49433,#49434,#49435,#49436,#49437,
#49438,#49439,#49440,#49441,#49442,#49443,#49444,#49445,#49446,#49447,#49448,
#49449,#49450,#49451,#49452,#49453,#49454,#49455,#49456,#49457,#49458,#49459,
#49460,#49461,#49462,#49463,#49464,#49465,#49466,#49467,#49468,#49469,#49470,
#49471,#49472,#49473,#49474,#49475,#49476,#49477,#49478,#49479,#49480,#49481,
#49482,#49483,#49484,#49485,#49486,#49487,#49488,#49489,#49490,#49491,#49492,
#49493,#49494,#49495,#49496,#49497,#49498,#49499,#49500,#49501,#49502,#49503,
#49504,#49505,#49506,#49507,#49508,#49509,#49510,#49511,#49512,#49513,#49514,
#49515,#49516,#49517,#49518,#49519,#49520,#49521,#49522,#49523,#49524,#49525,
#49526,#49527,#49528,#49529,#49530,#49531,#49532,#49533,#49534,#49535,#49536,
#49537,#49538,#49539,#49540,#49541,#49542,#49543,#49544,#49545,#49546,#49547,
#49548,#49549,#49550,#49551,#49552,#49553,#49554,#49555,#49556,#49557,#49558,
#49559,#49560,#49561,#49562,#49563,#49564,#49565,#49566,#49567,#49568,#49569,
#49570,#49571,#49572,#49573,#49574,#49575,#49576,#49577,#49578,#49579,#49580,
#49581,#49582,#49583,#49584,#49585,#49586,#49587,#49588,#49589,#49590,#49591,
#49592,#49593,#49594,#49595,#49596,#49597,#49598,#49599,#49600,#49601,#49602,
#49603,#49604,#49605,#49606,#49607,#49608,#49609,#49610,#49611,#49612,#49613,
#49614,#49615,#49616,#49617,#49618,#49619,#49620,#49621,#49622,#49623,#49624,
#49625,#49626),.UNSPECIFIED.,.F.,.F.,(4,3,3,3,3,3,3,3,3,3,3,3,3,3,3,3,3,
3,3,3,3,3,3,3,3,3,3,3,3,3,3,3,3,3,3,3,3,3,3,3,3,3,3,3,3,3,3,3,3,3,3,3,3,
3,3,3,3,3,3,3,3,3,3,3,3,3,3,3,4),(0.,0.0249804636836571,0.0498736791136485,
0.0680715392667395,0.0924456145405575,0.107891047923709,0.13155027304587,
0.140978184745424,0.163936834710769,0.171012733705645,0.193309979955154,
0.19957661620216,0.218750000000013,0.227549376577307,0.234375000000014,
0.242187500000015,0.246093750000015,0.248046875000015,0.249023437500015,
0.250000000000015,0.254527365901607,0.279953693811535,0.307391988817704,
0.309413242316365,0.337113752967077,0.344147025953986,0.371988483723474,
0.384896192383363,0.412553839552332,0.429823366019842,0.457830262004141,
0.468750000000032,0.477221641980619,0.484375000000033,0.492187500000034,
0.496093750000034,0.498046875000034,0.500000000000034,0.531271360692087,
0.565625668115633,0.578495294938005,0.613113327045429,0.616389579700112,
0.648091824942008,0.674916203548571,0.697979818908304,0.718065266624333,
0.718750000000046,0.734375000000046,0.735689389724538,0.742187500000047,
0.746093750000047,0.748046875000047,0.749023437500047,0.750000000000047,
0.751857160445813,0.773870925559924,0.795148605277167,0.815780746718848,
0.835884720177279,0.855614046419167,0.875000000000023,0.875173192428097,
0.894783855532303,0.914592979453005,0.93477486045262,0.955588500169355,
0.977472532414895,0.999999988514636),.UNSPECIFIED.);
#826=B_SPLINE_CURVE_WITH_KNOTS('',3,(#49789,#49790,#49791,#49792,#49793,
#49794,#49795,#49796,#49797,#49798,#49799,#49800,#49801,#49802,#49803,#49804,
#49805,#49806,#49807,#49808,#49809,#49810,#49811,#49812,#49813,#49814,#49815,
#49816,#49817,#49818,#49819,#49820,#49821,#49822,#49823,#49824,#49825,#49826,
#49827,#49828,#49829,#49830,#49831,#49832,#49833,#49834,#49835,#49836,#49837,
#49838,#49839,#49840,#49841,#49842,#49843,#49844,#49845,#49846,#49847,#49848,
#49849,#49850,#49851,#49852,#49853,#49854,#49855,#49856,#49857,#49858,#49859,
#49860,#49861,#49862,#49863,#49864,#49865,#49866,#49867,#49868,#49869,#49870,
#49871,#49872,#49873,#49874,#49875,#49876,#49877,#49878,#49879,#49880,#49881,
#49882,#49883,#49884,#49885,#49886,#49887,#49888,#49889,#49890,#49891,#49892,
#49893,#49894,#49895,#49896,#49897,#49898,#49899,#49900,#49901,#49902,#49903,
#49904,#49905,#49906,#49907,#49908,#49909),.UNSPECIFIED.,.F.,.F.,(4,3,3,
3,3,3,3,3,3,3,3,3,3,3,3,3,3,3,3,3,3,3,3,3,3,3,3,3,3,3,3,3,3,3,3,3,3,3,3,
3,4),(7.98329640859155E-8,0.0312500598747272,0.0618422344833354,0.093421117241676,
0.125000000000017,0.155569259137103,0.187159629568566,0.218750000000029,
0.234375000000031,0.242187500000032,0.246093750000032,0.248046875000033,
0.249023437500033,0.250000000000033,0.450296396147656,0.499981289091065,
0.500000000000053,0.625000000000064,0.687500000000069,0.718750000000071,
0.734375000000072,0.742187500000073,0.749511718750074,0.750000000000074,
0.765919093593849,0.781838365516704,0.797757825884924,0.813677598178679,
0.829597550311721,0.845517805734134,0.859375000000023,0.86718750000002,
0.871093750000018,0.873046875000017,0.874023437500017,0.875000000000016,
0.899836887460964,0.924877651876229,0.949727955905382,0.974863950513704,
0.999999945122025),.UNSPECIFIED.);
#827=B_SPLINE_CURVE_WITH_KNOTS('',3,(#49950,#49951,#49952,#49953,#49954,
#49955,#49956,#49957,#49958,#49959,#49960,#49961,#49962,#49963,#49964,#49965,
#49966,#49967,#49968,#49969,#49970,#49971,#49972,#49973,#49974,#49975,#49976,
#49977,#49978,#49979,#49980,#49981,#49982,#49983,#49984,#49985,#49986,#49987,
#49988,#49989,#49990,#49991,#49992,#49993,#49994,#49995),.UNSPECIFIED.,
 .F.,.F.,(4,3,3,3,3,3,3,3,3,3,3,3,3,3,3,4),(0.,0.0782533266680479,0.111885264806691,
0.193250892056667,0.25,0.333382423143553,0.353144888706974,0.375000000000001,
0.421430089632216,0.468271936287447,0.500000000000001,0.605744038432394,
0.711488076864787,0.812997093824424,0.915766521323154,1.),.UNSPECIFIED.);
#828=B_SPLINE_CURVE_WITH_KNOTS('',3,(#49997,#49998,#49999,#50000,#50001,
#50002,#50003),.UNSPECIFIED.,.F.,.F.,(4,3,4),(0.,0.5,1.),.UNSPECIFIED.);
#829=B_SPLINE_CURVE_WITH_KNOTS('',3,(#50006,#50007,#50008,#50009,#50010,
#50011,#50012,#50013,#50014,#50015,#50016,#50017,#50018,#50019,#50020,#50021,
#50022,#50023,#50024,#50025,#50026,#50027,#50028,#50029,#50030,#50031,#50032,
#50033,#50034,#50035,#50036,#50037,#50038,#50039,#50040,#50041,#50042,#50043,
#50044,#50045,#50046,#50047,#50048,#50049,#50050,#50051,#50052,#50053,#50054,
#50055,#50056,#50057,#50058,#50059,#50060,#50061,#50062,#50063),
 .UNSPECIFIED.,.F.,.F.,(4,3,3,3,3,3,3,3,3,3,3,3,3,3,3,3,3,3,3,4),(0.,0.0718960185229564,
0.148549048540975,0.168812943342999,0.250000000000035,0.335330459216654,
0.375000000000054,0.401332658039912,0.437500000000066,0.468750000000068,
0.484375000000069,0.4954147011734,0.50000000000007,0.594522675873066,0.634654368293966,
0.731775982825236,0.835154805307982,0.857963598960442,0.961721678414487,
1.),.UNSPECIFIED.);
#830=B_SPLINE_CURVE_WITH_KNOTS('',3,(#50104,#50105,#50106,#50107,#50108,
#50109,#50110,#50111,#50112,#50113,#50114,#50115,#50116,#50117,#50118,#50119,
#50120,#50121,#50122,#50123,#50124,#50125,#50126,#50127,#50128,#50129,#50130,
#50131,#50132,#50133,#50134,#50135,#50136,#50137,#50138,#50139,#50140,#50141,
#50142,#50143,#50144,#50145,#50146),.UNSPECIFIED.,.F.,.F.,(4,3,3,3,3,3,
3,3,3,3,3,3,3,3,4),(2.75833894896721E-11,0.0832137801231444,0.218577222507133,
0.246109198300411,0.25,0.383459482332676,0.408370355156758,0.541180692332896,
0.57005641089706,0.702294441295682,0.731364778032269,0.75,0.881938303227582,
0.892442188083098,0.999999987394052),.UNSPECIFIED.);
#831=B_SPLINE_CURVE_WITH_KNOTS('',3,(#50147,#50148,#50149,#50150,#50151,
#50152,#50153,#50154,#50155,#50156,#50157,#50158,#50159,#50160,#50161,#50162,
#50163,#50164,#50165,#50166,#50167,#50168,#50169,#50170,#50171,#50172,#50173,
#50174,#50175,#50176,#50177,#50178,#50179,#50180,#50181,#50182,#50183,#50184,
#50185,#50186,#50187,#50188,#50189,#50190,#50191,#50192,#50193,#50194,#50195,
#50196,#50197,#50198,#50199,#50200,#50201,#50202,#50203,#50204,#50205,#50206,
#50207,#50208,#50209,#50210,#50211,#50212,#50213,#50214,#50215,#50216,#50217,
#50218,#50219,#50220,#50221,#50222,#50223,#50224,#50225),.UNSPECIFIED.,
 .F.,.F.,(4,3,3,3,3,3,3,3,3,3,3,3,3,3,3,3,3,3,3,3,3,3,3,3,3,3,4),(0.,0.0457810645246147,
0.0917889109041794,0.120317263742967,0.1428571428571,0.198222938253958,
0.253550313181452,0.275526169261383,0.2857142857143,0.349641017084231,0.413645125780723,
0.4285714285714,0.430597661234344,0.49617639314214,0.561795640410392,0.5714285714286,
0.585374712199986,0.649830213242843,0.7142857142857,0.740396105591031,0.795252697928882,
0.850177797878476,0.8571428571429,0.895765291931708,0.941863322899958,0.987754468934129,
0.999999797061789),.UNSPECIFIED.);
#832=B_SPLINE_CURVE_WITH_KNOTS('',3,(#50261,#50262,#50263,#50264,#50265,
#50266,#50267,#50268,#50269,#50270,#50271,#50272,#50273,#50274,#50275,#50276,
#50277,#50278,#50279,#50280,#50281,#50282,#50283,#50284,#50285,#50286,#50287,
#50288,#50289,#50290,#50291,#50292,#50293,#50294,#50295,#50296,#50297,#50298,
#50299,#50300,#50301,#50302,#50303,#50304,#50305,#50306,#50307,#50308,#50309,
#50310,#50311,#50312,#50313,#50314,#50315,#50316,#50317,#50318,#50319,#50320,
#50321),.UNSPECIFIED.,.F.,.F.,(4,3,3,3,3,3,3,3,3,3,3,3,3,3,3,3,3,3,3,3,
4),(4.8303250918634E-11,0.100941512885383,0.175470756442692,0.239253174153164,
0.25,0.301331842025548,0.350998881519161,0.399809175346533,0.449904587673267,
0.49727836962675,0.5,0.500001745528387,0.547462517145405,0.595562092315673,
0.644827784964439,0.69741389248222,0.75,0.813347997687032,0.88965388098933,
0.988070502192274,0.999999999949836),.UNSPECIFIED.);
#833=B_SPLINE_CURVE_WITH_KNOTS('',3,(#50374,#50375,#50376,#50377,#50378,
#50379,#50380,#50381,#50382,#50383,#50384,#50385,#50386,#50387,#50388,#50389,
#50390,#50391,#50392,#50393,#50394,#50395,#50396,#50397,#50398,#50399,#50400,
#50401,#50402,#50403,#50404,#50405,#50406,#50407,#50408,#50409,#50410,#50411,
#50412,#50413,#50414,#50415,#50416,#50417,#50418,#50419,#50420,#50421,#50422,
#50423,#50424,#50425,#50426,#50427,#50428,#50429,#50430,#50431,#50432,#50433,
#50434,#50435,#50436,#50437,#50438,#50439,#50440,#50441,#50442,#50443,#50444,
#50445,#50446,#50447,#50448,#50449,#50450,#50451,#50452,#50453,#50454,#50455,
#50456,#50457,#50458,#50459,#50460,#50461,#50462,#50463,#50464,#50465,#50466,
#50467,#50468,#50469,#50470,#50471,#50472,#50473,#50474,#50475,#50476,#50477,
#50478,#50479,#50480,#50481,#50482),.UNSPECIFIED.,.F.,.F.,(4,3,3,3,3,3,
3,3,3,3,3,3,3,3,3,3,3,3,3,3,3,3,3,3,3,3,3,3,3,3,3,3,3,3,3,3,4),(0.,0.0467928392075614,
0.106852595902104,0.12499999999999,0.158174590936753,0.187499999999985,
0.218749999999983,0.234374999999982,0.242187499999981,0.246093749999981,
0.248046874999981,0.249999999999981,0.272158913360276,0.328161519570208,
0.380022334667793,0.435536871025077,0.489384170464846,0.499978897694337,
0.499999999999984,0.552950484647908,0.607509892827094,0.619956343228664,
0.624999999999986,0.682568620262455,0.687499999999987,0.718749999999987,
0.727810778333793,0.734374999999988,0.742187499999988,0.746093749999988,
0.748046874999988,0.749999999999988,0.808696804403464,0.841783862121717,
0.90271961245407,0.953171011994076,1.),.UNSPECIFIED.);
#834=B_SPLINE_CURVE_WITH_KNOTS('',3,(#50494,#50495,#50496,#50497,#50498,
#50499,#50500),.UNSPECIFIED.,.F.,.F.,(4,3,4),(0.,0.5,1.),.UNSPECIFIED.);
#835=B_SPLINE_CURVE_WITH_KNOTS('',3,(#50503,#50504,#50505,#50506,#50507,
#50508,#50509,#50510,#50511,#50512,#50513,#50514,#50515,#50516,#50517,#50518,
#50519,#50520,#50521,#50522,#50523,#50524,#50525,#50526,#50527,#50528,#50529,
#50530,#50531,#50532,#50533,#50534,#50535,#50536,#50537,#50538,#50539,#50540,
#50541,#50542,#50543,#50544,#50545,#50546,#50547,#50548,#50549,#50550,#50551,
#50552,#50553,#50554,#50555,#50556,#50557,#50558,#50559,#50560,#50561,#50562,
#50563,#50564,#50565,#50566,#50567,#50568,#50569,#50570,#50571,#50572,#50573,
#50574,#50575,#50576,#50577,#50578,#50579,#50580,#50581,#50582,#50583,#50584,
#50585,#50586,#50587,#50588,#50589,#50590,#50591,#50592,#50593,#50594,#50595,
#50596),.UNSPECIFIED.,.F.,.F.,(4,3,3,3,3,3,3,3,3,3,3,3,3,3,3,3,3,3,3,3,
3,3,3,3,3,3,3,3,3,3,3,4),(0.,0.0582117372293125,0.11492486666494,0.125,
0.183308049049635,0.1875,0.207496971641933,0.21875,0.234375,0.2421875,0.24802262248796,
0.25,0.317558458591829,0.355181903648077,0.422153520719486,0.487812341416293,
0.500000000000002,0.500435668994842,0.564209449619831,0.625000000000003,
0.645724511137929,0.687500000000003,0.718750000000004,0.734375000000004,
0.742187500000004,0.748068593613938,0.750000000000004,0.793398748827164,
0.850370210729963,0.908819711975139,0.942690483272083,0.999999999999969),
 .UNSPECIFIED.);
#836=B_SPLINE_CURVE_WITH_KNOTS('',3,(#50667,#50668,#50669,#50670,#50671,
#50672,#50673,#50674,#50675,#50676,#50677,#50678,#50679),.UNSPECIFIED.,
 .F.,.F.,(4,3,3,3,4),(0.,0.0431918505795297,0.5,0.95680640941812,1.),
 .UNSPECIFIED.);
#837=B_SPLINE_CURVE_WITH_KNOTS('',3,(#50725,#50726,#50727,#50728,#50729,
#50730,#50731,#50732,#50733,#50734,#50735,#50736,#50737,#50738,#50739,#50740,
#50741,#50742,#50743,#50744,#50745,#50746,#50747,#50748,#50749,#50750,#50751,
#50752,#50753,#50754,#50755,#50756,#50757,#50758,#50759,#50760,#50761,#50762,
#50763,#50764,#50765,#50766,#50767,#50768,#50769,#50770,#50771,#50772,#50773,
#50774,#50775,#50776,#50777,#50778,#50779,#50780,#50781,#50782,#50783,#50784,
#50785,#50786,#50787,#50788,#50789,#50790,#50791,#50792,#50793,#50794,#50795,
#50796,#50797,#50798,#50799,#50800,#50801,#50802,#50803,#50804,#50805,#50806,
#50807,#50808,#50809,#50810,#50811,#50812,#50813,#50814,#50815,#50816,#50817,
#50818,#50819,#50820,#50821,#50822,#50823,#50824,#50825,#50826,#50827,#50828,
#50829,#50830,#50831,#50832,#50833,#50834,#50835,#50836,#50837,#50838,#50839,
#50840,#50841,#50842,#50843,#50844,#50845,#50846,#50847,#50848,#50849,#50850,
#50851,#50852,#50853,#50854,#50855,#50856,#50857,#50858,#50859,#50860,#50861,
#50862,#50863,#50864,#50865,#50866,#50867,#50868,#50869,#50870,#50871,#50872,
#50873,#50874,#50875,#50876,#50877,#50878,#50879,#50880,#50881,#50882,#50883,
#50884,#50885,#50886,#50887,#50888,#50889,#50890,#50891,#50892,#50893,#50894,
#50895,#50896,#50897,#50898,#50899,#50900,#50901,#50902,#50903,#50904,#50905,
#50906,#50907,#50908,#50909,#50910,#50911,#50912,#50913,#50914,#50915,#50916,
#50917,#50918,#50919,#50920,#50921,#50922,#50923,#50924,#50925,#50926,#50927,
#50928,#50929),.UNSPECIFIED.,.F.,.F.,(4,3,3,3,3,3,3,3,3,3,3,3,3,3,3,3,3,
3,3,3,3,3,3,3,3,3,3,3,3,3,3,3,3,3,3,3,3,3,3,3,3,3,3,3,3,3,3,3,3,3,3,3,3,
3,3,3,3,3,3,3,3,3,3,3,3,3,3,3,4),(0.,0.024995203988787,0.0499029973964458,
0.0680454794037188,0.0924338450081712,0.10788091381137,0.131553995326861,
0.140984707974704,0.163956800589375,0.171035558786358,0.193345860615578,
0.199615480348319,0.21875000000001,0.227604280505406,0.234375000000011,
0.242187500000011,0.246093750000011,0.248046875000011,0.249023437500011,
0.250000000000011,0.254582621996816,0.280004562969263,0.307433325257189,
0.309461091902956,0.337151591648368,0.344194252658166,0.372025449551419,
0.38494233403053,0.412589612231462,0.42986856233789,0.457864930665073,0.468750000000003,
0.477270445622972,0.484375000000002,0.492187500000002,0.496093750000002,
0.498046875000001,0.500000000000001,0.531323457773232,0.565671952248005,
0.578524989644827,0.613136937399731,0.616404235470285,0.648095328173456,
0.674911251480646,0.697968240642263,0.718048375575022,0.718749999999998,
0.734374999999997,0.735668182676169,0.742187499999997,0.746093749999997,
0.748046874999997,0.749023437499997,0.749999999999997,0.751820094994314,
0.773837783154619,0.79511929168836,0.815755175333351,0.83586282083153,0.855595767527349,
0.874999999999999,0.87515850402918,0.894772751664911,0.91458543277808,0.934770787977508,
0.955587724715017,0.97747470972438,0.999999988569063),.UNSPECIFIED.);
#838=B_SPLINE_CURVE_WITH_KNOTS('',3,(#51090,#51091,#51092,#51093,#51094,
#51095,#51096,#51097,#51098,#51099,#51100,#51101,#51102,#51103,#51104,#51105,
#51106,#51107,#51108,#51109,#51110,#51111,#51112,#51113,#51114,#51115,#51116,
#51117,#51118,#51119,#51120,#51121,#51122,#51123,#51124,#51125,#51126,#51127,
#51128,#51129,#51130,#51131,#51132,#51133,#51134,#51135,#51136,#51137,#51138,
#51139,#51140,#51141,#51142,#51143,#51144,#51145,#51146,#51147,#51148,#51149,
#51150,#51151,#51152,#51153,#51154,#51155,#51156,#51157,#51158,#51159,#51160,
#51161,#51162,#51163,#51164,#51165,#51166,#51167,#51168,#51169,#51170,#51171,
#51172,#51173,#51174,#51175,#51176,#51177,#51178,#51179,#51180,#51181,#51182,
#51183,#51184,#51185,#51186,#51187,#51188,#51189,#51190,#51191,#51192,#51193,
#51194,#51195,#51196,#51197,#51198,#51199,#51200,#51201,#51202,#51203,#51204,
#51205,#51206,#51207,#51208,#51209,#51210),.UNSPECIFIED.,.F.,.F.,(4,3,3,
3,3,3,3,3,3,3,3,3,3,3,3,3,3,3,3,3,3,3,3,3,3,3,3,3,3,3,3,3,3,3,3,3,3,3,3,
3,4),(7.98332290391144E-8,0.0312500598749225,0.0618422411603766,0.0934211205801896,
0.125000000000003,0.15556926580042,0.187159632900212,0.218750000000005,
0.234375000000005,0.242187500000005,0.246093750000005,0.248046875000005,
0.249023437500006,0.250000000000006,0.450377472834497,0.499981371599594,
0.500000000000035,0.625000000000049,0.687500000000057,0.71875000000006,
0.734375000000062,0.742187500000063,0.749511718750063,0.750000000000063,
0.765918986321078,0.781838150966254,0.79775750405352,0.813677169065249,
0.829597013916694,0.845517162064315,0.859375000000035,0.867187500000033,
0.871093750000032,0.873046875000031,0.874023437500031,0.875000000000031,
0.899836671865672,0.924877490179526,0.949727578183808,0.974863761652447,
0.999999945121086),.UNSPECIFIED.);
#839=B_SPLINE_CURVE_WITH_KNOTS('',3,(#51247,#51248,#51249,#51250,#51251,
#51252,#51253,#51254,#51255,#51256,#51257,#51258,#51259,#51260,#51261,#51262,
#51263,#51264,#51265,#51266,#51267,#51268,#51269,#51270,#51271,#51272,#51273,
#51274,#51275,#51276,#51277,#51278,#51279,#51280),.UNSPECIFIED.,.F.,.F.,
(4,3,3,3,3,3,3,3,3,3,3,4),(1.02990837813416E-11,0.133918786859822,0.21381289071477,
0.25,0.377666333223483,0.484760468447434,0.5,0.631307102429207,0.75,0.754458269127967,
0.879638408390619,0.999999987393856),.UNSPECIFIED.);
#840=B_SPLINE_CURVE_WITH_KNOTS('',3,(#51281,#51282,#51283,#51284,#51285,
#51286,#51287,#51288,#51289,#51290,#51291,#51292,#51293,#51294,#51295,#51296,
#51297,#51298,#51299,#51300,#51301,#51302,#51303,#51304,#51305,#51306,#51307,
#51308,#51309,#51310,#51311,#51312,#51313,#51314,#51315,#51316,#51317,#51318,
#51319,#51320,#51321,#51322,#51323,#51324,#51325,#51326,#51327,#51328,#51329,
#51330,#51331,#51332,#51333,#51334,#51335,#51336,#51337,#51338,#51339,#51340,
#51341),.UNSPECIFIED.,.F.,.F.,(4,3,3,3,3,3,3,3,3,3,3,3,3,3,3,3,3,3,3,3,
4),(7.31797006928123E-11,0.100715529220303,0.175357764610152,0.238678478425238,
0.25,0.301434000969269,0.351119460711998,0.400021887779728,0.450010943889864,
0.497472186324765,0.5,0.500001800462764,0.54755125219235,0.598163439144263,
0.647566149279604,0.698783074639802,0.75,0.81286007931633,0.88802726687967,
0.987428003542778,0.999999999992996),.UNSPECIFIED.);
#841=B_SPLINE_CURVE_WITH_KNOTS('',3,(#51424,#51425,#51426,#51427,#51428,
#51429,#51430,#51431,#51432,#51433,#51434,#51435,#51436,#51437,#51438,#51439,
#51440,#51441,#51442,#51443,#51444,#51445,#51446,#51447,#51448,#51449,#51450,
#51451,#51452,#51453,#51454,#51455,#51456,#51457,#51458,#51459,#51460,#51461,
#51462,#51463,#51464,#51465,#51466,#51467,#51468,#51469,#51470,#51471,#51472),
 .UNSPECIFIED.,.F.,.F.,(4,3,3,3,3,3,3,3,3,3,3,3,3,3,3,3,4),(0.,0.0772490783748716,
0.125628580660424,0.206837347558675,0.250000000000001,0.333280273269906,
0.368977328446765,0.374999999999999,0.423220960550615,0.471880842368208,
0.499999999999997,0.601986585180624,0.703425665210588,0.731721858235954,
0.83332819110189,0.936212051837402,1.),.UNSPECIFIED.);
#842=B_SPLINE_CURVE_WITH_KNOTS('',3,(#51473,#51474,#51475,#51476,#51477,
#51478,#51479,#51480,#51481,#51482,#51483,#51484,#51485,#51486,#51487,#51488,
#51489,#51490,#51491,#51492,#51493,#51494,#51495,#51496,#51497,#51498,#51499,
#51500,#51501,#51502,#51503,#51504,#51505,#51506,#51507,#51508,#51509,#51510,
#51511,#51512,#51513,#51514,#51515,#51516,#51517,#51518,#51519,#51520,#51521,
#51522,#51523,#51524),.UNSPECIFIED.,.F.,.F.,(4,3,3,3,3,3,3,3,3,3,3,3,3,
3,3,3,3,4),(0.,0.0673552999085671,0.136367280704923,0.208456935206561,0.250000000000025,
0.329907800933807,0.375000000000035,0.437500000000039,0.468750000000042,
0.484375000000041,0.495400419983993,0.50000000000004,0.586602629559447,
0.675549917512404,0.768876331728931,0.865001499097696,0.965889321645426,
1.),.UNSPECIFIED.);
#843=B_SPLINE_CURVE_WITH_KNOTS('',3,(#51565,#51566,#51567,#51568,#51569,
#51570,#51571,#51572,#51573,#51574,#51575,#51576,#51577,#51578,#51579,#51580,
#51581,#51582,#51583,#51584,#51585,#51586,#51587,#51588,#51589,#51590,#51591,
#51592,#51593,#51594,#51595,#51596,#51597,#51598,#51599,#51600,#51601,#51602,
#51603,#51604,#51605,#51606,#51607,#51608,#51609,#51610,#51611,#51612,#51613,
#51614,#51615,#51616,#51617,#51618,#51619,#51620,#51621,#51622,#51623,#51624,
#51625,#51626,#51627,#51628,#51629,#51630,#51631,#51632,#51633,#51634,#51635,
#51636,#51637,#51638,#51639,#51640,#51641,#51642,#51643),.UNSPECIFIED.,
 .F.,.F.,(4,3,3,3,3,3,3,3,3,3,3,3,3,3,3,3,3,3,3,3,3,3,3,3,3,3,4),(0.,0.0457033068802993,
0.0916137398494609,0.120395916002719,0.1428571428571,0.19727492470639,0.251652801985863,
0.275597882536144,0.2857142857143,0.349092790520194,0.412555793048888,0.4285714285714,
0.430653365734671,0.4960636773585,0.561515650793809,0.5714285714286,0.585415002992912,
0.649850358639306,0.7142857142857,0.740421620406485,0.795269363043043,0.850185630861512,
0.8571428571429,0.895775606041297,0.941868794237302,0.987755080875803,0.999999797081952),
 .UNSPECIFIED.);
#844=B_SPLINE_CURVE_WITH_KNOTS('',3,(#51735,#51736,#51737,#51738,#51739,
#51740,#51741,#51742,#51743,#51744,#51745,#51746,#51747,#51748,#51749,#51750,
#51751,#51752),.UNSPECIFIED.,.F.,.F.,(4,2,2,2,2,2,2,2,4),(0.,0.0151925643701926,
0.0303851287403852,0.045584296496648,0.0607834642529108,0.0759910091953897,
0.0911985541378687,0.106391953286869,0.121585352435869),.UNSPECIFIED.);
#845=B_SPLINE_CURVE_WITH_KNOTS('',3,(#51844,#51845,#51846,#51847,#51848,
#51849,#51850,#51851,#51852,#51853,#51854,#51855,#51856,#51857,#51858,#51859,
#51860,#51861),.UNSPECIFIED.,.F.,.F.,(4,2,2,2,2,2,2,2,4),(0.316667444606564,
0.395834141831916,0.475000839057267,0.554167864135198,0.633334889213128,
0.712501914291059,0.791668939368989,0.870835636594341,0.950002333819692),
 .UNSPECIFIED.);
#846=B_SPLINE_CURVE_WITH_KNOTS('',3,(#51863,#51864,#51865,#51866,#51867,
#51868,#51869,#51870,#51871,#51872),.UNSPECIFIED.,.F.,.F.,(4,2,2,2,4),(-1.26666977842626,
-1.18750275334833,-1.10833572827039,-1.02916903104504,-0.950002333819692),
 .UNSPECIFIED.);
#847=B_SPLINE_CURVE_WITH_KNOTS('',3,(#51873,#51874,#51875,#51876,#51877,
#51878,#51879,#51880,#51881,#51882),.UNSPECIFIED.,.F.,.F.,(4,2,2,2,4),(0.950002333819692,
1.02916903104504,1.1083357282704,1.18750275334833,1.26666977842626),
 .UNSPECIFIED.);
#848=B_SPLINE_CURVE_WITH_KNOTS('',3,(#51888,#51889,#51890,#51891,#51892,
#51893,#51894,#51895,#51896,#51897,#51898,#51899,#51900,#51901,#51902,#51903),
 .UNSPECIFIED.,.F.,.F.,(4,2,2,2,2,2,2,4),(-0.779979052988675,-0.757912790448093,
-0.703814302563526,-0.64971581467896,-0.595510917659987,-0.541306020641014,
-0.487185868025911,-0.433065715410808),.UNSPECIFIED.);
#849=B_SPLINE_CURVE_WITH_KNOTS('',3,(#52126,#52127,#52128,#52129,#52130,
#52131,#52132,#52133,#52134,#52135,#52136,#52137,#52138,#52139,#52140,#52141),
 .UNSPECIFIED.,.F.,.F.,(4,2,2,2,2,2,2,4),(0.43308109743951,0.487202501340474,
0.541323905241438,0.595534461493003,0.649745017744569,0.703843614398011,
0.757942211051454,0.780009479202147),.UNSPECIFIED.);
#850=B_SPLINE_CURVE_WITH_KNOTS('',3,(#52173,#52174,#52175,#52176,#52177,
#52178,#52179,#52180,#52181,#52182,#52183,#52184,#52185,#52186,#52187,#52188,
#52189,#52190),.UNSPECIFIED.,.F.,.F.,(4,2,2,2,2,2,2,2,4),(0.121587491028333,
0.136780909575281,0.151974328122229,0.167182628159423,0.182390928196617,
0.197590414964019,0.212789901731421,0.227982441894043,0.243174982056666),
 .UNSPECIFIED.);
#851=B_SPLINE_CURVE_WITH_KNOTS('',3,(#52270,#52271,#52272,#52273,#52274,
#52275,#52276,#52277,#52278,#52279,#52280,#52281,#52282,#52283,#52284,#52285,
#52286,#52287),.UNSPECIFIED.,.F.,.F.,(4,2,2,2,2,2,2,2,4),(0.,0.0151925643701926,
0.0303851287403852,0.045584296496648,0.0607834642529108,0.0759910091953897,
0.0911985541378687,0.106391953286869,0.121585352435869),.UNSPECIFIED.);
#852=B_SPLINE_CURVE_WITH_KNOTS('',3,(#52369,#52370,#52371,#52372,#52373,
#52374,#52375,#52376,#52377,#52378,#52379),.UNSPECIFIED.,.F.,.F.,(4,2,3,
2,4),(-0.15830486583654,-0.080247501535826,0.,0.0802475015358259,0.15830486583654),
 .UNSPECIFIED.);
#853=B_SPLINE_CURVE_WITH_KNOTS('',3,(#52384,#52385,#52386,#52387,#52388,
#52389,#52390,#52391,#52392,#52393),.UNSPECIFIED.,.F.,.F.,(4,2,2,2,4),(0.483273505725753,
0.561330870026467,0.641578371562293,0.721825873098119,0.799883237398833),
 .UNSPECIFIED.);
#854=B_SPLINE_CURVE_WITH_KNOTS('',3,(#52421,#52422,#52423,#52424,#52425,
#52426,#52427,#52428,#52429,#52430,#52431,#52432,#52433,#52434,#52435,#52436,
#52437,#52438),.UNSPECIFIED.,.F.,.F.,(4,2,2,2,2,2,2,2,4),(0.316667444606564,
0.395834141831916,0.475000839057267,0.554167864135198,0.633334889213128,
0.712501914291059,0.791668939368989,0.870835636594341,0.950002333819692),
 .UNSPECIFIED.);
#855=B_SPLINE_CURVE_WITH_KNOTS('',3,(#52440,#52441,#52442,#52443,#52444,
#52445,#52446,#52447,#52448,#52449),.UNSPECIFIED.,.F.,.F.,(4,2,2,2,4),(-1.26666977842626,
-1.18750275334833,-1.10833572827039,-1.02916903104504,-0.950002333819692),
 .UNSPECIFIED.);
#856=B_SPLINE_CURVE_WITH_KNOTS('',3,(#52450,#52451,#52452,#52453,#52454,
#52455,#52456,#52457,#52458,#52459),.UNSPECIFIED.,.F.,.F.,(4,2,2,2,4),(0.950002333819692,
1.02916903104504,1.1083357282704,1.18750275334833,1.26666977842626),
 .UNSPECIFIED.);
#857=B_SPLINE_CURVE_WITH_KNOTS('',3,(#52465,#52466,#52467,#52468,#52469,
#52470,#52471,#52472,#52473,#52474,#52475,#52476,#52477,#52478,#52479,#52480),
 .UNSPECIFIED.,.F.,.F.,(4,2,2,2,2,2,2,4),(-0.779979052988675,-0.757912790448093,
-0.703814302563526,-0.64971581467896,-0.595510917659987,-0.541306020641014,
-0.487185868025911,-0.433065715410808),.UNSPECIFIED.);
#858=B_SPLINE_CURVE_WITH_KNOTS('',3,(#52703,#52704,#52705,#52706,#52707,
#52708,#52709,#52710,#52711,#52712,#52713,#52714,#52715,#52716,#52717,#52718),
 .UNSPECIFIED.,.F.,.F.,(4,2,2,2,2,2,2,4),(0.43308109743951,0.487202501340474,
0.541323905241438,0.595534461493003,0.649745017744569,0.703843614398011,
0.757942211051454,0.780009479202147),.UNSPECIFIED.);
#859=B_SPLINE_CURVE_WITH_KNOTS('',3,(#52750,#52751,#52752,#52753,#52754,
#52755,#52756,#52757,#52758,#52759,#52760,#52761,#52762,#52763,#52764,#52765,
#52766,#52767),.UNSPECIFIED.,.F.,.F.,(4,2,2,2,2,2,2,2,4),(0.121587491028333,
0.136780909575281,0.151974328122229,0.167182628159423,0.182390928196617,
0.197590414964019,0.212789901731421,0.227982441894043,0.243174982056666),
 .UNSPECIFIED.);
#860=B_SPLINE_CURVE_WITH_KNOTS('',3,(#54162,#54163,#54164,#54165,#54166,
#54167,#54168,#54169,#54170,#54171),.UNSPECIFIED.,.F.,.F.,(4,2,2,2,4),(-0.991617660219933,
-0.988360888345703,-0.882558915285875,-0.776756942226048,-0.773500170351817),
 .UNSPECIFIED.);
#861=B_SPLINE_CURVE_WITH_KNOTS('',3,(#54173,#54174,#54175,#54176,#54177,
#54178,#54179,#54180,#54181,#54182),.UNSPECIFIED.,.F.,.F.,(4,2,2,2,4),(-0.991617660219933,
-0.988360888345703,-0.882558915285875,-0.776756942226048,-0.773500170351817),
 .UNSPECIFIED.);
#862=B_SPLINE_CURVE_WITH_KNOTS('',3,(#54184,#54185,#54186,#54187,#54188,
#54189,#54190,#54191,#54192,#54193),.UNSPECIFIED.,.F.,.F.,(4,2,2,2,4),(-0.991617660219934,
-0.988360888345704,-0.882558915285876,-0.776756942226048,-0.773500170351818),
 .UNSPECIFIED.);
#863=B_SPLINE_CURVE_WITH_KNOTS('',3,(#54202,#54203,#54204,#54205,#54206,
#54207,#54208,#54209,#54210,#54211),.UNSPECIFIED.,.F.,.F.,(4,2,2,2,4),(0.773500170351818,
0.776756942226048,0.882558915285876,0.988360888345703,0.991617660219934),
 .UNSPECIFIED.);
#864=B_SPLINE_CURVE_WITH_KNOTS('',3,(#54213,#54214,#54215,#54216,#54217,
#54218,#54219,#54220,#54221,#54222),.UNSPECIFIED.,.F.,.F.,(4,2,2,2,4),(0.773500170351817,
0.776756942226048,0.882558915285875,0.988360888345703,0.991617660219933),
 .UNSPECIFIED.);
#865=B_SPLINE_CURVE_WITH_KNOTS('',3,(#54223,#54224,#54225,#54226,#54227,
#54228,#54229,#54230,#54231,#54232),.UNSPECIFIED.,.F.,.F.,(4,2,2,2,4),(0.773500170351818,
0.776756942226048,0.882558915285876,0.988360888345704,0.991617660219934),
 .UNSPECIFIED.);
#866=B_SPLINE_CURVE_WITH_KNOTS('',3,(#56130,#56131,#56132,#56133,#56134,
#56135,#56136,#56137,#56138,#56139),.UNSPECIFIED.,.F.,.F.,(4,2,2,2,4),(0.112312904835896,
0.113244103065848,0.226488206131697,0.343893756973101,0.461299307814506),
 .UNSPECIFIED.);
#867=B_SPLINE_CURVE_WITH_KNOTS('',3,(#56143,#56144,#56145,#56146,#56147,
#56148,#56149,#56150,#56151,#56152),.UNSPECIFIED.,.F.,.F.,(4,2,2,2,4),(0.461299307814506,
0.57870485865591,0.696110409497315,0.809354512563163,0.810285710793116),
 .UNSPECIFIED.);
#868=SHAPE_REPRESENTATION_RELATIONSHIP('SRR','None',#57250,#897);
#869=SHAPE_REPRESENTATION_RELATIONSHIP('SRR','None',#57253,#898);
#870=SHAPE_REPRESENTATION_RELATIONSHIP('SRR','None',#57254,#899);
#871=SHAPE_REPRESENTATION_RELATIONSHIP('SRR','None',#57256,#900);
#872=SHAPE_REPRESENTATION_RELATIONSHIP('SRR','None',#57257,#901);
#873=SHAPE_REPRESENTATION_RELATIONSHIP('SRR','None',#57258,#902);
#874=SHAPE_REPRESENTATION_RELATIONSHIP('SRR','None',#57260,#903);
#875=SHAPE_REPRESENTATION_RELATIONSHIP('SRR','None',#57261,#904);
#876=SHAPE_REPRESENTATION_RELATIONSHIP('SRR','None',#57262,#905);
#877=SHAPE_REPRESENTATION_RELATIONSHIP('SRR','None',#57263,#906);
#878=SHAPE_REPRESENTATION_RELATIONSHIP('SRR','None',#57264,#907);
#879=SHAPE_REPRESENTATION_RELATIONSHIP('SRR','None',#57267,#908);
#880=SHAPE_REPRESENTATION_RELATIONSHIP('SRR','None',#57268,#909);
#881=SHAPE_REPRESENTATION_RELATIONSHIP('SRR','None',#57269,#910);
#882=SHAPE_REPRESENTATION_RELATIONSHIP('SRR','None',#57270,#911);
#883=SHAPE_REPRESENTATION_RELATIONSHIP('SRR','None',#57271,#912);
#884=SHAPE_REPRESENTATION_RELATIONSHIP('SRR','None',#57273,#913);
#885=SHAPE_REPRESENTATION_RELATIONSHIP('SRR','None',#57274,#914);
#886=SHAPE_REPRESENTATION_RELATIONSHIP('SRR','None',#57275,#915);
#887=SHAPE_REPRESENTATION_RELATIONSHIP('SRR','None',#57276,#916);
#888=SHAPE_REPRESENTATION_RELATIONSHIP('SRR','None',#57278,#917);
#889=SHAPE_REPRESENTATION_RELATIONSHIP('SRR','None',#57279,#918);
#890=SHAPE_REPRESENTATION_RELATIONSHIP('SRR','None',#57280,#919);
#891=SHAPE_REPRESENTATION_RELATIONSHIP('SRR','None',#57281,#920);
#892=SHAPE_REPRESENTATION_RELATIONSHIP('SRR','None',#57282,#921);
#893=SHAPE_REPRESENTATION_RELATIONSHIP('SRR','None',#57283,#922);
#894=SHAPE_REPRESENTATION_RELATIONSHIP('SRR','None',#57284,#923);
#895=SHAPE_REPRESENTATION_RELATIONSHIP('SRR','None',#57285,#924);
#896=SHAPE_REPRESENTATION_RELATIONSHIP('SRR','None',#57286,#925);
#897=ADVANCED_BREP_SHAPE_REPRESENTATION('',(#963),#57042);
#898=ADVANCED_BREP_SHAPE_REPRESENTATION('',(#964),#57045);
#899=ADVANCED_BREP_SHAPE_REPRESENTATION('',(#965),#57046);
#900=ADVANCED_BREP_SHAPE_REPRESENTATION('',(#966),#57048);
#901=ADVANCED_BREP_SHAPE_REPRESENTATION('',(#967,#968),#57049);
#902=ADVANCED_BREP_SHAPE_REPRESENTATION('',(#969),#57050);
#903=ADVANCED_BREP_SHAPE_REPRESENTATION('',(#970,#971),#57052);
#904=ADVANCED_BREP_SHAPE_REPRESENTATION('',(#972),#57053);
#905=ADVANCED_BREP_SHAPE_REPRESENTATION('',(#973),#57054);
#906=ADVANCED_BREP_SHAPE_REPRESENTATION('',(#974),#57055);
#907=ADVANCED_BREP_SHAPE_REPRESENTATION('',(#975),#57056);
#908=ADVANCED_BREP_SHAPE_REPRESENTATION('',(#976),#57059);
#909=ADVANCED_BREP_SHAPE_REPRESENTATION('',(#977),#57060);
#910=ADVANCED_BREP_SHAPE_REPRESENTATION('',(#978),#57061);
#911=ADVANCED_BREP_SHAPE_REPRESENTATION('',(#979),#57062);
#912=ADVANCED_BREP_SHAPE_REPRESENTATION('',(#980),#57063);
#913=ADVANCED_BREP_SHAPE_REPRESENTATION('',(#981),#57065);
#914=ADVANCED_BREP_SHAPE_REPRESENTATION('',(#982),#57066);
#915=ADVANCED_BREP_SHAPE_REPRESENTATION('',(#983),#57067);
#916=ADVANCED_BREP_SHAPE_REPRESENTATION('',(#984,#985,#986),#57068);
#917=ADVANCED_BREP_SHAPE_REPRESENTATION('',(#987),#57070);
#918=ADVANCED_BREP_SHAPE_REPRESENTATION('',(#988),#57071);
#919=ADVANCED_BREP_SHAPE_REPRESENTATION('',(#989),#57072);
#920=ADVANCED_BREP_SHAPE_REPRESENTATION('',(#990),#57073);
#921=ADVANCED_BREP_SHAPE_REPRESENTATION('',(#991,#992,#993),#57074);
#922=ADVANCED_BREP_SHAPE_REPRESENTATION('',(#994),#57075);
#923=ADVANCED_BREP_SHAPE_REPRESENTATION('',(#995,#996,#997),#57076);
#924=ADVANCED_BREP_SHAPE_REPRESENTATION('',(#998),#57077);
#925=ADVANCED_BREP_SHAPE_REPRESENTATION('',(#999),#57078);
#926=STYLED_ITEM('',(#57444),#963);
#927=STYLED_ITEM('',(#57444),#964);
#928=STYLED_ITEM('',(#57444),#965);
#929=STYLED_ITEM('',(#57444),#966);
#930=STYLED_ITEM('',(#57444),#967);
#931=STYLED_ITEM('',(#57444),#968);
#932=STYLED_ITEM('',(#57444),#969);
#933=STYLED_ITEM('',(#57444),#970);
#934=STYLED_ITEM('',(#57444),#971);
#935=STYLED_ITEM('',(#57444),#972);
#936=STYLED_ITEM('',(#57444),#973);
#937=STYLED_ITEM('',(#57444),#974);
#938=STYLED_ITEM('',(#57444),#975);
#939=STYLED_ITEM('',(#57444),#976);
#940=STYLED_ITEM('',(#57444),#977);
#941=STYLED_ITEM('',(#57444),#978);
#942=STYLED_ITEM('',(#57444),#979);
#943=STYLED_ITEM('',(#57444),#980);
#944=STYLED_ITEM('',(#57444),#981);
#945=STYLED_ITEM('',(#57444),#982);
#946=STYLED_ITEM('',(#57444),#983);
#947=STYLED_ITEM('',(#57444),#984);
#948=STYLED_ITEM('',(#57444),#985);
#949=STYLED_ITEM('',(#57444),#986);
#950=STYLED_ITEM('',(#57444),#987);
#951=STYLED_ITEM('',(#57444),#988);
#952=STYLED_ITEM('',(#57444),#989);
#953=STYLED_ITEM('',(#57444),#990);
#954=STYLED_ITEM('',(#57444),#991);
#955=STYLED_ITEM('',(#57444),#992);
#956=STYLED_ITEM('',(#57444),#993);
#957=STYLED_ITEM('',(#57444),#994);
#958=STYLED_ITEM('',(#57444),#995);
#959=STYLED_ITEM('',(#57444),#996);
#960=STYLED_ITEM('',(#57444),#997);
#961=STYLED_ITEM('',(#57444),#998);
#962=STYLED_ITEM('',(#57444),#999);
#963=MANIFOLD_SOLID_BREP('Body1',#24526);
#964=MANIFOLD_SOLID_BREP('Body1',#24527);
#965=MANIFOLD_SOLID_BREP('Body1',#24528);
#966=MANIFOLD_SOLID_BREP('Body1',#24529);
#967=MANIFOLD_SOLID_BREP('Body1',#24530);
#968=MANIFOLD_SOLID_BREP('Body2',#24531);
#969=MANIFOLD_SOLID_BREP('Body1',#24532);
#970=MANIFOLD_SOLID_BREP('Body1',#24533);
#971=MANIFOLD_SOLID_BREP('Body2',#24534);
#972=MANIFOLD_SOLID_BREP('Body1',#24535);
#973=MANIFOLD_SOLID_BREP('Body1',#24536);
#974=MANIFOLD_SOLID_BREP('Body1',#24537);
#975=MANIFOLD_SOLID_BREP('Body1',#24538);
#976=MANIFOLD_SOLID_BREP('Body1',#24539);
#977=MANIFOLD_SOLID_BREP('Body1',#24540);
#978=MANIFOLD_SOLID_BREP('Body1',#24541);
#979=MANIFOLD_SOLID_BREP('Body1',#24542);
#980=MANIFOLD_SOLID_BREP('Body1',#24543);
#981=MANIFOLD_SOLID_BREP('Body1',#24544);
#982=MANIFOLD_SOLID_BREP('Body1',#24545);
#983=MANIFOLD_SOLID_BREP('Body1',#24546);
#984=MANIFOLD_SOLID_BREP('Body1',#24547);
#985=MANIFOLD_SOLID_BREP('Body2',#24548);
#986=MANIFOLD_SOLID_BREP('Body3',#24549);
#987=MANIFOLD_SOLID_BREP('Body1',#24550);
#988=MANIFOLD_SOLID_BREP('Body1',#24551);
#989=MANIFOLD_SOLID_BREP('Body1',#24552);
#990=MANIFOLD_SOLID_BREP('Body1',#24553);
#991=MANIFOLD_SOLID_BREP('Body1',#24554);
#992=MANIFOLD_SOLID_BREP('Body2',#24555);
#993=MANIFOLD_SOLID_BREP('Body3',#24556);
#994=MANIFOLD_SOLID_BREP('Body1',#24557);
#995=MANIFOLD_SOLID_BREP('Body1',#24558);
#996=MANIFOLD_SOLID_BREP('Body2',#24559);
#997=MANIFOLD_SOLID_BREP('Body3',#24560);
#998=MANIFOLD_SOLID_BREP('Body1',#24561);
#999=MANIFOLD_SOLID_BREP('Body1',#24562);
#1000=FACE_BOUND('',#3553,.T.);
#1001=FACE_BOUND('',#3554,.T.);
#1002=FACE_BOUND('',#3555,.T.);
#1003=FACE_BOUND('',#3556,.T.);
#1004=FACE_BOUND('',#3560,.T.);
#1005=FACE_BOUND('',#3561,.T.);
#1006=FACE_BOUND('',#3562,.T.);
#1007=FACE_BOUND('',#3563,.T.);
#1008=FACE_BOUND('',#3564,.T.);
#1009=FACE_BOUND('',#3565,.T.);
#1010=FACE_BOUND('',#3566,.T.);
#1011=FACE_BOUND('',#3567,.T.);
#1012=FACE_BOUND('',#3569,.T.);
#1013=FACE_BOUND('',#3570,.T.);
#1014=FACE_BOUND('',#3571,.T.);
#1015=FACE_BOUND('',#3572,.T.);
#1016=FACE_BOUND('',#3573,.T.);
#1017=FACE_BOUND('',#3574,.T.);
#1018=FACE_BOUND('',#3575,.T.);
#1019=FACE_BOUND('',#3576,.T.);
#1020=FACE_BOUND('',#3594,.T.);
#1021=FACE_BOUND('',#3596,.T.);
#1022=FACE_BOUND('',#3598,.T.);
#1023=FACE_BOUND('',#3600,.T.);
#1024=FACE_BOUND('',#3602,.T.);
#1025=FACE_BOUND('',#3621,.T.);
#1026=FACE_BOUND('',#3626,.T.);
#1027=FACE_BOUND('',#3627,.T.);
#1028=FACE_BOUND('',#3628,.T.);
#1029=FACE_BOUND('',#3629,.T.);
#1030=FACE_BOUND('',#3630,.T.);
#1031=FACE_BOUND('',#3631,.T.);
#1032=FACE_BOUND('',#3632,.T.);
#1033=FACE_BOUND('',#3636,.T.);
#1034=FACE_BOUND('',#3641,.T.);
#1035=FACE_BOUND('',#3642,.T.);
#1036=FACE_BOUND('',#3643,.T.);
#1037=FACE_BOUND('',#3644,.T.);
#1038=FACE_BOUND('',#3645,.T.);
#1039=FACE_BOUND('',#3646,.T.);
#1040=FACE_BOUND('',#3647,.T.);
#1041=FACE_BOUND('',#3649,.T.);
#1042=FACE_BOUND('',#3651,.T.);
#1043=FACE_BOUND('',#3653,.T.);
#1044=FACE_BOUND('',#3655,.T.);
#1045=FACE_BOUND('',#3657,.T.);
#1046=FACE_BOUND('',#3680,.T.);
#1047=FACE_BOUND('',#3682,.T.);
#1048=FACE_BOUND('',#3684,.T.);
#1049=FACE_BOUND('',#3686,.T.);
#1050=FACE_BOUND('',#3688,.T.);
#1051=FACE_BOUND('',#3690,.T.);
#1052=FACE_BOUND('',#3694,.T.);
#1053=FACE_BOUND('',#3695,.T.);
#1054=FACE_BOUND('',#3699,.T.);
#1055=FACE_BOUND('',#3706,.T.);
#1056=FACE_BOUND('',#3708,.T.);
#1057=FACE_BOUND('',#3709,.T.);
#1058=FACE_BOUND('',#3710,.T.);
#1059=FACE_BOUND('',#3711,.T.);
#1060=FACE_BOUND('',#3712,.T.);
#1061=FACE_BOUND('',#3722,.T.);
#1062=FACE_BOUND('',#3724,.T.);
#1063=FACE_BOUND('',#3726,.T.);
#1064=FACE_BOUND('',#3728,.T.);
#1065=FACE_BOUND('',#3778,.T.);
#1066=FACE_BOUND('',#3780,.T.);
#1067=FACE_BOUND('',#3782,.T.);
#1068=FACE_BOUND('',#3784,.T.);
#1069=FACE_BOUND('',#3789,.T.);
#1070=FACE_BOUND('',#3795,.T.);
#1071=FACE_BOUND('',#3797,.T.);
#1072=FACE_BOUND('',#3799,.T.);
#1073=FACE_BOUND('',#3801,.T.);
#1074=FACE_BOUND('',#3811,.T.);
#1075=FACE_BOUND('',#3822,.T.);
#1076=FACE_BOUND('',#3824,.T.);
#1077=FACE_BOUND('',#3829,.T.);
#1078=FACE_BOUND('',#3831,.T.);
#1079=FACE_BOUND('',#3833,.T.);
#1080=FACE_BOUND('',#3837,.T.);
#1081=FACE_BOUND('',#3838,.T.);
#1082=FACE_BOUND('',#3842,.T.);
#1083=FACE_BOUND('',#3859,.T.);
#1084=FACE_BOUND('',#3861,.T.);
#1085=FACE_BOUND('',#3863,.T.);
#1086=FACE_BOUND('',#3865,.T.);
#1087=FACE_BOUND('',#3867,.T.);
#1088=FACE_BOUND('',#3869,.T.);
#1089=FACE_BOUND('',#3875,.T.);
#1090=FACE_BOUND('',#3876,.T.);
#1091=FACE_BOUND('',#3878,.T.);
#1092=FACE_BOUND('',#3879,.T.);
#1093=FACE_BOUND('',#3901,.T.);
#1094=FACE_BOUND('',#3902,.T.);
#1095=FACE_BOUND('',#3903,.T.);
#1096=FACE_BOUND('',#3904,.T.);
#1097=FACE_BOUND('',#3910,.T.);
#1098=FACE_BOUND('',#3911,.T.);
#1099=FACE_BOUND('',#3912,.T.);
#1100=FACE_BOUND('',#3913,.T.);
#1101=FACE_BOUND('',#3925,.T.);
#1102=FACE_BOUND('',#3926,.T.);
#1103=FACE_BOUND('',#3927,.T.);
#1104=FACE_BOUND('',#3928,.T.);
#1105=FACE_BOUND('',#3934,.T.);
#1106=FACE_BOUND('',#3935,.T.);
#1107=FACE_BOUND('',#3936,.T.);
#1108=FACE_BOUND('',#3937,.T.);
#1109=FACE_BOUND('',#3951,.T.);
#1110=FACE_BOUND('',#3952,.T.);
#1111=FACE_BOUND('',#3953,.T.);
#1112=FACE_BOUND('',#3954,.T.);
#1113=FACE_BOUND('',#3955,.T.);
#1114=FACE_BOUND('',#3956,.T.);
#1115=FACE_BOUND('',#3957,.T.);
#1116=FACE_BOUND('',#3958,.T.);
#1117=FACE_BOUND('',#3959,.T.);
#1118=FACE_BOUND('',#3965,.T.);
#1119=FACE_BOUND('',#3966,.T.);
#1120=FACE_BOUND('',#3967,.T.);
#1121=FACE_BOUND('',#3968,.T.);
#1122=FACE_BOUND('',#3969,.T.);
#1123=FACE_BOUND('',#3970,.T.);
#1124=FACE_BOUND('',#3971,.T.);
#1125=FACE_BOUND('',#3972,.T.);
#1126=FACE_BOUND('',#3973,.T.);
#1127=FACE_BOUND('',#3975,.T.);
#1128=FACE_BOUND('',#3977,.T.);
#1129=FACE_BOUND('',#3979,.T.);
#1130=FACE_BOUND('',#4115,.T.);
#1131=FACE_BOUND('',#4116,.T.);
#1132=FACE_BOUND('',#4117,.T.);
#1133=FACE_BOUND('',#4118,.T.);
#1134=FACE_BOUND('',#4131,.T.);
#1135=FACE_BOUND('',#4132,.T.);
#1136=FACE_BOUND('',#4133,.T.);
#1137=FACE_BOUND('',#4134,.T.);
#1138=FACE_BOUND('',#4136,.T.);
#1139=FACE_BOUND('',#4148,.T.);
#1140=FACE_BOUND('',#4160,.T.);
#1141=FACE_BOUND('',#4166,.T.);
#1142=FACE_BOUND('',#4171,.T.);
#1143=FACE_BOUND('',#4172,.T.);
#1144=FACE_BOUND('',#4173,.T.);
#1145=FACE_BOUND('',#4174,.T.);
#1146=FACE_BOUND('',#4175,.T.);
#1147=FACE_BOUND('',#4225,.T.);
#1148=FACE_BOUND('',#4227,.T.);
#1149=FACE_BOUND('',#4239,.T.);
#1150=FACE_BOUND('',#4251,.T.);
#1151=FACE_BOUND('',#4264,.T.);
#1152=FACE_BOUND('',#4265,.T.);
#1153=FACE_BOUND('',#4266,.T.);
#1154=FACE_BOUND('',#4267,.T.);
#1155=FACE_BOUND('',#4268,.T.);
#1156=FACE_BOUND('',#4318,.T.);
#1157=FACE_BOUND('',#4327,.T.);
#1158=FACE_BOUND('',#4328,.T.);
#1159=FACE_BOUND('',#4329,.T.);
#1160=FACE_BOUND('',#4330,.T.);
#1161=FACE_BOUND('',#4331,.T.);
#1162=FACE_BOUND('',#4332,.T.);
#1163=FACE_BOUND('',#4333,.T.);
#1164=FACE_BOUND('',#4336,.T.);
#1165=FACE_BOUND('',#4337,.T.);
#1166=FACE_BOUND('',#4338,.T.);
#1167=FACE_BOUND('',#4339,.T.);
#1168=FACE_BOUND('',#4340,.T.);
#1169=FACE_BOUND('',#4341,.T.);
#1170=FACE_BOUND('',#4342,.T.);
#1171=FACE_BOUND('',#4359,.T.);
#1172=FACE_BOUND('',#4360,.T.);
#1173=FACE_BOUND('',#4361,.T.);
#1174=FACE_BOUND('',#4362,.T.);
#1175=FACE_BOUND('',#4363,.T.);
#1176=FACE_BOUND('',#4364,.T.);
#1177=FACE_BOUND('',#4366,.T.);
#1178=FACE_BOUND('',#4367,.T.);
#1179=FACE_BOUND('',#4368,.T.);
#1180=FACE_BOUND('',#4369,.T.);
#1181=FACE_BOUND('',#4370,.T.);
#1182=FACE_BOUND('',#4371,.T.);
#1183=FACE_BOUND('',#4383,.T.);
#1184=FACE_BOUND('',#4384,.T.);
#1185=FACE_BOUND('',#4385,.T.);
#1186=FACE_BOUND('',#4386,.T.);
#1187=FACE_BOUND('',#4387,.T.);
#1188=FACE_BOUND('',#4388,.T.);
#1189=FACE_BOUND('',#4390,.T.);
#1190=FACE_BOUND('',#4391,.T.);
#1191=FACE_BOUND('',#4392,.T.);
#1192=FACE_BOUND('',#4393,.T.);
#1193=FACE_BOUND('',#4394,.T.);
#1194=FACE_BOUND('',#4395,.T.);
#1195=FACE_BOUND('',#4460,.T.);
#1196=FACE_BOUND('',#4461,.T.);
#1197=FACE_BOUND('',#4462,.T.);
#1198=FACE_BOUND('',#4463,.T.);
#1199=FACE_BOUND('',#4464,.T.);
#1200=FACE_BOUND('',#4465,.T.);
#1201=FACE_BOUND('',#4466,.T.);
#1202=FACE_BOUND('',#4467,.T.);
#1203=FACE_BOUND('',#4468,.T.);
#1204=FACE_BOUND('',#4469,.T.);
#1205=FACE_BOUND('',#4470,.T.);
#1206=FACE_BOUND('',#4471,.T.);
#1207=FACE_BOUND('',#4472,.T.);
#1208=FACE_BOUND('',#4473,.T.);
#1209=FACE_BOUND('',#4474,.T.);
#1210=FACE_BOUND('',#4475,.T.);
#1211=FACE_BOUND('',#4476,.T.);
#1212=FACE_BOUND('',#4477,.T.);
#1213=FACE_BOUND('',#4478,.T.);
#1214=FACE_BOUND('',#4479,.T.);
#1215=FACE_BOUND('',#4480,.T.);
#1216=FACE_BOUND('',#4481,.T.);
#1217=FACE_BOUND('',#4486,.T.);
#1218=FACE_BOUND('',#4487,.T.);
#1219=FACE_BOUND('',#4488,.T.);
#1220=FACE_BOUND('',#4489,.T.);
#1221=FACE_BOUND('',#4490,.T.);
#1222=FACE_BOUND('',#4491,.T.);
#1223=FACE_BOUND('',#4492,.T.);
#1224=FACE_BOUND('',#4493,.T.);
#1225=FACE_BOUND('',#4494,.T.);
#1226=FACE_BOUND('',#4495,.T.);
#1227=FACE_BOUND('',#4497,.T.);
#1228=FACE_BOUND('',#4498,.T.);
#1229=FACE_BOUND('',#4499,.T.);
#1230=FACE_BOUND('',#4500,.T.);
#1231=FACE_BOUND('',#4501,.T.);
#1232=FACE_BOUND('',#4502,.T.);
#1233=FACE_BOUND('',#4503,.T.);
#1234=FACE_BOUND('',#4504,.T.);
#1235=FACE_BOUND('',#4505,.T.);
#1236=FACE_BOUND('',#4506,.T.);
#1237=FACE_BOUND('',#4508,.T.);
#1238=FACE_BOUND('',#4509,.T.);
#1239=FACE_BOUND('',#4510,.T.);
#1240=FACE_BOUND('',#4511,.T.);
#1241=FACE_BOUND('',#4512,.T.);
#1242=FACE_BOUND('',#4513,.T.);
#1243=FACE_BOUND('',#4514,.T.);
#1244=FACE_BOUND('',#4515,.T.);
#1245=FACE_BOUND('',#4516,.T.);
#1246=FACE_BOUND('',#4517,.T.);
#1247=FACE_BOUND('',#4518,.T.);
#1248=FACE_BOUND('',#4519,.T.);
#1249=FACE_BOUND('',#4520,.T.);
#1250=FACE_BOUND('',#4521,.T.);
#1251=FACE_BOUND('',#4522,.T.);
#1252=FACE_BOUND('',#4523,.T.);
#1253=FACE_BOUND('',#4524,.T.);
#1254=FACE_BOUND('',#4525,.T.);
#1255=FACE_BOUND('',#4526,.T.);
#1256=FACE_BOUND('',#4527,.T.);
#1257=FACE_BOUND('',#4528,.T.);
#1258=FACE_BOUND('',#4529,.T.);
#1259=FACE_BOUND('',#4530,.T.);
#1260=FACE_BOUND('',#4536,.T.);
#1261=FACE_BOUND('',#4538,.T.);
#1262=FACE_BOUND('',#4540,.T.);
#1263=FACE_BOUND('',#4542,.T.);
#1264=FACE_BOUND('',#4544,.T.);
#1265=FACE_BOUND('',#4546,.T.);
#1266=FACE_BOUND('',#4548,.T.);
#1267=FACE_BOUND('',#4550,.T.);
#1268=FACE_BOUND('',#4552,.T.);
#1269=FACE_BOUND('',#4554,.T.);
#1270=FACE_BOUND('',#4556,.T.);
#1271=FACE_BOUND('',#4558,.T.);
#1272=FACE_BOUND('',#4560,.T.);
#1273=FACE_BOUND('',#4562,.T.);
#1274=FACE_BOUND('',#4564,.T.);
#1275=FACE_BOUND('',#4566,.T.);
#1276=FACE_BOUND('',#4568,.T.);
#1277=FACE_BOUND('',#4629,.T.);
#1278=FACE_BOUND('',#4630,.T.);
#1279=FACE_BOUND('',#4631,.T.);
#1280=FACE_BOUND('',#4632,.T.);
#1281=FACE_BOUND('',#4633,.T.);
#1282=FACE_BOUND('',#4634,.T.);
#1283=FACE_BOUND('',#4635,.T.);
#1284=FACE_BOUND('',#4636,.T.);
#1285=FACE_BOUND('',#4675,.T.);
#1286=FACE_BOUND('',#4677,.T.);
#1287=FACE_BOUND('',#4679,.T.);
#1288=FACE_BOUND('',#4681,.T.);
#1289=FACE_BOUND('',#4683,.T.);
#1290=FACE_BOUND('',#4685,.T.);
#1291=FACE_BOUND('',#4687,.T.);
#1292=FACE_BOUND('',#4689,.T.);
#1293=FACE_BOUND('',#4751,.T.);
#1294=FACE_BOUND('',#4754,.T.);
#1295=FACE_BOUND('',#4769,.T.);
#1296=FACE_BOUND('',#4867,.T.);
#1297=FACE_BOUND('',#4880,.T.);
#1298=FACE_BOUND('',#4888,.T.);
#1299=FACE_BOUND('',#4891,.T.);
#1300=FACE_BOUND('',#4896,.T.);
#1301=FACE_BOUND('',#4944,.T.);
#1302=FACE_BOUND('',#4949,.T.);
#1303=FACE_BOUND('',#4951,.T.);
#1304=FACE_BOUND('',#4958,.T.);
#1305=FACE_BOUND('',#4959,.T.);
#1306=FACE_BOUND('',#4968,.T.);
#1307=FACE_BOUND('',#4969,.T.);
#1308=FACE_BOUND('',#4975,.T.);
#1309=FACE_BOUND('',#4981,.T.);
#1310=FACE_BOUND('',#4988,.T.);
#1311=FACE_BOUND('',#4993,.T.);
#1312=FACE_BOUND('',#5028,.T.);
#1313=FACE_BOUND('',#5040,.T.);
#1314=FACE_BOUND('',#5042,.T.);
#1315=FACE_BOUND('',#5061,.T.);
#1316=FACE_BOUND('',#5063,.T.);
#1317=FACE_BOUND('',#5094,.T.);
#1318=FACE_BOUND('',#5120,.T.);
#1319=FACE_BOUND('',#5121,.T.);
#1320=FACE_BOUND('',#5122,.T.);
#1321=FACE_BOUND('',#5123,.T.);
#1322=FACE_BOUND('',#5124,.T.);
#1323=FACE_BOUND('',#5125,.T.);
#1324=FACE_BOUND('',#5126,.T.);
#1325=FACE_BOUND('',#5127,.T.);
#1326=FACE_BOUND('',#5137,.T.);
#1327=FACE_BOUND('',#5140,.T.);
#1328=FACE_BOUND('',#5142,.T.);
#1329=FACE_BOUND('',#5158,.T.);
#1330=FACE_BOUND('',#5160,.T.);
#1331=FACE_BOUND('',#5173,.T.);
#1332=FACE_BOUND('',#5175,.T.);
#1333=FACE_BOUND('',#5189,.T.);
#1334=FACE_BOUND('',#5192,.T.);
#1335=FACE_BOUND('',#5194,.T.);
#1336=FACE_BOUND('',#5210,.T.);
#1337=FACE_BOUND('',#5212,.T.);
#1338=FACE_BOUND('',#5225,.T.);
#1339=FACE_BOUND('',#5227,.T.);
#1340=FACE_BOUND('',#5241,.T.);
#1341=FACE_BOUND('',#5243,.T.);
#1342=PLANE('',#24925);
#1343=PLANE('',#24926);
#1344=PLANE('',#24927);
#1345=PLANE('',#24928);
#1346=PLANE('',#24929);
#1347=PLANE('',#24930);
#1348=PLANE('',#24931);
#1349=PLANE('',#24932);
#1350=PLANE('',#24933);
#1351=PLANE('',#24934);
#1352=PLANE('',#24976);
#1353=PLANE('',#24977);
#1354=PLANE('',#24978);
#1355=PLANE('',#24979);
#1356=PLANE('',#24980);
#1357=PLANE('',#24983);
#1358=PLANE('',#24984);
#1359=PLANE('',#24985);
#1360=PLANE('',#24986);
#1361=PLANE('',#24987);
#1362=PLANE('',#25031);
#1363=PLANE('',#25046);
#1364=PLANE('',#25047);
#1365=PLANE('',#25048);
#1366=PLANE('',#25049);
#1367=PLANE('',#25050);
#1368=PLANE('',#25051);
#1369=PLANE('',#25052);
#1370=PLANE('',#25053);
#1371=PLANE('',#25131);
#1372=PLANE('',#25132);
#1373=PLANE('',#25133);
#1374=PLANE('',#25134);
#1375=PLANE('',#25135);
#1376=PLANE('',#25136);
#1377=PLANE('',#25137);
#1378=PLANE('',#25138);
#1379=PLANE('',#25139);
#1380=PLANE('',#25140);
#1381=PLANE('',#25141);
#1382=PLANE('',#25142);
#1383=PLANE('',#25143);
#1384=PLANE('',#25144);
#1385=PLANE('',#25145);
#1386=PLANE('',#25146);
#1387=PLANE('',#25147);
#1388=PLANE('',#25148);
#1389=PLANE('',#25149);
#1390=PLANE('',#25150);
#1391=PLANE('',#25151);
#1392=PLANE('',#25152);
#1393=PLANE('',#25153);
#1394=PLANE('',#25154);
#1395=PLANE('',#25155);
#1396=PLANE('',#25156);
#1397=PLANE('',#25157);
#1398=PLANE('',#25158);
#1399=PLANE('',#25159);
#1400=PLANE('',#25160);
#1401=PLANE('',#25161);
#1402=PLANE('',#25162);
#1403=PLANE('',#25163);
#1404=PLANE('',#25164);
#1405=PLANE('',#25165);
#1406=PLANE('',#25166);
#1407=PLANE('',#25167);
#1408=PLANE('',#25168);
#1409=PLANE('',#25169);
#1410=PLANE('',#25170);
#1411=PLANE('',#25171);
#1412=PLANE('',#25172);
#1413=PLANE('',#25173);
#1414=PLANE('',#25174);
#1415=PLANE('',#25175);
#1416=PLANE('',#25176);
#1417=PLANE('',#25177);
#1418=PLANE('',#25178);
#1419=PLANE('',#25179);
#1420=PLANE('',#25180);
#1421=PLANE('',#25181);
#1422=PLANE('',#25182);
#1423=PLANE('',#25183);
#1424=PLANE('',#25184);
#1425=PLANE('',#25185);
#1426=PLANE('',#25186);
#1427=PLANE('',#25187);
#1428=PLANE('',#25188);
#1429=PLANE('',#25189);
#1430=PLANE('',#25190);
#1431=PLANE('',#25191);
#1432=PLANE('',#25192);
#1433=PLANE('',#25193);
#1434=PLANE('',#25194);
#1435=PLANE('',#25195);
#1436=PLANE('',#25196);
#1437=PLANE('',#25197);
#1438=PLANE('',#25198);
#1439=PLANE('',#25199);
#1440=PLANE('',#25200);
#1441=PLANE('',#25201);
#1442=PLANE('',#25202);
#1443=PLANE('',#25203);
#1444=PLANE('',#25204);
#1445=PLANE('',#25205);
#1446=PLANE('',#25206);
#1447=PLANE('',#25207);
#1448=PLANE('',#25208);
#1449=PLANE('',#25209);
#1450=PLANE('',#25210);
#1451=PLANE('',#25211);
#1452=PLANE('',#25212);
#1453=PLANE('',#25213);
#1454=PLANE('',#25239);
#1455=PLANE('',#25240);
#1456=PLANE('',#25241);
#1457=PLANE('',#25242);
#1458=PLANE('',#25243);
#1459=PLANE('',#25244);
#1460=PLANE('',#25245);
#1461=PLANE('',#25254);
#1462=PLANE('',#25255);
#1463=PLANE('',#25256);
#1464=PLANE('',#25257);
#1465=PLANE('',#25258);
#1466=PLANE('',#25259);
#1467=PLANE('',#25260);
#1468=PLANE('',#25261);
#1469=PLANE('',#25262);
#1470=PLANE('',#25270);
#1471=PLANE('',#25271);
#1472=PLANE('',#25287);
#1473=PLANE('',#25288);
#1474=PLANE('',#25289);
#1475=PLANE('',#25290);
#1476=PLANE('',#25291);
#1477=PLANE('',#25292);
#1478=PLANE('',#25293);
#1479=PLANE('',#25294);
#1480=PLANE('',#25295);
#1481=PLANE('',#25296);
#1482=PLANE('',#25297);
#1483=PLANE('',#25298);
#1484=PLANE('',#25299);
#1485=PLANE('',#25300);
#1486=PLANE('',#25331);
#1487=PLANE('',#25332);
#1488=PLANE('',#25333);
#1489=PLANE('',#25334);
#1490=PLANE('',#25335);
#1491=PLANE('',#25336);
#1492=PLANE('',#25350);
#1493=PLANE('',#25355);
#1494=PLANE('',#25360);
#1495=PLANE('',#25362);
#1496=PLANE('',#25365);
#1497=PLANE('',#25367);
#1498=PLANE('',#25368);
#1499=PLANE('',#25369);
#1500=PLANE('',#25385);
#1501=PLANE('',#25386);
#1502=PLANE('',#25387);
#1503=PLANE('',#25388);
#1504=PLANE('',#25389);
#1505=PLANE('',#25390);
#1506=PLANE('',#25391);
#1507=PLANE('',#25392);
#1508=PLANE('',#25393);
#1509=PLANE('',#25394);
#1510=PLANE('',#25395);
#1511=PLANE('',#25396);
#1512=PLANE('',#25410);
#1513=PLANE('',#25411);
#1514=PLANE('',#25412);
#1515=PLANE('',#25413);
#1516=PLANE('',#25414);
#1517=PLANE('',#25415);
#1518=PLANE('',#25416);
#1519=PLANE('',#25417);
#1520=PLANE('',#25418);
#1521=PLANE('',#25419);
#1522=PLANE('',#25420);
#1523=PLANE('',#25421);
#1524=PLANE('',#25459);
#1525=PLANE('',#25460);
#1526=PLANE('',#25461);
#1527=PLANE('',#25462);
#1528=PLANE('',#25463);
#1529=PLANE('',#25464);
#1530=PLANE('',#25465);
#1531=PLANE('',#25466);
#1532=PLANE('',#25467);
#1533=PLANE('',#25471);
#1534=PLANE('',#25478);
#1535=PLANE('',#25624);
#1536=PLANE('',#25628);
#1537=PLANE('',#25632);
#1538=PLANE('',#25635);
#1539=PLANE('',#25639);
#1540=PLANE('',#25643);
#1541=PLANE('',#25645);
#1542=PLANE('',#25647);
#1543=PLANE('',#25650);
#1544=PLANE('',#25651);
#1545=PLANE('',#25652);
#1546=PLANE('',#25653);
#1547=PLANE('',#25654);
#1548=PLANE('',#25655);
#1549=PLANE('',#25656);
#1550=PLANE('',#25658);
#1551=PLANE('',#25663);
#1552=PLANE('',#25670);
#1553=PLANE('',#25675);
#1554=PLANE('',#25692);
#1555=PLANE('',#25705);
#1556=PLANE('',#25707);
#1557=PLANE('',#25708);
#1558=PLANE('',#25739);
#1559=PLANE('',#25740);
#1560=PLANE('',#25741);
#1561=PLANE('',#25742);
#1562=PLANE('',#25743);
#1563=PLANE('',#25744);
#1564=PLANE('',#25745);
#1565=PLANE('',#25746);
#1566=PLANE('',#25747);
#1567=PLANE('',#25749);
#1568=PLANE('',#25750);
#1569=PLANE('',#25752);
#1570=PLANE('',#25753);
#1571=PLANE('',#25755);
#1572=PLANE('',#25757);
#1573=PLANE('',#25758);
#1574=PLANE('',#25760);
#1575=PLANE('',#25761);
#1576=PLANE('',#25763);
#1577=PLANE('',#25771);
#1578=PLANE('',#25772);
#1579=PLANE('',#25773);
#1580=PLANE('',#25774);
#1581=PLANE('',#25775);
#1582=PLANE('',#25776);
#1583=PLANE('',#25777);
#1584=PLANE('',#25778);
#1585=PLANE('',#25780);
#1586=PLANE('',#25782);
#1587=PLANE('',#25783);
#1588=PLANE('',#25785);
#1589=PLANE('',#25788);
#1590=PLANE('',#25790);
#1591=PLANE('',#25791);
#1592=PLANE('',#25794);
#1593=PLANE('',#25795);
#1594=PLANE('',#25797);
#1595=PLANE('',#25798);
#1596=PLANE('',#25800);
#1597=PLANE('',#25801);
#1598=PLANE('',#25803);
#1599=PLANE('',#25805);
#1600=PLANE('',#25808);
#1601=PLANE('',#25810);
#1602=PLANE('',#25813);
#1603=PLANE('',#25814);
#1604=PLANE('',#25815);
#1605=PLANE('',#25816);
#1606=PLANE('',#25817);
#1607=PLANE('',#25818);
#1608=PLANE('',#25819);
#1609=PLANE('',#25821);
#1610=PLANE('',#25826);
#1611=PLANE('',#25833);
#1612=PLANE('',#25838);
#1613=PLANE('',#25855);
#1614=PLANE('',#25868);
#1615=PLANE('',#25869);
#1616=PLANE('',#25870);
#1617=PLANE('',#25872);
#1618=PLANE('',#25875);
#1619=PLANE('',#25876);
#1620=PLANE('',#25907);
#1621=PLANE('',#25908);
#1622=PLANE('',#25909);
#1623=PLANE('',#25910);
#1624=PLANE('',#25911);
#1625=PLANE('',#25912);
#1626=PLANE('',#25913);
#1627=PLANE('',#25914);
#1628=PLANE('',#25915);
#1629=PLANE('',#25917);
#1630=PLANE('',#25918);
#1631=PLANE('',#25920);
#1632=PLANE('',#25921);
#1633=PLANE('',#25923);
#1634=PLANE('',#25925);
#1635=PLANE('',#25926);
#1636=PLANE('',#25928);
#1637=PLANE('',#25929);
#1638=PLANE('',#25931);
#1639=PLANE('',#25939);
#1640=PLANE('',#25940);
#1641=PLANE('',#25941);
#1642=PLANE('',#25942);
#1643=PLANE('',#25943);
#1644=PLANE('',#25944);
#1645=PLANE('',#25945);
#1646=PLANE('',#25946);
#1647=PLANE('',#25948);
#1648=PLANE('',#25950);
#1649=PLANE('',#25951);
#1650=PLANE('',#25953);
#1651=PLANE('',#25956);
#1652=PLANE('',#25958);
#1653=PLANE('',#25959);
#1654=PLANE('',#25962);
#1655=PLANE('',#25963);
#1656=PLANE('',#25965);
#1657=PLANE('',#25966);
#1658=PLANE('',#25968);
#1659=PLANE('',#25969);
#1660=PLANE('',#25971);
#1661=PLANE('',#25973);
#1662=PLANE('',#26004);
#1663=PLANE('',#26007);
#1664=PLANE('',#26008);
#1665=PLANE('',#26011);
#1666=PLANE('',#26012);
#1667=PLANE('',#26013);
#1668=PLANE('',#26035);
#1669=PLANE('',#26036);
#1670=PLANE('',#26037);
#1671=PLANE('',#26038);
#1672=PLANE('',#26039);
#1673=PLANE('',#26040);
#1674=PLANE('',#26062);
#1675=PLANE('',#26063);
#1676=PLANE('',#26064);
#1677=PLANE('',#26065);
#1678=PLANE('',#26066);
#1679=PLANE('',#26067);
#1680=PLANE('',#26069);
#1681=PLANE('',#26070);
#1682=PLANE('',#26071);
#1683=PLANE('',#26072);
#1684=PLANE('',#26073);
#1685=PLANE('',#26074);
#1686=PLANE('',#26075);
#1687=PLANE('',#26076);
#1688=PLANE('',#26077);
#1689=PLANE('',#26078);
#1690=PLANE('',#26079);
#1691=PLANE('',#26080);
#1692=PLANE('',#26081);
#1693=PLANE('',#26082);
#1694=PLANE('',#26230);
#1695=PLANE('',#26231);
#1696=PLANE('',#26232);
#1697=PLANE('',#26233);
#1698=PLANE('',#26234);
#1699=PLANE('',#26236);
#1700=PLANE('',#26238);
#1701=PLANE('',#26239);
#1702=PLANE('',#26240);
#1703=PLANE('',#26241);
#1704=PLANE('',#26242);
#1705=PLANE('',#26243);
#1706=PLANE('',#26244);
#1707=PLANE('',#26245);
#1708=PLANE('',#26246);
#1709=PLANE('',#26247);
#1710=PLANE('',#26248);
#1711=PLANE('',#26249);
#1712=PLANE('',#26250);
#1713=PLANE('',#26251);
#1714=PLANE('',#26252);
#1715=PLANE('',#26253);
#1716=PLANE('',#26254);
#1717=PLANE('',#26255);
#1718=PLANE('',#26256);
#1719=PLANE('',#26257);
#1720=PLANE('',#26258);
#1721=PLANE('',#26259);
#1722=PLANE('',#26260);
#1723=PLANE('',#26261);
#1724=PLANE('',#26262);
#1725=PLANE('',#26263);
#1726=PLANE('',#26265);
#1727=PLANE('',#26266);
#1728=PLANE('',#26267);
#1729=PLANE('',#26268);
#1730=PLANE('',#26383);
#1731=PLANE('',#26384);
#1732=PLANE('',#26385);
#1733=PLANE('',#26386);
#1734=PLANE('',#26387);
#1735=PLANE('',#26388);
#1736=PLANE('',#26389);
#1737=PLANE('',#26390);
#1738=PLANE('',#26391);
#1739=PLANE('',#26392);
#1740=PLANE('',#26393);
#1741=PLANE('',#26394);
#1742=PLANE('',#26395);
#1743=PLANE('',#26396);
#1744=PLANE('',#26397);
#1745=PLANE('',#26398);
#1746=PLANE('',#26399);
#1747=PLANE('',#26400);
#1748=PLANE('',#26401);
#1749=PLANE('',#26402);
#1750=PLANE('',#26403);
#1751=PLANE('',#26404);
#1752=PLANE('',#26405);
#1753=PLANE('',#26406);
#1754=PLANE('',#26407);
#1755=PLANE('',#26408);
#1756=PLANE('',#26409);
#1757=PLANE('',#26432);
#1758=PLANE('',#26455);
#1759=PLANE('',#26456);
#1760=PLANE('',#26457);
#1761=PLANE('',#26458);
#1762=PLANE('',#26459);
#1763=PLANE('',#26460);
#1764=PLANE('',#26461);
#1765=PLANE('',#26462);
#1766=PLANE('',#26463);
#1767=PLANE('',#26464);
#1768=PLANE('',#26465);
#1769=PLANE('',#26466);
#1770=PLANE('',#26467);
#1771=PLANE('',#26468);
#1772=PLANE('',#26480);
#1773=PLANE('',#26481);
#1774=PLANE('',#26482);
#1775=PLANE('',#26483);
#1776=PLANE('',#26484);
#1777=PLANE('',#26496);
#1778=PLANE('',#26497);
#1779=PLANE('',#26498);
#1780=PLANE('',#26499);
#1781=PLANE('',#26500);
#1782=PLANE('',#26501);
#1783=PLANE('',#26502);
#1784=PLANE('',#26503);
#1785=PLANE('',#26504);
#1786=PLANE('',#26505);
#1787=PLANE('',#26506);
#1788=PLANE('',#26557);
#1789=PLANE('',#26559);
#1790=PLANE('',#26562);
#1791=PLANE('',#26565);
#1792=PLANE('',#26567);
#1793=PLANE('',#26568);
#1794=PLANE('',#26569);
#1795=PLANE('',#26570);
#1796=PLANE('',#26571);
#1797=PLANE('',#26572);
#1798=PLANE('',#26573);
#1799=PLANE('',#26574);
#1800=PLANE('',#26575);
#1801=PLANE('',#26576);
#1802=PLANE('',#26577);
#1803=PLANE('',#26578);
#1804=PLANE('',#26579);
#1805=PLANE('',#26580);
#1806=PLANE('',#26581);
#1807=PLANE('',#26582);
#1808=PLANE('',#26583);
#1809=PLANE('',#26644);
#1810=PLANE('',#26645);
#1811=PLANE('',#26646);
#1812=PLANE('',#26647);
#1813=PLANE('',#26648);
#1814=PLANE('',#26649);
#1815=PLANE('',#26650);
#1816=PLANE('',#26651);
#1817=PLANE('',#26652);
#1818=PLANE('',#26653);
#1819=PLANE('',#26654);
#1820=PLANE('',#26655);
#1821=PLANE('',#26656);
#1822=PLANE('',#26657);
#1823=PLANE('',#26658);
#1824=PLANE('',#26659);
#1825=PLANE('',#26660);
#1826=PLANE('',#26681);
#1827=PLANE('',#26684);
#1828=PLANE('',#26687);
#1829=PLANE('',#26694);
#1830=PLANE('',#26697);
#1831=PLANE('',#26700);
#1832=PLANE('',#26707);
#1833=PLANE('',#26708);
#1834=PLANE('',#26709);
#1835=PLANE('',#26716);
#1836=PLANE('',#26719);
#1837=PLANE('',#26722);
#1838=PLANE('',#26729);
#1839=PLANE('',#26732);
#1840=PLANE('',#26735);
#1841=PLANE('',#26736);
#1842=PLANE('',#26737);
#1843=PLANE('',#26738);
#1844=PLANE('',#26739);
#1845=PLANE('',#26740);
#1846=PLANE('',#26741);
#1847=PLANE('',#26742);
#1848=PLANE('',#26743);
#1849=PLANE('',#26744);
#1850=PLANE('',#26745);
#1851=PLANE('',#26746);
#1852=PLANE('',#26748);
#1853=PLANE('',#26770);
#1854=PLANE('',#26771);
#1855=PLANE('',#26774);
#1856=PLANE('',#26775);
#1857=PLANE('',#26777);
#1858=PLANE('',#26778);
#1859=PLANE('',#26779);
#1860=PLANE('',#26780);
#1861=PLANE('',#26781);
#1862=PLANE('',#26782);
#1863=PLANE('',#26783);
#1864=PLANE('',#26784);
#1865=PLANE('',#26785);
#1866=PLANE('',#26786);
#1867=PLANE('',#26789);
#1868=PLANE('',#26792);
#1869=PLANE('',#26799);
#1870=PLANE('',#26802);
#1871=PLANE('',#26805);
#1872=PLANE('',#26812);
#1873=PLANE('',#26813);
#1874=PLANE('',#26814);
#1875=PLANE('',#26821);
#1876=PLANE('',#26824);
#1877=PLANE('',#26827);
#1878=PLANE('',#26834);
#1879=PLANE('',#26837);
#1880=PLANE('',#26840);
#1881=PLANE('',#26841);
#1882=PLANE('',#26842);
#1883=PLANE('',#26843);
#1884=PLANE('',#26844);
#1885=PLANE('',#26845);
#1886=PLANE('',#26851);
#1887=PLANE('',#26852);
#1888=PLANE('',#26853);
#1889=PLANE('',#26854);
#1890=PLANE('',#26858);
#1891=PLANE('',#26879);
#1892=PLANE('',#26880);
#1893=PLANE('',#26881);
#1894=PLANE('',#26882);
#1895=PLANE('',#26883);
#1896=PLANE('',#26884);
#1897=PLANE('',#26885);
#1898=PLANE('',#26886);
#1899=PLANE('',#26889);
#1900=PLANE('',#26891);
#1901=PLANE('',#26892);
#1902=PLANE('',#26894);
#1903=PLANE('',#26895);
#1904=PLANE('',#26897);
#1905=PLANE('',#26899);
#1906=PLANE('',#26902);
#1907=PLANE('',#26903);
#1908=PLANE('',#26904);
#1909=PLANE('',#26905);
#1910=PLANE('',#26906);
#1911=PLANE('',#26907);
#1912=PLANE('',#26908);
#1913=PLANE('',#26909);
#1914=PLANE('',#26910);
#1915=PLANE('',#26911);
#1916=PLANE('',#26914);
#1917=PLANE('',#26917);
#1918=PLANE('',#26924);
#1919=PLANE('',#26927);
#1920=PLANE('',#26930);
#1921=PLANE('',#26937);
#1922=PLANE('',#26938);
#1923=PLANE('',#26939);
#1924=PLANE('',#26946);
#1925=PLANE('',#26949);
#1926=PLANE('',#26952);
#1927=PLANE('',#26959);
#1928=PLANE('',#26962);
#1929=PLANE('',#26965);
#1930=PLANE('',#26966);
#1931=PLANE('',#26967);
#1932=PLANE('',#26968);
#1933=PLANE('',#26969);
#1934=PLANE('',#26970);
#1935=PLANE('',#26971);
#1936=PLANE('',#26972);
#1937=PLANE('',#26973);
#1938=PLANE('',#26974);
#1939=PLANE('',#26975);
#1940=PLANE('',#26976);
#1941=PLANE('',#26977);
#1942=PLANE('',#26978);
#1943=PLANE('',#26979);
#1944=PLANE('',#26980);
#1945=PLANE('',#26981);
#1946=PLANE('',#26982);
#1947=PLANE('',#26983);
#1948=PLANE('',#26984);
#1949=PLANE('',#26985);
#1950=PLANE('',#26986);
#1951=PLANE('',#26987);
#1952=PLANE('',#26988);
#1953=PLANE('',#26989);
#1954=PLANE('',#26990);
#1955=PLANE('',#26992);
#1956=PLANE('',#26993);
#1957=PLANE('',#26995);
#1958=PLANE('',#26997);
#1959=PLANE('',#26998);
#1960=PLANE('',#27000);
#1961=PLANE('',#27002);
#1962=PLANE('',#27003);
#1963=PLANE('',#27004);
#1964=PLANE('',#27005);
#1965=PLANE('',#27007);
#1966=PLANE('',#27028);
#1967=PLANE('',#27029);
#1968=PLANE('',#27030);
#1969=PLANE('',#27031);
#1970=PLANE('',#27032);
#1971=PLANE('',#27033);
#1972=PLANE('',#27038);
#1973=PLANE('',#27039);
#1974=PLANE('',#27040);
#1975=PLANE('',#27051);
#1976=PLANE('',#27052);
#1977=PLANE('',#27059);
#1978=PLANE('',#27060);
#1979=PLANE('',#27071);
#1980=PLANE('',#27072);
#1981=PLANE('',#27073);
#1982=PLANE('',#27084);
#1983=PLANE('',#27085);
#1984=PLANE('',#27086);
#1985=PLANE('',#27087);
#1986=PLANE('',#27088);
#1987=PLANE('',#27089);
#1988=PLANE('',#27090);
#1989=PLANE('',#27091);
#1990=PLANE('',#27092);
#1991=PLANE('',#27093);
#1992=PLANE('',#27094);
#1993=PLANE('',#27095);
#1994=PLANE('',#27096);
#1995=PLANE('',#27097);
#1996=PLANE('',#27098);
#1997=PLANE('',#27101);
#1998=PLANE('',#27102);
#1999=PLANE('',#27137);
#2000=PLANE('',#27143);
#2001=PLANE('',#27149);
#2002=PLANE('',#27150);
#2003=PLANE('',#27151);
#2004=PLANE('',#27152);
#2005=PLANE('',#27153);
#2006=PLANE('',#27154);
#2007=PLANE('',#27155);
#2008=PLANE('',#27156);
#2009=PLANE('',#27157);
#2010=PLANE('',#27158);
#2011=PLANE('',#27159);
#2012=PLANE('',#27160);
#2013=PLANE('',#27161);
#2014=PLANE('',#27172);
#2015=PLANE('',#27173);
#2016=PLANE('',#27174);
#2017=PLANE('',#27175);
#2018=PLANE('',#27176);
#2019=PLANE('',#27177);
#2020=PLANE('',#27178);
#2021=PLANE('',#27222);
#2022=PLANE('',#27223);
#2023=PLANE('',#27226);
#2024=PLANE('',#27227);
#2025=PLANE('',#27230);
#2026=PLANE('',#27231);
#2027=PLANE('',#27232);
#2028=PLANE('',#27233);
#2029=PLANE('',#27234);
#2030=PLANE('',#27235);
#2031=PLANE('',#27259);
#2032=PLANE('',#27260);
#2033=PLANE('',#27261);
#2034=PLANE('',#27262);
#2035=PLANE('',#27263);
#2036=PLANE('',#27264);
#2037=PLANE('',#27265);
#2038=PLANE('',#27266);
#2039=PLANE('',#27267);
#2040=PLANE('',#27268);
#2041=PLANE('',#27269);
#2042=PLANE('',#27270);
#2043=PLANE('',#27271);
#2044=PLANE('',#27272);
#2045=PLANE('',#27273);
#2046=PLANE('',#27274);
#2047=PLANE('',#27281);
#2048=PLANE('',#27282);
#2049=PLANE('',#27289);
#2050=PLANE('',#27290);
#2051=PLANE('',#27291);
#2052=PLANE('',#27292);
#2053=PLANE('',#27305);
#2054=PLANE('',#27306);
#2055=PLANE('',#27307);
#2056=PLANE('',#27308);
#2057=PLANE('',#27309);
#2058=PLANE('',#27310);
#2059=PLANE('',#27311);
#2060=PLANE('',#27312);
#2061=PLANE('',#27313);
#2062=PLANE('',#27314);
#2063=PLANE('',#27336);
#2064=PLANE('',#27337);
#2065=PLANE('',#27338);
#2066=PLANE('',#27339);
#2067=PLANE('',#27340);
#2068=PLANE('',#27341);
#2069=PLANE('',#27342);
#2070=PLANE('',#27343);
#2071=PLANE('',#27344);
#2072=PLANE('',#27345);
#2073=PLANE('',#27346);
#2074=PLANE('',#27347);
#2075=PLANE('',#27348);
#2076=PLANE('',#27349);
#2077=PLANE('',#27350);
#2078=PLANE('',#27351);
#2079=PLANE('',#27358);
#2080=PLANE('',#27359);
#2081=PLANE('',#27366);
#2082=PLANE('',#27367);
#2083=PLANE('',#27368);
#2084=PLANE('',#27369);
#2085=PLANE('',#27382);
#2086=PLANE('',#27383);
#2087=PLANE('',#27384);
#2088=PLANE('',#27385);
#2089=PLANE('',#27386);
#2090=PLANE('',#27387);
#2091=PLANE('',#27388);
#2092=PLANE('',#27389);
#2093=PLANE('',#27390);
#2094=PLANE('',#27391);
#2095=PLANE('',#27404);
#2096=PLANE('',#27405);
#2097=PLANE('',#27406);
#2098=PLANE('',#27407);
#2099=PLANE('',#27408);
#2100=PLANE('',#27409);
#2101=PLANE('',#27410);
#2102=PLANE('',#27411);
#2103=PLANE('',#27412);
#2104=PLANE('',#27413);
#2105=CONICAL_SURFACE('',#24912,3.,1.02974425867665);
#2106=CONICAL_SURFACE('',#24916,3.,1.02974425867665);
#2107=CONICAL_SURFACE('',#24920,2.49999999999999,1.02974425867666);
#2108=CONICAL_SURFACE('',#24924,2.49999999999999,1.02974425867666);
#2109=CONICAL_SURFACE('',#24945,5.50000000000001,0.785398163397526);
#2110=CONICAL_SURFACE('',#24953,7.00000000000006,0.785398163397535);
#2111=CONICAL_SURFACE('',#24959,7.49999999999999,0.785398163397418);
#2112=CONICAL_SURFACE('',#24974,5.,0.785398163397416);
#2113=CONICAL_SURFACE('',#24981,4.50000000000006,0.78539816339741);
#2114=CONICAL_SURFACE('',#25079,1.5,1.02974425867665);
#2115=CONICAL_SURFACE('',#25086,1.5,1.02974425867665);
#2116=CONICAL_SURFACE('',#25093,1.5,1.02974425867665);
#2117=CONICAL_SURFACE('',#25100,1.5,1.02974425867665);
#2118=CONICAL_SURFACE('',#25216,5.4585,0.785398163397448);
#2119=CONICAL_SURFACE('',#25220,6.,0.785398163397449);
#2120=CONICAL_SURFACE('',#25246,2.,0.785398163397445);
#2121=CONICAL_SURFACE('',#25249,1.25,0.78539816339745);
#2122=CONICAL_SURFACE('',#25666,19.5,0.785398163397448);
#2123=CONICAL_SURFACE('',#25829,19.5,0.785398163397448);
#2124=CONICAL_SURFACE('',#26517,2.5,1.02974425867665);
#2125=CONICAL_SURFACE('',#26518,2.5,1.02974425867665);
#2126=CONICAL_SURFACE('',#26544,2.5,1.02974425867665);
#2127=CONICAL_SURFACE('',#26545,2.5,1.02974425867665);
#2128=CONICAL_SURFACE('',#27114,2.5,0.371257902576146);
#2129=CONICAL_SURFACE('',#27118,4.00000000000001,1.04719755119661);
#2130=CONICAL_SURFACE('',#27120,3.46410161513776,1.0471975511966);
#2131=CONICAL_SURFACE('',#27162,3.46410161513776,1.0471975511966);
#2132=CONICAL_SURFACE('',#27163,3.46410161513776,1.0471975511966);
#2133=CONICAL_SURFACE('',#27164,3.46410161513776,1.0471975511966);
#2134=CONICAL_SURFACE('',#27165,3.46410161513776,1.0471975511966);
#2135=CONICAL_SURFACE('',#27166,3.46410161513776,1.0471975511966);
#2136=CONICAL_SURFACE('',#27167,4.00000000000001,1.04719755119661);
#2137=CONICAL_SURFACE('',#27168,4.00000000000001,1.04719755119661);
#2138=CONICAL_SURFACE('',#27169,4.00000000000001,1.04719755119661);
#2139=CONICAL_SURFACE('',#27170,4.00000000000001,1.04719755119661);
#2140=CONICAL_SURFACE('',#27171,4.00000000000001,1.04719755119661);
#2141=CONICAL_SURFACE('',#27193,2.5,1.02974425867665);
#2142=CONICAL_SURFACE('',#27197,2.5,1.02974425867665);
#2143=CONICAL_SURFACE('',#27201,2.5,1.02974425867665);
#2144=CONICAL_SURFACE('',#27205,2.5,1.02974425867665);
#2145=CONICAL_SURFACE('',#27209,2.5,1.02974425867665);
#2146=CONICAL_SURFACE('',#27213,2.5,1.02974425867665);
#2147=CONICAL_SURFACE('',#27217,2.5,1.02974425867665);
#2148=CONICAL_SURFACE('',#27221,2.5,1.02974425867665);
#2149=CONICAL_SURFACE('',#27239,3.75,0.785398163397444);
#2150=CONICAL_SURFACE('',#27243,1664.2794823505,1.02974425867665);
#2151=CONICAL_SURFACE('',#27297,5.,0.785398163397451);
#2152=CONICAL_SURFACE('',#27299,2.4585,0.785398163397442);
#2153=CONICAL_SURFACE('',#27316,5.7,0.785398163397444);
#2154=CONICAL_SURFACE('',#27320,1664.2794823505,1.02974425867665);
#2155=CONICAL_SURFACE('',#27374,5.,0.785398163397445);
#2156=CONICAL_SURFACE('',#27376,2.4585,0.785398163397448);
#2157=CONICAL_SURFACE('',#27396,3.5,0.785398163397447);
#2158=CONICAL_SURFACE('',#27398,1.621,0.785398163397443);
#2159=FACE_OUTER_BOUND('',#3534,.T.);
#2160=FACE_OUTER_BOUND('',#3535,.T.);
#2161=FACE_OUTER_BOUND('',#3536,.T.);
#2162=FACE_OUTER_BOUND('',#3537,.T.);
#2163=FACE_OUTER_BOUND('',#3538,.T.);
#2164=FACE_OUTER_BOUND('',#3539,.T.);
#2165=FACE_OUTER_BOUND('',#3540,.T.);
#2166=FACE_OUTER_BOUND('',#3541,.T.);
#2167=FACE_OUTER_BOUND('',#3542,.T.);
#2168=FACE_OUTER_BOUND('',#3543,.T.);
#2169=FACE_OUTER_BOUND('',#3544,.T.);
#2170=FACE_OUTER_BOUND('',#3545,.T.);
#2171=FACE_OUTER_BOUND('',#3546,.T.);
#2172=FACE_OUTER_BOUND('',#3547,.T.);
#2173=FACE_OUTER_BOUND('',#3548,.T.);
#2174=FACE_OUTER_BOUND('',#3549,.T.);
#2175=FACE_OUTER_BOUND('',#3550,.T.);
#2176=FACE_OUTER_BOUND('',#3551,.T.);
#2177=FACE_OUTER_BOUND('',#3552,.T.);
#2178=FACE_OUTER_BOUND('',#3557,.T.);
#2179=FACE_OUTER_BOUND('',#3558,.T.);
#2180=FACE_OUTER_BOUND('',#3559,.T.);
#2181=FACE_OUTER_BOUND('',#3568,.T.);
#2182=FACE_OUTER_BOUND('',#3577,.T.);
#2183=FACE_OUTER_BOUND('',#3578,.T.);
#2184=FACE_OUTER_BOUND('',#3579,.T.);
#2185=FACE_OUTER_BOUND('',#3580,.T.);
#2186=FACE_OUTER_BOUND('',#3581,.T.);
#2187=FACE_OUTER_BOUND('',#3582,.T.);
#2188=FACE_OUTER_BOUND('',#3583,.T.);
#2189=FACE_OUTER_BOUND('',#3584,.T.);
#2190=FACE_OUTER_BOUND('',#3585,.T.);
#2191=FACE_OUTER_BOUND('',#3586,.T.);
#2192=FACE_OUTER_BOUND('',#3587,.T.);
#2193=FACE_OUTER_BOUND('',#3588,.T.);
#2194=FACE_OUTER_BOUND('',#3589,.T.);
#2195=FACE_OUTER_BOUND('',#3590,.T.);
#2196=FACE_OUTER_BOUND('',#3591,.T.);
#2197=FACE_OUTER_BOUND('',#3592,.T.);
#2198=FACE_OUTER_BOUND('',#3593,.T.);
#2199=FACE_OUTER_BOUND('',#3595,.T.);
#2200=FACE_OUTER_BOUND('',#3597,.T.);
#2201=FACE_OUTER_BOUND('',#3599,.T.);
#2202=FACE_OUTER_BOUND('',#3601,.T.);
#2203=FACE_OUTER_BOUND('',#3603,.T.);
#2204=FACE_OUTER_BOUND('',#3604,.T.);
#2205=FACE_OUTER_BOUND('',#3605,.T.);
#2206=FACE_OUTER_BOUND('',#3606,.T.);
#2207=FACE_OUTER_BOUND('',#3607,.T.);
#2208=FACE_OUTER_BOUND('',#3608,.T.);
#2209=FACE_OUTER_BOUND('',#3609,.T.);
#2210=FACE_OUTER_BOUND('',#3610,.T.);
#2211=FACE_OUTER_BOUND('',#3611,.T.);
#2212=FACE_OUTER_BOUND('',#3612,.T.);
#2213=FACE_OUTER_BOUND('',#3613,.T.);
#2214=FACE_OUTER_BOUND('',#3614,.T.);
#2215=FACE_OUTER_BOUND('',#3615,.T.);
#2216=FACE_OUTER_BOUND('',#3616,.T.);
#2217=FACE_OUTER_BOUND('',#3617,.T.);
#2218=FACE_OUTER_BOUND('',#3618,.T.);
#2219=FACE_OUTER_BOUND('',#3619,.T.);
#2220=FACE_OUTER_BOUND('',#3620,.T.);
#2221=FACE_OUTER_BOUND('',#3622,.T.);
#2222=FACE_OUTER_BOUND('',#3623,.T.);
#2223=FACE_OUTER_BOUND('',#3624,.T.);
#2224=FACE_OUTER_BOUND('',#3625,.T.);
#2225=FACE_OUTER_BOUND('',#3633,.T.);
#2226=FACE_OUTER_BOUND('',#3634,.T.);
#2227=FACE_OUTER_BOUND('',#3635,.T.);
#2228=FACE_OUTER_BOUND('',#3637,.T.);
#2229=FACE_OUTER_BOUND('',#3638,.T.);
#2230=FACE_OUTER_BOUND('',#3639,.T.);
#2231=FACE_OUTER_BOUND('',#3640,.T.);
#2232=FACE_OUTER_BOUND('',#3648,.T.);
#2233=FACE_OUTER_BOUND('',#3650,.T.);
#2234=FACE_OUTER_BOUND('',#3652,.T.);
#2235=FACE_OUTER_BOUND('',#3654,.T.);
#2236=FACE_OUTER_BOUND('',#3656,.T.);
#2237=FACE_OUTER_BOUND('',#3658,.T.);
#2238=FACE_OUTER_BOUND('',#3659,.T.);
#2239=FACE_OUTER_BOUND('',#3660,.T.);
#2240=FACE_OUTER_BOUND('',#3661,.T.);
#2241=FACE_OUTER_BOUND('',#3662,.T.);
#2242=FACE_OUTER_BOUND('',#3663,.T.);
#2243=FACE_OUTER_BOUND('',#3664,.T.);
#2244=FACE_OUTER_BOUND('',#3665,.T.);
#2245=FACE_OUTER_BOUND('',#3666,.T.);
#2246=FACE_OUTER_BOUND('',#3667,.T.);
#2247=FACE_OUTER_BOUND('',#3668,.T.);
#2248=FACE_OUTER_BOUND('',#3669,.T.);
#2249=FACE_OUTER_BOUND('',#3670,.T.);
#2250=FACE_OUTER_BOUND('',#3671,.T.);
#2251=FACE_OUTER_BOUND('',#3672,.T.);
#2252=FACE_OUTER_BOUND('',#3673,.T.);
#2253=FACE_OUTER_BOUND('',#3674,.T.);
#2254=FACE_OUTER_BOUND('',#3675,.T.);
#2255=FACE_OUTER_BOUND('',#3676,.T.);
#2256=FACE_OUTER_BOUND('',#3677,.T.);
#2257=FACE_OUTER_BOUND('',#3678,.T.);
#2258=FACE_OUTER_BOUND('',#3679,.T.);
#2259=FACE_OUTER_BOUND('',#3681,.T.);
#2260=FACE_OUTER_BOUND('',#3683,.T.);
#2261=FACE_OUTER_BOUND('',#3685,.T.);
#2262=FACE_OUTER_BOUND('',#3687,.T.);
#2263=FACE_OUTER_BOUND('',#3689,.T.);
#2264=FACE_OUTER_BOUND('',#3691,.T.);
#2265=FACE_OUTER_BOUND('',#3692,.T.);
#2266=FACE_OUTER_BOUND('',#3693,.T.);
#2267=FACE_OUTER_BOUND('',#3696,.T.);
#2268=FACE_OUTER_BOUND('',#3697,.T.);
#2269=FACE_OUTER_BOUND('',#3698,.T.);
#2270=FACE_OUTER_BOUND('',#3700,.T.);
#2271=FACE_OUTER_BOUND('',#3701,.T.);
#2272=FACE_OUTER_BOUND('',#3702,.T.);
#2273=FACE_OUTER_BOUND('',#3703,.T.);
#2274=FACE_OUTER_BOUND('',#3704,.T.);
#2275=FACE_OUTER_BOUND('',#3705,.T.);
#2276=FACE_OUTER_BOUND('',#3707,.T.);
#2277=FACE_OUTER_BOUND('',#3713,.T.);
#2278=FACE_OUTER_BOUND('',#3714,.T.);
#2279=FACE_OUTER_BOUND('',#3715,.T.);
#2280=FACE_OUTER_BOUND('',#3716,.T.);
#2281=FACE_OUTER_BOUND('',#3717,.T.);
#2282=FACE_OUTER_BOUND('',#3718,.T.);
#2283=FACE_OUTER_BOUND('',#3719,.T.);
#2284=FACE_OUTER_BOUND('',#3720,.T.);
#2285=FACE_OUTER_BOUND('',#3721,.T.);
#2286=FACE_OUTER_BOUND('',#3723,.T.);
#2287=FACE_OUTER_BOUND('',#3725,.T.);
#2288=FACE_OUTER_BOUND('',#3727,.T.);
#2289=FACE_OUTER_BOUND('',#3729,.T.);
#2290=FACE_OUTER_BOUND('',#3730,.T.);
#2291=FACE_OUTER_BOUND('',#3731,.T.);
#2292=FACE_OUTER_BOUND('',#3732,.T.);
#2293=FACE_OUTER_BOUND('',#3733,.T.);
#2294=FACE_OUTER_BOUND('',#3734,.T.);
#2295=FACE_OUTER_BOUND('',#3735,.T.);
#2296=FACE_OUTER_BOUND('',#3736,.T.);
#2297=FACE_OUTER_BOUND('',#3737,.T.);
#2298=FACE_OUTER_BOUND('',#3738,.T.);
#2299=FACE_OUTER_BOUND('',#3739,.T.);
#2300=FACE_OUTER_BOUND('',#3740,.T.);
#2301=FACE_OUTER_BOUND('',#3741,.T.);
#2302=FACE_OUTER_BOUND('',#3742,.T.);
#2303=FACE_OUTER_BOUND('',#3743,.T.);
#2304=FACE_OUTER_BOUND('',#3744,.T.);
#2305=FACE_OUTER_BOUND('',#3745,.T.);
#2306=FACE_OUTER_BOUND('',#3746,.T.);
#2307=FACE_OUTER_BOUND('',#3747,.T.);
#2308=FACE_OUTER_BOUND('',#3748,.T.);
#2309=FACE_OUTER_BOUND('',#3749,.T.);
#2310=FACE_OUTER_BOUND('',#3750,.T.);
#2311=FACE_OUTER_BOUND('',#3751,.T.);
#2312=FACE_OUTER_BOUND('',#3752,.T.);
#2313=FACE_OUTER_BOUND('',#3753,.T.);
#2314=FACE_OUTER_BOUND('',#3754,.T.);
#2315=FACE_OUTER_BOUND('',#3755,.T.);
#2316=FACE_OUTER_BOUND('',#3756,.T.);
#2317=FACE_OUTER_BOUND('',#3757,.T.);
#2318=FACE_OUTER_BOUND('',#3758,.T.);
#2319=FACE_OUTER_BOUND('',#3759,.T.);
#2320=FACE_OUTER_BOUND('',#3760,.T.);
#2321=FACE_OUTER_BOUND('',#3761,.T.);
#2322=FACE_OUTER_BOUND('',#3762,.T.);
#2323=FACE_OUTER_BOUND('',#3763,.T.);
#2324=FACE_OUTER_BOUND('',#3764,.T.);
#2325=FACE_OUTER_BOUND('',#3765,.T.);
#2326=FACE_OUTER_BOUND('',#3766,.T.);
#2327=FACE_OUTER_BOUND('',#3767,.T.);
#2328=FACE_OUTER_BOUND('',#3768,.T.);
#2329=FACE_OUTER_BOUND('',#3769,.T.);
#2330=FACE_OUTER_BOUND('',#3770,.T.);
#2331=FACE_OUTER_BOUND('',#3771,.T.);
#2332=FACE_OUTER_BOUND('',#3772,.T.);
#2333=FACE_OUTER_BOUND('',#3773,.T.);
#2334=FACE_OUTER_BOUND('',#3774,.T.);
#2335=FACE_OUTER_BOUND('',#3775,.T.);
#2336=FACE_OUTER_BOUND('',#3776,.T.);
#2337=FACE_OUTER_BOUND('',#3777,.T.);
#2338=FACE_OUTER_BOUND('',#3779,.T.);
#2339=FACE_OUTER_BOUND('',#3781,.T.);
#2340=FACE_OUTER_BOUND('',#3783,.T.);
#2341=FACE_OUTER_BOUND('',#3785,.T.);
#2342=FACE_OUTER_BOUND('',#3786,.T.);
#2343=FACE_OUTER_BOUND('',#3787,.T.);
#2344=FACE_OUTER_BOUND('',#3788,.T.);
#2345=FACE_OUTER_BOUND('',#3790,.T.);
#2346=FACE_OUTER_BOUND('',#3791,.T.);
#2347=FACE_OUTER_BOUND('',#3792,.T.);
#2348=FACE_OUTER_BOUND('',#3793,.T.);
#2349=FACE_OUTER_BOUND('',#3794,.T.);
#2350=FACE_OUTER_BOUND('',#3796,.T.);
#2351=FACE_OUTER_BOUND('',#3798,.T.);
#2352=FACE_OUTER_BOUND('',#3800,.T.);
#2353=FACE_OUTER_BOUND('',#3802,.T.);
#2354=FACE_OUTER_BOUND('',#3803,.T.);
#2355=FACE_OUTER_BOUND('',#3804,.T.);
#2356=FACE_OUTER_BOUND('',#3805,.T.);
#2357=FACE_OUTER_BOUND('',#3806,.T.);
#2358=FACE_OUTER_BOUND('',#3807,.T.);
#2359=FACE_OUTER_BOUND('',#3808,.T.);
#2360=FACE_OUTER_BOUND('',#3809,.T.);
#2361=FACE_OUTER_BOUND('',#3810,.T.);
#2362=FACE_OUTER_BOUND('',#3812,.T.);
#2363=FACE_OUTER_BOUND('',#3813,.T.);
#2364=FACE_OUTER_BOUND('',#3814,.T.);
#2365=FACE_OUTER_BOUND('',#3815,.T.);
#2366=FACE_OUTER_BOUND('',#3816,.T.);
#2367=FACE_OUTER_BOUND('',#3817,.T.);
#2368=FACE_OUTER_BOUND('',#3818,.T.);
#2369=FACE_OUTER_BOUND('',#3819,.T.);
#2370=FACE_OUTER_BOUND('',#3820,.T.);
#2371=FACE_OUTER_BOUND('',#3821,.T.);
#2372=FACE_OUTER_BOUND('',#3823,.T.);
#2373=FACE_OUTER_BOUND('',#3825,.T.);
#2374=FACE_OUTER_BOUND('',#3826,.T.);
#2375=FACE_OUTER_BOUND('',#3827,.T.);
#2376=FACE_OUTER_BOUND('',#3828,.T.);
#2377=FACE_OUTER_BOUND('',#3830,.T.);
#2378=FACE_OUTER_BOUND('',#3832,.T.);
#2379=FACE_OUTER_BOUND('',#3834,.T.);
#2380=FACE_OUTER_BOUND('',#3835,.T.);
#2381=FACE_OUTER_BOUND('',#3836,.T.);
#2382=FACE_OUTER_BOUND('',#3839,.T.);
#2383=FACE_OUTER_BOUND('',#3840,.T.);
#2384=FACE_OUTER_BOUND('',#3841,.T.);
#2385=FACE_OUTER_BOUND('',#3843,.T.);
#2386=FACE_OUTER_BOUND('',#3844,.T.);
#2387=FACE_OUTER_BOUND('',#3845,.T.);
#2388=FACE_OUTER_BOUND('',#3846,.T.);
#2389=FACE_OUTER_BOUND('',#3847,.T.);
#2390=FACE_OUTER_BOUND('',#3848,.T.);
#2391=FACE_OUTER_BOUND('',#3849,.T.);
#2392=FACE_OUTER_BOUND('',#3850,.T.);
#2393=FACE_OUTER_BOUND('',#3851,.T.);
#2394=FACE_OUTER_BOUND('',#3852,.T.);
#2395=FACE_OUTER_BOUND('',#3853,.T.);
#2396=FACE_OUTER_BOUND('',#3854,.T.);
#2397=FACE_OUTER_BOUND('',#3855,.T.);
#2398=FACE_OUTER_BOUND('',#3856,.T.);
#2399=FACE_OUTER_BOUND('',#3857,.T.);
#2400=FACE_OUTER_BOUND('',#3858,.T.);
#2401=FACE_OUTER_BOUND('',#3860,.T.);
#2402=FACE_OUTER_BOUND('',#3862,.T.);
#2403=FACE_OUTER_BOUND('',#3864,.T.);
#2404=FACE_OUTER_BOUND('',#3866,.T.);
#2405=FACE_OUTER_BOUND('',#3868,.T.);
#2406=FACE_OUTER_BOUND('',#3870,.T.);
#2407=FACE_OUTER_BOUND('',#3871,.T.);
#2408=FACE_OUTER_BOUND('',#3872,.T.);
#2409=FACE_OUTER_BOUND('',#3873,.T.);
#2410=FACE_OUTER_BOUND('',#3874,.T.);
#2411=FACE_OUTER_BOUND('',#3877,.T.);
#2412=FACE_OUTER_BOUND('',#3880,.T.);
#2413=FACE_OUTER_BOUND('',#3881,.T.);
#2414=FACE_OUTER_BOUND('',#3882,.T.);
#2415=FACE_OUTER_BOUND('',#3883,.T.);
#2416=FACE_OUTER_BOUND('',#3884,.T.);
#2417=FACE_OUTER_BOUND('',#3885,.T.);
#2418=FACE_OUTER_BOUND('',#3886,.T.);
#2419=FACE_OUTER_BOUND('',#3887,.T.);
#2420=FACE_OUTER_BOUND('',#3888,.T.);
#2421=FACE_OUTER_BOUND('',#3889,.T.);
#2422=FACE_OUTER_BOUND('',#3890,.T.);
#2423=FACE_OUTER_BOUND('',#3891,.T.);
#2424=FACE_OUTER_BOUND('',#3892,.T.);
#2425=FACE_OUTER_BOUND('',#3893,.T.);
#2426=FACE_OUTER_BOUND('',#3894,.T.);
#2427=FACE_OUTER_BOUND('',#3895,.T.);
#2428=FACE_OUTER_BOUND('',#3896,.T.);
#2429=FACE_OUTER_BOUND('',#3897,.T.);
#2430=FACE_OUTER_BOUND('',#3898,.T.);
#2431=FACE_OUTER_BOUND('',#3899,.T.);
#2432=FACE_OUTER_BOUND('',#3900,.T.);
#2433=FACE_OUTER_BOUND('',#3905,.T.);
#2434=FACE_OUTER_BOUND('',#3906,.T.);
#2435=FACE_OUTER_BOUND('',#3907,.T.);
#2436=FACE_OUTER_BOUND('',#3908,.T.);
#2437=FACE_OUTER_BOUND('',#3909,.T.);
#2438=FACE_OUTER_BOUND('',#3914,.T.);
#2439=FACE_OUTER_BOUND('',#3915,.T.);
#2440=FACE_OUTER_BOUND('',#3916,.T.);
#2441=FACE_OUTER_BOUND('',#3917,.T.);
#2442=FACE_OUTER_BOUND('',#3918,.T.);
#2443=FACE_OUTER_BOUND('',#3919,.T.);
#2444=FACE_OUTER_BOUND('',#3920,.T.);
#2445=FACE_OUTER_BOUND('',#3921,.T.);
#2446=FACE_OUTER_BOUND('',#3922,.T.);
#2447=FACE_OUTER_BOUND('',#3923,.T.);
#2448=FACE_OUTER_BOUND('',#3924,.T.);
#2449=FACE_OUTER_BOUND('',#3929,.T.);
#2450=FACE_OUTER_BOUND('',#3930,.T.);
#2451=FACE_OUTER_BOUND('',#3931,.T.);
#2452=FACE_OUTER_BOUND('',#3932,.T.);
#2453=FACE_OUTER_BOUND('',#3933,.T.);
#2454=FACE_OUTER_BOUND('',#3938,.T.);
#2455=FACE_OUTER_BOUND('',#3939,.T.);
#2456=FACE_OUTER_BOUND('',#3940,.T.);
#2457=FACE_OUTER_BOUND('',#3941,.T.);
#2458=FACE_OUTER_BOUND('',#3942,.T.);
#2459=FACE_OUTER_BOUND('',#3943,.T.);
#2460=FACE_OUTER_BOUND('',#3944,.T.);
#2461=FACE_OUTER_BOUND('',#3945,.T.);
#2462=FACE_OUTER_BOUND('',#3946,.T.);
#2463=FACE_OUTER_BOUND('',#3947,.T.);
#2464=FACE_OUTER_BOUND('',#3948,.T.);
#2465=FACE_OUTER_BOUND('',#3949,.T.);
#2466=FACE_OUTER_BOUND('',#3950,.T.);
#2467=FACE_OUTER_BOUND('',#3960,.T.);
#2468=FACE_OUTER_BOUND('',#3961,.T.);
#2469=FACE_OUTER_BOUND('',#3962,.T.);
#2470=FACE_OUTER_BOUND('',#3963,.T.);
#2471=FACE_OUTER_BOUND('',#3964,.T.);
#2472=FACE_OUTER_BOUND('',#3974,.T.);
#2473=FACE_OUTER_BOUND('',#3976,.T.);
#2474=FACE_OUTER_BOUND('',#3978,.T.);
#2475=FACE_OUTER_BOUND('',#3980,.T.);
#2476=FACE_OUTER_BOUND('',#3981,.T.);
#2477=FACE_OUTER_BOUND('',#3982,.T.);
#2478=FACE_OUTER_BOUND('',#3983,.T.);
#2479=FACE_OUTER_BOUND('',#3984,.T.);
#2480=FACE_OUTER_BOUND('',#3985,.T.);
#2481=FACE_OUTER_BOUND('',#3986,.T.);
#2482=FACE_OUTER_BOUND('',#3987,.T.);
#2483=FACE_OUTER_BOUND('',#3988,.T.);
#2484=FACE_OUTER_BOUND('',#3989,.T.);
#2485=FACE_OUTER_BOUND('',#3990,.T.);
#2486=FACE_OUTER_BOUND('',#3991,.T.);
#2487=FACE_OUTER_BOUND('',#3992,.T.);
#2488=FACE_OUTER_BOUND('',#3993,.T.);
#2489=FACE_OUTER_BOUND('',#3994,.T.);
#2490=FACE_OUTER_BOUND('',#3995,.T.);
#2491=FACE_OUTER_BOUND('',#3996,.T.);
#2492=FACE_OUTER_BOUND('',#3997,.T.);
#2493=FACE_OUTER_BOUND('',#3998,.T.);
#2494=FACE_OUTER_BOUND('',#3999,.T.);
#2495=FACE_OUTER_BOUND('',#4000,.T.);
#2496=FACE_OUTER_BOUND('',#4001,.T.);
#2497=FACE_OUTER_BOUND('',#4002,.T.);
#2498=FACE_OUTER_BOUND('',#4003,.T.);
#2499=FACE_OUTER_BOUND('',#4004,.T.);
#2500=FACE_OUTER_BOUND('',#4005,.T.);
#2501=FACE_OUTER_BOUND('',#4006,.T.);
#2502=FACE_OUTER_BOUND('',#4007,.T.);
#2503=FACE_OUTER_BOUND('',#4008,.T.);
#2504=FACE_OUTER_BOUND('',#4009,.T.);
#2505=FACE_OUTER_BOUND('',#4010,.T.);
#2506=FACE_OUTER_BOUND('',#4011,.T.);
#2507=FACE_OUTER_BOUND('',#4012,.T.);
#2508=FACE_OUTER_BOUND('',#4013,.T.);
#2509=FACE_OUTER_BOUND('',#4014,.T.);
#2510=FACE_OUTER_BOUND('',#4015,.T.);
#2511=FACE_OUTER_BOUND('',#4016,.T.);
#2512=FACE_OUTER_BOUND('',#4017,.T.);
#2513=FACE_OUTER_BOUND('',#4018,.T.);
#2514=FACE_OUTER_BOUND('',#4019,.T.);
#2515=FACE_OUTER_BOUND('',#4020,.T.);
#2516=FACE_OUTER_BOUND('',#4021,.T.);
#2517=FACE_OUTER_BOUND('',#4022,.T.);
#2518=FACE_OUTER_BOUND('',#4023,.T.);
#2519=FACE_OUTER_BOUND('',#4024,.T.);
#2520=FACE_OUTER_BOUND('',#4025,.T.);
#2521=FACE_OUTER_BOUND('',#4026,.T.);
#2522=FACE_OUTER_BOUND('',#4027,.T.);
#2523=FACE_OUTER_BOUND('',#4028,.T.);
#2524=FACE_OUTER_BOUND('',#4029,.T.);
#2525=FACE_OUTER_BOUND('',#4030,.T.);
#2526=FACE_OUTER_BOUND('',#4031,.T.);
#2527=FACE_OUTER_BOUND('',#4032,.T.);
#2528=FACE_OUTER_BOUND('',#4033,.T.);
#2529=FACE_OUTER_BOUND('',#4034,.T.);
#2530=FACE_OUTER_BOUND('',#4035,.T.);
#2531=FACE_OUTER_BOUND('',#4036,.T.);
#2532=FACE_OUTER_BOUND('',#4037,.T.);
#2533=FACE_OUTER_BOUND('',#4038,.T.);
#2534=FACE_OUTER_BOUND('',#4039,.T.);
#2535=FACE_OUTER_BOUND('',#4040,.T.);
#2536=FACE_OUTER_BOUND('',#4041,.T.);
#2537=FACE_OUTER_BOUND('',#4042,.T.);
#2538=FACE_OUTER_BOUND('',#4043,.T.);
#2539=FACE_OUTER_BOUND('',#4044,.T.);
#2540=FACE_OUTER_BOUND('',#4045,.T.);
#2541=FACE_OUTER_BOUND('',#4046,.T.);
#2542=FACE_OUTER_BOUND('',#4047,.T.);
#2543=FACE_OUTER_BOUND('',#4048,.T.);
#2544=FACE_OUTER_BOUND('',#4049,.T.);
#2545=FACE_OUTER_BOUND('',#4050,.T.);
#2546=FACE_OUTER_BOUND('',#4051,.T.);
#2547=FACE_OUTER_BOUND('',#4052,.T.);
#2548=FACE_OUTER_BOUND('',#4053,.T.);
#2549=FACE_OUTER_BOUND('',#4054,.T.);
#2550=FACE_OUTER_BOUND('',#4055,.T.);
#2551=FACE_OUTER_BOUND('',#4056,.T.);
#2552=FACE_OUTER_BOUND('',#4057,.T.);
#2553=FACE_OUTER_BOUND('',#4058,.T.);
#2554=FACE_OUTER_BOUND('',#4059,.T.);
#2555=FACE_OUTER_BOUND('',#4060,.T.);
#2556=FACE_OUTER_BOUND('',#4061,.T.);
#2557=FACE_OUTER_BOUND('',#4062,.T.);
#2558=FACE_OUTER_BOUND('',#4063,.T.);
#2559=FACE_OUTER_BOUND('',#4064,.T.);
#2560=FACE_OUTER_BOUND('',#4065,.T.);
#2561=FACE_OUTER_BOUND('',#4066,.T.);
#2562=FACE_OUTER_BOUND('',#4067,.T.);
#2563=FACE_OUTER_BOUND('',#4068,.T.);
#2564=FACE_OUTER_BOUND('',#4069,.T.);
#2565=FACE_OUTER_BOUND('',#4070,.T.);
#2566=FACE_OUTER_BOUND('',#4071,.T.);
#2567=FACE_OUTER_BOUND('',#4072,.T.);
#2568=FACE_OUTER_BOUND('',#4073,.T.);
#2569=FACE_OUTER_BOUND('',#4074,.T.);
#2570=FACE_OUTER_BOUND('',#4075,.T.);
#2571=FACE_OUTER_BOUND('',#4076,.T.);
#2572=FACE_OUTER_BOUND('',#4077,.T.);
#2573=FACE_OUTER_BOUND('',#4078,.T.);
#2574=FACE_OUTER_BOUND('',#4079,.T.);
#2575=FACE_OUTER_BOUND('',#4080,.T.);
#2576=FACE_OUTER_BOUND('',#4081,.T.);
#2577=FACE_OUTER_BOUND('',#4082,.T.);
#2578=FACE_OUTER_BOUND('',#4083,.T.);
#2579=FACE_OUTER_BOUND('',#4084,.T.);
#2580=FACE_OUTER_BOUND('',#4085,.T.);
#2581=FACE_OUTER_BOUND('',#4086,.T.);
#2582=FACE_OUTER_BOUND('',#4087,.T.);
#2583=FACE_OUTER_BOUND('',#4088,.T.);
#2584=FACE_OUTER_BOUND('',#4089,.T.);
#2585=FACE_OUTER_BOUND('',#4090,.T.);
#2586=FACE_OUTER_BOUND('',#4091,.T.);
#2587=FACE_OUTER_BOUND('',#4092,.T.);
#2588=FACE_OUTER_BOUND('',#4093,.T.);
#2589=FACE_OUTER_BOUND('',#4094,.T.);
#2590=FACE_OUTER_BOUND('',#4095,.T.);
#2591=FACE_OUTER_BOUND('',#4096,.T.);
#2592=FACE_OUTER_BOUND('',#4097,.T.);
#2593=FACE_OUTER_BOUND('',#4098,.T.);
#2594=FACE_OUTER_BOUND('',#4099,.T.);
#2595=FACE_OUTER_BOUND('',#4100,.T.);
#2596=FACE_OUTER_BOUND('',#4101,.T.);
#2597=FACE_OUTER_BOUND('',#4102,.T.);
#2598=FACE_OUTER_BOUND('',#4103,.T.);
#2599=FACE_OUTER_BOUND('',#4104,.T.);
#2600=FACE_OUTER_BOUND('',#4105,.T.);
#2601=FACE_OUTER_BOUND('',#4106,.T.);
#2602=FACE_OUTER_BOUND('',#4107,.T.);
#2603=FACE_OUTER_BOUND('',#4108,.T.);
#2604=FACE_OUTER_BOUND('',#4109,.T.);
#2605=FACE_OUTER_BOUND('',#4110,.T.);
#2606=FACE_OUTER_BOUND('',#4111,.T.);
#2607=FACE_OUTER_BOUND('',#4112,.T.);
#2608=FACE_OUTER_BOUND('',#4113,.T.);
#2609=FACE_OUTER_BOUND('',#4114,.T.);
#2610=FACE_OUTER_BOUND('',#4119,.T.);
#2611=FACE_OUTER_BOUND('',#4120,.T.);
#2612=FACE_OUTER_BOUND('',#4121,.T.);
#2613=FACE_OUTER_BOUND('',#4122,.T.);
#2614=FACE_OUTER_BOUND('',#4123,.T.);
#2615=FACE_OUTER_BOUND('',#4124,.T.);
#2616=FACE_OUTER_BOUND('',#4125,.T.);
#2617=FACE_OUTER_BOUND('',#4126,.T.);
#2618=FACE_OUTER_BOUND('',#4127,.T.);
#2619=FACE_OUTER_BOUND('',#4128,.T.);
#2620=FACE_OUTER_BOUND('',#4129,.T.);
#2621=FACE_OUTER_BOUND('',#4130,.T.);
#2622=FACE_OUTER_BOUND('',#4135,.T.);
#2623=FACE_OUTER_BOUND('',#4137,.T.);
#2624=FACE_OUTER_BOUND('',#4138,.T.);
#2625=FACE_OUTER_BOUND('',#4139,.T.);
#2626=FACE_OUTER_BOUND('',#4140,.T.);
#2627=FACE_OUTER_BOUND('',#4141,.T.);
#2628=FACE_OUTER_BOUND('',#4142,.T.);
#2629=FACE_OUTER_BOUND('',#4143,.T.);
#2630=FACE_OUTER_BOUND('',#4144,.T.);
#2631=FACE_OUTER_BOUND('',#4145,.T.);
#2632=FACE_OUTER_BOUND('',#4146,.T.);
#2633=FACE_OUTER_BOUND('',#4147,.T.);
#2634=FACE_OUTER_BOUND('',#4149,.T.);
#2635=FACE_OUTER_BOUND('',#4150,.T.);
#2636=FACE_OUTER_BOUND('',#4151,.T.);
#2637=FACE_OUTER_BOUND('',#4152,.T.);
#2638=FACE_OUTER_BOUND('',#4153,.T.);
#2639=FACE_OUTER_BOUND('',#4154,.T.);
#2640=FACE_OUTER_BOUND('',#4155,.T.);
#2641=FACE_OUTER_BOUND('',#4156,.T.);
#2642=FACE_OUTER_BOUND('',#4157,.T.);
#2643=FACE_OUTER_BOUND('',#4158,.T.);
#2644=FACE_OUTER_BOUND('',#4159,.T.);
#2645=FACE_OUTER_BOUND('',#4161,.T.);
#2646=FACE_OUTER_BOUND('',#4162,.T.);
#2647=FACE_OUTER_BOUND('',#4163,.T.);
#2648=FACE_OUTER_BOUND('',#4164,.T.);
#2649=FACE_OUTER_BOUND('',#4165,.T.);
#2650=FACE_OUTER_BOUND('',#4167,.T.);
#2651=FACE_OUTER_BOUND('',#4168,.T.);
#2652=FACE_OUTER_BOUND('',#4169,.T.);
#2653=FACE_OUTER_BOUND('',#4170,.T.);
#2654=FACE_OUTER_BOUND('',#4176,.T.);
#2655=FACE_OUTER_BOUND('',#4177,.T.);
#2656=FACE_OUTER_BOUND('',#4178,.T.);
#2657=FACE_OUTER_BOUND('',#4179,.T.);
#2658=FACE_OUTER_BOUND('',#4180,.T.);
#2659=FACE_OUTER_BOUND('',#4181,.T.);
#2660=FACE_OUTER_BOUND('',#4182,.T.);
#2661=FACE_OUTER_BOUND('',#4183,.T.);
#2662=FACE_OUTER_BOUND('',#4184,.T.);
#2663=FACE_OUTER_BOUND('',#4185,.T.);
#2664=FACE_OUTER_BOUND('',#4186,.T.);
#2665=FACE_OUTER_BOUND('',#4187,.T.);
#2666=FACE_OUTER_BOUND('',#4188,.T.);
#2667=FACE_OUTER_BOUND('',#4189,.T.);
#2668=FACE_OUTER_BOUND('',#4190,.T.);
#2669=FACE_OUTER_BOUND('',#4191,.T.);
#2670=FACE_OUTER_BOUND('',#4192,.T.);
#2671=FACE_OUTER_BOUND('',#4193,.T.);
#2672=FACE_OUTER_BOUND('',#4194,.T.);
#2673=FACE_OUTER_BOUND('',#4195,.T.);
#2674=FACE_OUTER_BOUND('',#4196,.T.);
#2675=FACE_OUTER_BOUND('',#4197,.T.);
#2676=FACE_OUTER_BOUND('',#4198,.T.);
#2677=FACE_OUTER_BOUND('',#4199,.T.);
#2678=FACE_OUTER_BOUND('',#4200,.T.);
#2679=FACE_OUTER_BOUND('',#4201,.T.);
#2680=FACE_OUTER_BOUND('',#4202,.T.);
#2681=FACE_OUTER_BOUND('',#4203,.T.);
#2682=FACE_OUTER_BOUND('',#4204,.T.);
#2683=FACE_OUTER_BOUND('',#4205,.T.);
#2684=FACE_OUTER_BOUND('',#4206,.T.);
#2685=FACE_OUTER_BOUND('',#4207,.T.);
#2686=FACE_OUTER_BOUND('',#4208,.T.);
#2687=FACE_OUTER_BOUND('',#4209,.T.);
#2688=FACE_OUTER_BOUND('',#4210,.T.);
#2689=FACE_OUTER_BOUND('',#4211,.T.);
#2690=FACE_OUTER_BOUND('',#4212,.T.);
#2691=FACE_OUTER_BOUND('',#4213,.T.);
#2692=FACE_OUTER_BOUND('',#4214,.T.);
#2693=FACE_OUTER_BOUND('',#4215,.T.);
#2694=FACE_OUTER_BOUND('',#4216,.T.);
#2695=FACE_OUTER_BOUND('',#4217,.T.);
#2696=FACE_OUTER_BOUND('',#4218,.T.);
#2697=FACE_OUTER_BOUND('',#4219,.T.);
#2698=FACE_OUTER_BOUND('',#4220,.T.);
#2699=FACE_OUTER_BOUND('',#4221,.T.);
#2700=FACE_OUTER_BOUND('',#4222,.T.);
#2701=FACE_OUTER_BOUND('',#4223,.T.);
#2702=FACE_OUTER_BOUND('',#4224,.T.);
#2703=FACE_OUTER_BOUND('',#4226,.T.);
#2704=FACE_OUTER_BOUND('',#4228,.T.);
#2705=FACE_OUTER_BOUND('',#4229,.T.);
#2706=FACE_OUTER_BOUND('',#4230,.T.);
#2707=FACE_OUTER_BOUND('',#4231,.T.);
#2708=FACE_OUTER_BOUND('',#4232,.T.);
#2709=FACE_OUTER_BOUND('',#4233,.T.);
#2710=FACE_OUTER_BOUND('',#4234,.T.);
#2711=FACE_OUTER_BOUND('',#4235,.T.);
#2712=FACE_OUTER_BOUND('',#4236,.T.);
#2713=FACE_OUTER_BOUND('',#4237,.T.);
#2714=FACE_OUTER_BOUND('',#4238,.T.);
#2715=FACE_OUTER_BOUND('',#4240,.T.);
#2716=FACE_OUTER_BOUND('',#4241,.T.);
#2717=FACE_OUTER_BOUND('',#4242,.T.);
#2718=FACE_OUTER_BOUND('',#4243,.T.);
#2719=FACE_OUTER_BOUND('',#4244,.T.);
#2720=FACE_OUTER_BOUND('',#4245,.T.);
#2721=FACE_OUTER_BOUND('',#4246,.T.);
#2722=FACE_OUTER_BOUND('',#4247,.T.);
#2723=FACE_OUTER_BOUND('',#4248,.T.);
#2724=FACE_OUTER_BOUND('',#4249,.T.);
#2725=FACE_OUTER_BOUND('',#4250,.T.);
#2726=FACE_OUTER_BOUND('',#4252,.T.);
#2727=FACE_OUTER_BOUND('',#4253,.T.);
#2728=FACE_OUTER_BOUND('',#4254,.T.);
#2729=FACE_OUTER_BOUND('',#4255,.T.);
#2730=FACE_OUTER_BOUND('',#4256,.T.);
#2731=FACE_OUTER_BOUND('',#4257,.T.);
#2732=FACE_OUTER_BOUND('',#4258,.T.);
#2733=FACE_OUTER_BOUND('',#4259,.T.);
#2734=FACE_OUTER_BOUND('',#4260,.T.);
#2735=FACE_OUTER_BOUND('',#4261,.T.);
#2736=FACE_OUTER_BOUND('',#4262,.T.);
#2737=FACE_OUTER_BOUND('',#4263,.T.);
#2738=FACE_OUTER_BOUND('',#4269,.T.);
#2739=FACE_OUTER_BOUND('',#4270,.T.);
#2740=FACE_OUTER_BOUND('',#4271,.T.);
#2741=FACE_OUTER_BOUND('',#4272,.T.);
#2742=FACE_OUTER_BOUND('',#4273,.T.);
#2743=FACE_OUTER_BOUND('',#4274,.T.);
#2744=FACE_OUTER_BOUND('',#4275,.T.);
#2745=FACE_OUTER_BOUND('',#4276,.T.);
#2746=FACE_OUTER_BOUND('',#4277,.T.);
#2747=FACE_OUTER_BOUND('',#4278,.T.);
#2748=FACE_OUTER_BOUND('',#4279,.T.);
#2749=FACE_OUTER_BOUND('',#4280,.T.);
#2750=FACE_OUTER_BOUND('',#4281,.T.);
#2751=FACE_OUTER_BOUND('',#4282,.T.);
#2752=FACE_OUTER_BOUND('',#4283,.T.);
#2753=FACE_OUTER_BOUND('',#4284,.T.);
#2754=FACE_OUTER_BOUND('',#4285,.T.);
#2755=FACE_OUTER_BOUND('',#4286,.T.);
#2756=FACE_OUTER_BOUND('',#4287,.T.);
#2757=FACE_OUTER_BOUND('',#4288,.T.);
#2758=FACE_OUTER_BOUND('',#4289,.T.);
#2759=FACE_OUTER_BOUND('',#4290,.T.);
#2760=FACE_OUTER_BOUND('',#4291,.T.);
#2761=FACE_OUTER_BOUND('',#4292,.T.);
#2762=FACE_OUTER_BOUND('',#4293,.T.);
#2763=FACE_OUTER_BOUND('',#4294,.T.);
#2764=FACE_OUTER_BOUND('',#4295,.T.);
#2765=FACE_OUTER_BOUND('',#4296,.T.);
#2766=FACE_OUTER_BOUND('',#4297,.T.);
#2767=FACE_OUTER_BOUND('',#4298,.T.);
#2768=FACE_OUTER_BOUND('',#4299,.T.);
#2769=FACE_OUTER_BOUND('',#4300,.T.);
#2770=FACE_OUTER_BOUND('',#4301,.T.);
#2771=FACE_OUTER_BOUND('',#4302,.T.);
#2772=FACE_OUTER_BOUND('',#4303,.T.);
#2773=FACE_OUTER_BOUND('',#4304,.T.);
#2774=FACE_OUTER_BOUND('',#4305,.T.);
#2775=FACE_OUTER_BOUND('',#4306,.T.);
#2776=FACE_OUTER_BOUND('',#4307,.T.);
#2777=FACE_OUTER_BOUND('',#4308,.T.);
#2778=FACE_OUTER_BOUND('',#4309,.T.);
#2779=FACE_OUTER_BOUND('',#4310,.T.);
#2780=FACE_OUTER_BOUND('',#4311,.T.);
#2781=FACE_OUTER_BOUND('',#4312,.T.);
#2782=FACE_OUTER_BOUND('',#4313,.T.);
#2783=FACE_OUTER_BOUND('',#4314,.T.);
#2784=FACE_OUTER_BOUND('',#4315,.T.);
#2785=FACE_OUTER_BOUND('',#4316,.T.);
#2786=FACE_OUTER_BOUND('',#4317,.T.);
#2787=FACE_OUTER_BOUND('',#4319,.T.);
#2788=FACE_OUTER_BOUND('',#4320,.T.);
#2789=FACE_OUTER_BOUND('',#4321,.T.);
#2790=FACE_OUTER_BOUND('',#4322,.T.);
#2791=FACE_OUTER_BOUND('',#4323,.T.);
#2792=FACE_OUTER_BOUND('',#4324,.T.);
#2793=FACE_OUTER_BOUND('',#4325,.T.);
#2794=FACE_OUTER_BOUND('',#4326,.T.);
#2795=FACE_OUTER_BOUND('',#4334,.T.);
#2796=FACE_OUTER_BOUND('',#4335,.T.);
#2797=FACE_OUTER_BOUND('',#4343,.T.);
#2798=FACE_OUTER_BOUND('',#4344,.T.);
#2799=FACE_OUTER_BOUND('',#4345,.T.);
#2800=FACE_OUTER_BOUND('',#4346,.T.);
#2801=FACE_OUTER_BOUND('',#4347,.T.);
#2802=FACE_OUTER_BOUND('',#4348,.T.);
#2803=FACE_OUTER_BOUND('',#4349,.T.);
#2804=FACE_OUTER_BOUND('',#4350,.T.);
#2805=FACE_OUTER_BOUND('',#4351,.T.);
#2806=FACE_OUTER_BOUND('',#4352,.T.);
#2807=FACE_OUTER_BOUND('',#4353,.T.);
#2808=FACE_OUTER_BOUND('',#4354,.T.);
#2809=FACE_OUTER_BOUND('',#4355,.T.);
#2810=FACE_OUTER_BOUND('',#4356,.T.);
#2811=FACE_OUTER_BOUND('',#4357,.T.);
#2812=FACE_OUTER_BOUND('',#4358,.T.);
#2813=FACE_OUTER_BOUND('',#4365,.T.);
#2814=FACE_OUTER_BOUND('',#4372,.T.);
#2815=FACE_OUTER_BOUND('',#4373,.T.);
#2816=FACE_OUTER_BOUND('',#4374,.T.);
#2817=FACE_OUTER_BOUND('',#4375,.T.);
#2818=FACE_OUTER_BOUND('',#4376,.T.);
#2819=FACE_OUTER_BOUND('',#4377,.T.);
#2820=FACE_OUTER_BOUND('',#4378,.T.);
#2821=FACE_OUTER_BOUND('',#4379,.T.);
#2822=FACE_OUTER_BOUND('',#4380,.T.);
#2823=FACE_OUTER_BOUND('',#4381,.T.);
#2824=FACE_OUTER_BOUND('',#4382,.T.);
#2825=FACE_OUTER_BOUND('',#4389,.T.);
#2826=FACE_OUTER_BOUND('',#4396,.T.);
#2827=FACE_OUTER_BOUND('',#4397,.T.);
#2828=FACE_OUTER_BOUND('',#4398,.T.);
#2829=FACE_OUTER_BOUND('',#4399,.T.);
#2830=FACE_OUTER_BOUND('',#4400,.T.);
#2831=FACE_OUTER_BOUND('',#4401,.T.);
#2832=FACE_OUTER_BOUND('',#4402,.T.);
#2833=FACE_OUTER_BOUND('',#4403,.T.);
#2834=FACE_OUTER_BOUND('',#4404,.T.);
#2835=FACE_OUTER_BOUND('',#4405,.T.);
#2836=FACE_OUTER_BOUND('',#4406,.T.);
#2837=FACE_OUTER_BOUND('',#4407,.T.);
#2838=FACE_OUTER_BOUND('',#4408,.T.);
#2839=FACE_OUTER_BOUND('',#4409,.T.);
#2840=FACE_OUTER_BOUND('',#4410,.T.);
#2841=FACE_OUTER_BOUND('',#4411,.T.);
#2842=FACE_OUTER_BOUND('',#4412,.T.);
#2843=FACE_OUTER_BOUND('',#4413,.T.);
#2844=FACE_OUTER_BOUND('',#4414,.T.);
#2845=FACE_OUTER_BOUND('',#4415,.T.);
#2846=FACE_OUTER_BOUND('',#4416,.T.);
#2847=FACE_OUTER_BOUND('',#4417,.T.);
#2848=FACE_OUTER_BOUND('',#4418,.T.);
#2849=FACE_OUTER_BOUND('',#4419,.T.);
#2850=FACE_OUTER_BOUND('',#4420,.T.);
#2851=FACE_OUTER_BOUND('',#4421,.T.);
#2852=FACE_OUTER_BOUND('',#4422,.T.);
#2853=FACE_OUTER_BOUND('',#4423,.T.);
#2854=FACE_OUTER_BOUND('',#4424,.T.);
#2855=FACE_OUTER_BOUND('',#4425,.T.);
#2856=FACE_OUTER_BOUND('',#4426,.T.);
#2857=FACE_OUTER_BOUND('',#4427,.T.);
#2858=FACE_OUTER_BOUND('',#4428,.T.);
#2859=FACE_OUTER_BOUND('',#4429,.T.);
#2860=FACE_OUTER_BOUND('',#4430,.T.);
#2861=FACE_OUTER_BOUND('',#4431,.T.);
#2862=FACE_OUTER_BOUND('',#4432,.T.);
#2863=FACE_OUTER_BOUND('',#4433,.T.);
#2864=FACE_OUTER_BOUND('',#4434,.T.);
#2865=FACE_OUTER_BOUND('',#4435,.T.);
#2866=FACE_OUTER_BOUND('',#4436,.T.);
#2867=FACE_OUTER_BOUND('',#4437,.T.);
#2868=FACE_OUTER_BOUND('',#4438,.T.);
#2869=FACE_OUTER_BOUND('',#4439,.T.);
#2870=FACE_OUTER_BOUND('',#4440,.T.);
#2871=FACE_OUTER_BOUND('',#4441,.T.);
#2872=FACE_OUTER_BOUND('',#4442,.T.);
#2873=FACE_OUTER_BOUND('',#4443,.T.);
#2874=FACE_OUTER_BOUND('',#4444,.T.);
#2875=FACE_OUTER_BOUND('',#4445,.T.);
#2876=FACE_OUTER_BOUND('',#4446,.T.);
#2877=FACE_OUTER_BOUND('',#4447,.T.);
#2878=FACE_OUTER_BOUND('',#4448,.T.);
#2879=FACE_OUTER_BOUND('',#4449,.T.);
#2880=FACE_OUTER_BOUND('',#4450,.T.);
#2881=FACE_OUTER_BOUND('',#4451,.T.);
#2882=FACE_OUTER_BOUND('',#4452,.T.);
#2883=FACE_OUTER_BOUND('',#4453,.T.);
#2884=FACE_OUTER_BOUND('',#4454,.T.);
#2885=FACE_OUTER_BOUND('',#4455,.T.);
#2886=FACE_OUTER_BOUND('',#4456,.T.);
#2887=FACE_OUTER_BOUND('',#4457,.T.);
#2888=FACE_OUTER_BOUND('',#4458,.T.);
#2889=FACE_OUTER_BOUND('',#4459,.T.);
#2890=FACE_OUTER_BOUND('',#4482,.T.);
#2891=FACE_OUTER_BOUND('',#4483,.T.);
#2892=FACE_OUTER_BOUND('',#4484,.T.);
#2893=FACE_OUTER_BOUND('',#4485,.T.);
#2894=FACE_OUTER_BOUND('',#4496,.T.);
#2895=FACE_OUTER_BOUND('',#4507,.T.);
#2896=FACE_OUTER_BOUND('',#4531,.T.);
#2897=FACE_OUTER_BOUND('',#4532,.T.);
#2898=FACE_OUTER_BOUND('',#4533,.T.);
#2899=FACE_OUTER_BOUND('',#4534,.T.);
#2900=FACE_OUTER_BOUND('',#4535,.T.);
#2901=FACE_OUTER_BOUND('',#4537,.T.);
#2902=FACE_OUTER_BOUND('',#4539,.T.);
#2903=FACE_OUTER_BOUND('',#4541,.T.);
#2904=FACE_OUTER_BOUND('',#4543,.T.);
#2905=FACE_OUTER_BOUND('',#4545,.T.);
#2906=FACE_OUTER_BOUND('',#4547,.T.);
#2907=FACE_OUTER_BOUND('',#4549,.T.);
#2908=FACE_OUTER_BOUND('',#4551,.T.);
#2909=FACE_OUTER_BOUND('',#4553,.T.);
#2910=FACE_OUTER_BOUND('',#4555,.T.);
#2911=FACE_OUTER_BOUND('',#4557,.T.);
#2912=FACE_OUTER_BOUND('',#4559,.T.);
#2913=FACE_OUTER_BOUND('',#4561,.T.);
#2914=FACE_OUTER_BOUND('',#4563,.T.);
#2915=FACE_OUTER_BOUND('',#4565,.T.);
#2916=FACE_OUTER_BOUND('',#4567,.T.);
#2917=FACE_OUTER_BOUND('',#4569,.T.);
#2918=FACE_OUTER_BOUND('',#4570,.T.);
#2919=FACE_OUTER_BOUND('',#4571,.T.);
#2920=FACE_OUTER_BOUND('',#4572,.T.);
#2921=FACE_OUTER_BOUND('',#4573,.T.);
#2922=FACE_OUTER_BOUND('',#4574,.T.);
#2923=FACE_OUTER_BOUND('',#4575,.T.);
#2924=FACE_OUTER_BOUND('',#4576,.T.);
#2925=FACE_OUTER_BOUND('',#4577,.T.);
#2926=FACE_OUTER_BOUND('',#4578,.T.);
#2927=FACE_OUTER_BOUND('',#4579,.T.);
#2928=FACE_OUTER_BOUND('',#4580,.T.);
#2929=FACE_OUTER_BOUND('',#4581,.T.);
#2930=FACE_OUTER_BOUND('',#4582,.T.);
#2931=FACE_OUTER_BOUND('',#4583,.T.);
#2932=FACE_OUTER_BOUND('',#4584,.T.);
#2933=FACE_OUTER_BOUND('',#4585,.T.);
#2934=FACE_OUTER_BOUND('',#4586,.T.);
#2935=FACE_OUTER_BOUND('',#4587,.T.);
#2936=FACE_OUTER_BOUND('',#4588,.T.);
#2937=FACE_OUTER_BOUND('',#4589,.T.);
#2938=FACE_OUTER_BOUND('',#4590,.T.);
#2939=FACE_OUTER_BOUND('',#4591,.T.);
#2940=FACE_OUTER_BOUND('',#4592,.T.);
#2941=FACE_OUTER_BOUND('',#4593,.T.);
#2942=FACE_OUTER_BOUND('',#4594,.T.);
#2943=FACE_OUTER_BOUND('',#4595,.T.);
#2944=FACE_OUTER_BOUND('',#4596,.T.);
#2945=FACE_OUTER_BOUND('',#4597,.T.);
#2946=FACE_OUTER_BOUND('',#4598,.T.);
#2947=FACE_OUTER_BOUND('',#4599,.T.);
#2948=FACE_OUTER_BOUND('',#4600,.T.);
#2949=FACE_OUTER_BOUND('',#4601,.T.);
#2950=FACE_OUTER_BOUND('',#4602,.T.);
#2951=FACE_OUTER_BOUND('',#4603,.T.);
#2952=FACE_OUTER_BOUND('',#4604,.T.);
#2953=FACE_OUTER_BOUND('',#4605,.T.);
#2954=FACE_OUTER_BOUND('',#4606,.T.);
#2955=FACE_OUTER_BOUND('',#4607,.T.);
#2956=FACE_OUTER_BOUND('',#4608,.T.);
#2957=FACE_OUTER_BOUND('',#4609,.T.);
#2958=FACE_OUTER_BOUND('',#4610,.T.);
#2959=FACE_OUTER_BOUND('',#4611,.T.);
#2960=FACE_OUTER_BOUND('',#4612,.T.);
#2961=FACE_OUTER_BOUND('',#4613,.T.);
#2962=FACE_OUTER_BOUND('',#4614,.T.);
#2963=FACE_OUTER_BOUND('',#4615,.T.);
#2964=FACE_OUTER_BOUND('',#4616,.T.);
#2965=FACE_OUTER_BOUND('',#4617,.T.);
#2966=FACE_OUTER_BOUND('',#4618,.T.);
#2967=FACE_OUTER_BOUND('',#4619,.T.);
#2968=FACE_OUTER_BOUND('',#4620,.T.);
#2969=FACE_OUTER_BOUND('',#4621,.T.);
#2970=FACE_OUTER_BOUND('',#4622,.T.);
#2971=FACE_OUTER_BOUND('',#4623,.T.);
#2972=FACE_OUTER_BOUND('',#4624,.T.);
#2973=FACE_OUTER_BOUND('',#4625,.T.);
#2974=FACE_OUTER_BOUND('',#4626,.T.);
#2975=FACE_OUTER_BOUND('',#4627,.T.);
#2976=FACE_OUTER_BOUND('',#4628,.T.);
#2977=FACE_OUTER_BOUND('',#4637,.T.);
#2978=FACE_OUTER_BOUND('',#4638,.T.);
#2979=FACE_OUTER_BOUND('',#4639,.T.);
#2980=FACE_OUTER_BOUND('',#4640,.T.);
#2981=FACE_OUTER_BOUND('',#4641,.T.);
#2982=FACE_OUTER_BOUND('',#4642,.T.);
#2983=FACE_OUTER_BOUND('',#4643,.T.);
#2984=FACE_OUTER_BOUND('',#4644,.T.);
#2985=FACE_OUTER_BOUND('',#4645,.T.);
#2986=FACE_OUTER_BOUND('',#4646,.T.);
#2987=FACE_OUTER_BOUND('',#4647,.T.);
#2988=FACE_OUTER_BOUND('',#4648,.T.);
#2989=FACE_OUTER_BOUND('',#4649,.T.);
#2990=FACE_OUTER_BOUND('',#4650,.T.);
#2991=FACE_OUTER_BOUND('',#4651,.T.);
#2992=FACE_OUTER_BOUND('',#4652,.T.);
#2993=FACE_OUTER_BOUND('',#4653,.T.);
#2994=FACE_OUTER_BOUND('',#4654,.T.);
#2995=FACE_OUTER_BOUND('',#4655,.T.);
#2996=FACE_OUTER_BOUND('',#4656,.T.);
#2997=FACE_OUTER_BOUND('',#4657,.T.);
#2998=FACE_OUTER_BOUND('',#4658,.T.);
#2999=FACE_OUTER_BOUND('',#4659,.T.);
#3000=FACE_OUTER_BOUND('',#4660,.T.);
#3001=FACE_OUTER_BOUND('',#4661,.T.);
#3002=FACE_OUTER_BOUND('',#4662,.T.);
#3003=FACE_OUTER_BOUND('',#4663,.T.);
#3004=FACE_OUTER_BOUND('',#4664,.T.);
#3005=FACE_OUTER_BOUND('',#4665,.T.);
#3006=FACE_OUTER_BOUND('',#4666,.T.);
#3007=FACE_OUTER_BOUND('',#4667,.T.);
#3008=FACE_OUTER_BOUND('',#4668,.T.);
#3009=FACE_OUTER_BOUND('',#4669,.T.);
#3010=FACE_OUTER_BOUND('',#4670,.T.);
#3011=FACE_OUTER_BOUND('',#4671,.T.);
#3012=FACE_OUTER_BOUND('',#4672,.T.);
#3013=FACE_OUTER_BOUND('',#4673,.T.);
#3014=FACE_OUTER_BOUND('',#4674,.T.);
#3015=FACE_OUTER_BOUND('',#4676,.T.);
#3016=FACE_OUTER_BOUND('',#4678,.T.);
#3017=FACE_OUTER_BOUND('',#4680,.T.);
#3018=FACE_OUTER_BOUND('',#4682,.T.);
#3019=FACE_OUTER_BOUND('',#4684,.T.);
#3020=FACE_OUTER_BOUND('',#4686,.T.);
#3021=FACE_OUTER_BOUND('',#4688,.T.);
#3022=FACE_OUTER_BOUND('',#4690,.T.);
#3023=FACE_OUTER_BOUND('',#4691,.T.);
#3024=FACE_OUTER_BOUND('',#4692,.T.);
#3025=FACE_OUTER_BOUND('',#4693,.T.);
#3026=FACE_OUTER_BOUND('',#4694,.T.);
#3027=FACE_OUTER_BOUND('',#4695,.T.);
#3028=FACE_OUTER_BOUND('',#4696,.T.);
#3029=FACE_OUTER_BOUND('',#4697,.T.);
#3030=FACE_OUTER_BOUND('',#4698,.T.);
#3031=FACE_OUTER_BOUND('',#4699,.T.);
#3032=FACE_OUTER_BOUND('',#4700,.T.);
#3033=FACE_OUTER_BOUND('',#4701,.T.);
#3034=FACE_OUTER_BOUND('',#4702,.T.);
#3035=FACE_OUTER_BOUND('',#4703,.T.);
#3036=FACE_OUTER_BOUND('',#4704,.T.);
#3037=FACE_OUTER_BOUND('',#4705,.T.);
#3038=FACE_OUTER_BOUND('',#4706,.T.);
#3039=FACE_OUTER_BOUND('',#4707,.T.);
#3040=FACE_OUTER_BOUND('',#4708,.T.);
#3041=FACE_OUTER_BOUND('',#4709,.T.);
#3042=FACE_OUTER_BOUND('',#4710,.T.);
#3043=FACE_OUTER_BOUND('',#4711,.T.);
#3044=FACE_OUTER_BOUND('',#4712,.T.);
#3045=FACE_OUTER_BOUND('',#4713,.T.);
#3046=FACE_OUTER_BOUND('',#4714,.T.);
#3047=FACE_OUTER_BOUND('',#4715,.T.);
#3048=FACE_OUTER_BOUND('',#4716,.T.);
#3049=FACE_OUTER_BOUND('',#4717,.T.);
#3050=FACE_OUTER_BOUND('',#4718,.T.);
#3051=FACE_OUTER_BOUND('',#4719,.T.);
#3052=FACE_OUTER_BOUND('',#4720,.T.);
#3053=FACE_OUTER_BOUND('',#4721,.T.);
#3054=FACE_OUTER_BOUND('',#4722,.T.);
#3055=FACE_OUTER_BOUND('',#4723,.T.);
#3056=FACE_OUTER_BOUND('',#4724,.T.);
#3057=FACE_OUTER_BOUND('',#4725,.T.);
#3058=FACE_OUTER_BOUND('',#4726,.T.);
#3059=FACE_OUTER_BOUND('',#4727,.T.);
#3060=FACE_OUTER_BOUND('',#4728,.T.);
#3061=FACE_OUTER_BOUND('',#4729,.T.);
#3062=FACE_OUTER_BOUND('',#4730,.T.);
#3063=FACE_OUTER_BOUND('',#4731,.T.);
#3064=FACE_OUTER_BOUND('',#4732,.T.);
#3065=FACE_OUTER_BOUND('',#4733,.T.);
#3066=FACE_OUTER_BOUND('',#4734,.T.);
#3067=FACE_OUTER_BOUND('',#4735,.T.);
#3068=FACE_OUTER_BOUND('',#4736,.T.);
#3069=FACE_OUTER_BOUND('',#4737,.T.);
#3070=FACE_OUTER_BOUND('',#4738,.T.);
#3071=FACE_OUTER_BOUND('',#4739,.T.);
#3072=FACE_OUTER_BOUND('',#4740,.T.);
#3073=FACE_OUTER_BOUND('',#4741,.T.);
#3074=FACE_OUTER_BOUND('',#4742,.T.);
#3075=FACE_OUTER_BOUND('',#4743,.T.);
#3076=FACE_OUTER_BOUND('',#4744,.T.);
#3077=FACE_OUTER_BOUND('',#4745,.T.);
#3078=FACE_OUTER_BOUND('',#4746,.T.);
#3079=FACE_OUTER_BOUND('',#4747,.T.);
#3080=FACE_OUTER_BOUND('',#4748,.T.);
#3081=FACE_OUTER_BOUND('',#4749,.T.);
#3082=FACE_OUTER_BOUND('',#4750,.T.);
#3083=FACE_OUTER_BOUND('',#4752,.T.);
#3084=FACE_OUTER_BOUND('',#4753,.T.);
#3085=FACE_OUTER_BOUND('',#4755,.T.);
#3086=FACE_OUTER_BOUND('',#4756,.T.);
#3087=FACE_OUTER_BOUND('',#4757,.T.);
#3088=FACE_OUTER_BOUND('',#4758,.T.);
#3089=FACE_OUTER_BOUND('',#4759,.T.);
#3090=FACE_OUTER_BOUND('',#4760,.T.);
#3091=FACE_OUTER_BOUND('',#4761,.T.);
#3092=FACE_OUTER_BOUND('',#4762,.T.);
#3093=FACE_OUTER_BOUND('',#4763,.T.);
#3094=FACE_OUTER_BOUND('',#4764,.T.);
#3095=FACE_OUTER_BOUND('',#4765,.T.);
#3096=FACE_OUTER_BOUND('',#4766,.T.);
#3097=FACE_OUTER_BOUND('',#4767,.T.);
#3098=FACE_OUTER_BOUND('',#4768,.T.);
#3099=FACE_OUTER_BOUND('',#4770,.T.);
#3100=FACE_OUTER_BOUND('',#4771,.T.);
#3101=FACE_OUTER_BOUND('',#4772,.T.);
#3102=FACE_OUTER_BOUND('',#4773,.T.);
#3103=FACE_OUTER_BOUND('',#4774,.T.);
#3104=FACE_OUTER_BOUND('',#4775,.T.);
#3105=FACE_OUTER_BOUND('',#4776,.T.);
#3106=FACE_OUTER_BOUND('',#4777,.T.);
#3107=FACE_OUTER_BOUND('',#4778,.T.);
#3108=FACE_OUTER_BOUND('',#4779,.T.);
#3109=FACE_OUTER_BOUND('',#4780,.T.);
#3110=FACE_OUTER_BOUND('',#4781,.T.);
#3111=FACE_OUTER_BOUND('',#4782,.T.);
#3112=FACE_OUTER_BOUND('',#4783,.T.);
#3113=FACE_OUTER_BOUND('',#4784,.T.);
#3114=FACE_OUTER_BOUND('',#4785,.T.);
#3115=FACE_OUTER_BOUND('',#4786,.T.);
#3116=FACE_OUTER_BOUND('',#4787,.T.);
#3117=FACE_OUTER_BOUND('',#4788,.T.);
#3118=FACE_OUTER_BOUND('',#4789,.T.);
#3119=FACE_OUTER_BOUND('',#4790,.T.);
#3120=FACE_OUTER_BOUND('',#4791,.T.);
#3121=FACE_OUTER_BOUND('',#4792,.T.);
#3122=FACE_OUTER_BOUND('',#4793,.T.);
#3123=FACE_OUTER_BOUND('',#4794,.T.);
#3124=FACE_OUTER_BOUND('',#4795,.T.);
#3125=FACE_OUTER_BOUND('',#4796,.T.);
#3126=FACE_OUTER_BOUND('',#4797,.T.);
#3127=FACE_OUTER_BOUND('',#4798,.T.);
#3128=FACE_OUTER_BOUND('',#4799,.T.);
#3129=FACE_OUTER_BOUND('',#4800,.T.);
#3130=FACE_OUTER_BOUND('',#4801,.T.);
#3131=FACE_OUTER_BOUND('',#4802,.T.);
#3132=FACE_OUTER_BOUND('',#4803,.T.);
#3133=FACE_OUTER_BOUND('',#4804,.T.);
#3134=FACE_OUTER_BOUND('',#4805,.T.);
#3135=FACE_OUTER_BOUND('',#4806,.T.);
#3136=FACE_OUTER_BOUND('',#4807,.T.);
#3137=FACE_OUTER_BOUND('',#4808,.T.);
#3138=FACE_OUTER_BOUND('',#4809,.T.);
#3139=FACE_OUTER_BOUND('',#4810,.T.);
#3140=FACE_OUTER_BOUND('',#4811,.T.);
#3141=FACE_OUTER_BOUND('',#4812,.T.);
#3142=FACE_OUTER_BOUND('',#4813,.T.);
#3143=FACE_OUTER_BOUND('',#4814,.T.);
#3144=FACE_OUTER_BOUND('',#4815,.T.);
#3145=FACE_OUTER_BOUND('',#4816,.T.);
#3146=FACE_OUTER_BOUND('',#4817,.T.);
#3147=FACE_OUTER_BOUND('',#4818,.T.);
#3148=FACE_OUTER_BOUND('',#4819,.T.);
#3149=FACE_OUTER_BOUND('',#4820,.T.);
#3150=FACE_OUTER_BOUND('',#4821,.T.);
#3151=FACE_OUTER_BOUND('',#4822,.T.);
#3152=FACE_OUTER_BOUND('',#4823,.T.);
#3153=FACE_OUTER_BOUND('',#4824,.T.);
#3154=FACE_OUTER_BOUND('',#4825,.T.);
#3155=FACE_OUTER_BOUND('',#4826,.T.);
#3156=FACE_OUTER_BOUND('',#4827,.T.);
#3157=FACE_OUTER_BOUND('',#4828,.T.);
#3158=FACE_OUTER_BOUND('',#4829,.T.);
#3159=FACE_OUTER_BOUND('',#4830,.T.);
#3160=FACE_OUTER_BOUND('',#4831,.T.);
#3161=FACE_OUTER_BOUND('',#4832,.T.);
#3162=FACE_OUTER_BOUND('',#4833,.T.);
#3163=FACE_OUTER_BOUND('',#4834,.T.);
#3164=FACE_OUTER_BOUND('',#4835,.T.);
#3165=FACE_OUTER_BOUND('',#4836,.T.);
#3166=FACE_OUTER_BOUND('',#4837,.T.);
#3167=FACE_OUTER_BOUND('',#4838,.T.);
#3168=FACE_OUTER_BOUND('',#4839,.T.);
#3169=FACE_OUTER_BOUND('',#4840,.T.);
#3170=FACE_OUTER_BOUND('',#4841,.T.);
#3171=FACE_OUTER_BOUND('',#4842,.T.);
#3172=FACE_OUTER_BOUND('',#4843,.T.);
#3173=FACE_OUTER_BOUND('',#4844,.T.);
#3174=FACE_OUTER_BOUND('',#4845,.T.);
#3175=FACE_OUTER_BOUND('',#4846,.T.);
#3176=FACE_OUTER_BOUND('',#4847,.T.);
#3177=FACE_OUTER_BOUND('',#4848,.T.);
#3178=FACE_OUTER_BOUND('',#4849,.T.);
#3179=FACE_OUTER_BOUND('',#4850,.T.);
#3180=FACE_OUTER_BOUND('',#4851,.T.);
#3181=FACE_OUTER_BOUND('',#4852,.T.);
#3182=FACE_OUTER_BOUND('',#4853,.T.);
#3183=FACE_OUTER_BOUND('',#4854,.T.);
#3184=FACE_OUTER_BOUND('',#4855,.T.);
#3185=FACE_OUTER_BOUND('',#4856,.T.);
#3186=FACE_OUTER_BOUND('',#4857,.T.);
#3187=FACE_OUTER_BOUND('',#4858,.T.);
#3188=FACE_OUTER_BOUND('',#4859,.T.);
#3189=FACE_OUTER_BOUND('',#4860,.T.);
#3190=FACE_OUTER_BOUND('',#4861,.T.);
#3191=FACE_OUTER_BOUND('',#4862,.T.);
#3192=FACE_OUTER_BOUND('',#4863,.T.);
#3193=FACE_OUTER_BOUND('',#4864,.T.);
#3194=FACE_OUTER_BOUND('',#4865,.T.);
#3195=FACE_OUTER_BOUND('',#4866,.T.);
#3196=FACE_OUTER_BOUND('',#4868,.T.);
#3197=FACE_OUTER_BOUND('',#4869,.T.);
#3198=FACE_OUTER_BOUND('',#4870,.T.);
#3199=FACE_OUTER_BOUND('',#4871,.T.);
#3200=FACE_OUTER_BOUND('',#4872,.T.);
#3201=FACE_OUTER_BOUND('',#4873,.T.);
#3202=FACE_OUTER_BOUND('',#4874,.T.);
#3203=FACE_OUTER_BOUND('',#4875,.T.);
#3204=FACE_OUTER_BOUND('',#4876,.T.);
#3205=FACE_OUTER_BOUND('',#4877,.T.);
#3206=FACE_OUTER_BOUND('',#4878,.T.);
#3207=FACE_OUTER_BOUND('',#4879,.T.);
#3208=FACE_OUTER_BOUND('',#4881,.T.);
#3209=FACE_OUTER_BOUND('',#4882,.T.);
#3210=FACE_OUTER_BOUND('',#4883,.T.);
#3211=FACE_OUTER_BOUND('',#4884,.T.);
#3212=FACE_OUTER_BOUND('',#4885,.T.);
#3213=FACE_OUTER_BOUND('',#4886,.T.);
#3214=FACE_OUTER_BOUND('',#4887,.T.);
#3215=FACE_OUTER_BOUND('',#4889,.T.);
#3216=FACE_OUTER_BOUND('',#4890,.T.);
#3217=FACE_OUTER_BOUND('',#4892,.T.);
#3218=FACE_OUTER_BOUND('',#4893,.T.);
#3219=FACE_OUTER_BOUND('',#4894,.T.);
#3220=FACE_OUTER_BOUND('',#4895,.T.);
#3221=FACE_OUTER_BOUND('',#4897,.T.);
#3222=FACE_OUTER_BOUND('',#4898,.T.);
#3223=FACE_OUTER_BOUND('',#4899,.T.);
#3224=FACE_OUTER_BOUND('',#4900,.T.);
#3225=FACE_OUTER_BOUND('',#4901,.T.);
#3226=FACE_OUTER_BOUND('',#4902,.T.);
#3227=FACE_OUTER_BOUND('',#4903,.T.);
#3228=FACE_OUTER_BOUND('',#4904,.T.);
#3229=FACE_OUTER_BOUND('',#4905,.T.);
#3230=FACE_OUTER_BOUND('',#4906,.T.);
#3231=FACE_OUTER_BOUND('',#4907,.T.);
#3232=FACE_OUTER_BOUND('',#4908,.T.);
#3233=FACE_OUTER_BOUND('',#4909,.T.);
#3234=FACE_OUTER_BOUND('',#4910,.T.);
#3235=FACE_OUTER_BOUND('',#4911,.T.);
#3236=FACE_OUTER_BOUND('',#4912,.T.);
#3237=FACE_OUTER_BOUND('',#4913,.T.);
#3238=FACE_OUTER_BOUND('',#4914,.T.);
#3239=FACE_OUTER_BOUND('',#4915,.T.);
#3240=FACE_OUTER_BOUND('',#4916,.T.);
#3241=FACE_OUTER_BOUND('',#4917,.T.);
#3242=FACE_OUTER_BOUND('',#4918,.T.);
#3243=FACE_OUTER_BOUND('',#4919,.T.);
#3244=FACE_OUTER_BOUND('',#4920,.T.);
#3245=FACE_OUTER_BOUND('',#4921,.T.);
#3246=FACE_OUTER_BOUND('',#4922,.T.);
#3247=FACE_OUTER_BOUND('',#4923,.T.);
#3248=FACE_OUTER_BOUND('',#4924,.T.);
#3249=FACE_OUTER_BOUND('',#4925,.T.);
#3250=FACE_OUTER_BOUND('',#4926,.T.);
#3251=FACE_OUTER_BOUND('',#4927,.T.);
#3252=FACE_OUTER_BOUND('',#4928,.T.);
#3253=FACE_OUTER_BOUND('',#4929,.T.);
#3254=FACE_OUTER_BOUND('',#4930,.T.);
#3255=FACE_OUTER_BOUND('',#4931,.T.);
#3256=FACE_OUTER_BOUND('',#4932,.T.);
#3257=FACE_OUTER_BOUND('',#4933,.T.);
#3258=FACE_OUTER_BOUND('',#4934,.T.);
#3259=FACE_OUTER_BOUND('',#4935,.T.);
#3260=FACE_OUTER_BOUND('',#4936,.T.);
#3261=FACE_OUTER_BOUND('',#4937,.T.);
#3262=FACE_OUTER_BOUND('',#4938,.T.);
#3263=FACE_OUTER_BOUND('',#4939,.T.);
#3264=FACE_OUTER_BOUND('',#4940,.T.);
#3265=FACE_OUTER_BOUND('',#4941,.T.);
#3266=FACE_OUTER_BOUND('',#4942,.T.);
#3267=FACE_OUTER_BOUND('',#4943,.T.);
#3268=FACE_OUTER_BOUND('',#4945,.T.);
#3269=FACE_OUTER_BOUND('',#4946,.T.);
#3270=FACE_OUTER_BOUND('',#4947,.T.);
#3271=FACE_OUTER_BOUND('',#4948,.T.);
#3272=FACE_OUTER_BOUND('',#4950,.T.);
#3273=FACE_OUTER_BOUND('',#4952,.T.);
#3274=FACE_OUTER_BOUND('',#4953,.T.);
#3275=FACE_OUTER_BOUND('',#4954,.T.);
#3276=FACE_OUTER_BOUND('',#4955,.T.);
#3277=FACE_OUTER_BOUND('',#4956,.T.);
#3278=FACE_OUTER_BOUND('',#4957,.T.);
#3279=FACE_OUTER_BOUND('',#4960,.T.);
#3280=FACE_OUTER_BOUND('',#4961,.T.);
#3281=FACE_OUTER_BOUND('',#4962,.T.);
#3282=FACE_OUTER_BOUND('',#4963,.T.);
#3283=FACE_OUTER_BOUND('',#4964,.T.);
#3284=FACE_OUTER_BOUND('',#4965,.T.);
#3285=FACE_OUTER_BOUND('',#4966,.T.);
#3286=FACE_OUTER_BOUND('',#4967,.T.);
#3287=FACE_OUTER_BOUND('',#4970,.T.);
#3288=FACE_OUTER_BOUND('',#4971,.T.);
#3289=FACE_OUTER_BOUND('',#4972,.T.);
#3290=FACE_OUTER_BOUND('',#4973,.T.);
#3291=FACE_OUTER_BOUND('',#4974,.T.);
#3292=FACE_OUTER_BOUND('',#4976,.T.);
#3293=FACE_OUTER_BOUND('',#4977,.T.);
#3294=FACE_OUTER_BOUND('',#4978,.T.);
#3295=FACE_OUTER_BOUND('',#4979,.T.);
#3296=FACE_OUTER_BOUND('',#4980,.T.);
#3297=FACE_OUTER_BOUND('',#4982,.T.);
#3298=FACE_OUTER_BOUND('',#4983,.T.);
#3299=FACE_OUTER_BOUND('',#4984,.T.);
#3300=FACE_OUTER_BOUND('',#4985,.T.);
#3301=FACE_OUTER_BOUND('',#4986,.T.);
#3302=FACE_OUTER_BOUND('',#4987,.T.);
#3303=FACE_OUTER_BOUND('',#4989,.T.);
#3304=FACE_OUTER_BOUND('',#4990,.T.);
#3305=FACE_OUTER_BOUND('',#4991,.T.);
#3306=FACE_OUTER_BOUND('',#4992,.T.);
#3307=FACE_OUTER_BOUND('',#4994,.T.);
#3308=FACE_OUTER_BOUND('',#4995,.T.);
#3309=FACE_OUTER_BOUND('',#4996,.T.);
#3310=FACE_OUTER_BOUND('',#4997,.T.);
#3311=FACE_OUTER_BOUND('',#4998,.T.);
#3312=FACE_OUTER_BOUND('',#4999,.T.);
#3313=FACE_OUTER_BOUND('',#5000,.T.);
#3314=FACE_OUTER_BOUND('',#5001,.T.);
#3315=FACE_OUTER_BOUND('',#5002,.T.);
#3316=FACE_OUTER_BOUND('',#5003,.T.);
#3317=FACE_OUTER_BOUND('',#5004,.T.);
#3318=FACE_OUTER_BOUND('',#5005,.T.);
#3319=FACE_OUTER_BOUND('',#5006,.T.);
#3320=FACE_OUTER_BOUND('',#5007,.T.);
#3321=FACE_OUTER_BOUND('',#5008,.T.);
#3322=FACE_OUTER_BOUND('',#5009,.T.);
#3323=FACE_OUTER_BOUND('',#5010,.T.);
#3324=FACE_OUTER_BOUND('',#5011,.T.);
#3325=FACE_OUTER_BOUND('',#5012,.T.);
#3326=FACE_OUTER_BOUND('',#5013,.T.);
#3327=FACE_OUTER_BOUND('',#5014,.T.);
#3328=FACE_OUTER_BOUND('',#5015,.T.);
#3329=FACE_OUTER_BOUND('',#5016,.T.);
#3330=FACE_OUTER_BOUND('',#5017,.T.);
#3331=FACE_OUTER_BOUND('',#5018,.T.);
#3332=FACE_OUTER_BOUND('',#5019,.T.);
#3333=FACE_OUTER_BOUND('',#5020,.T.);
#3334=FACE_OUTER_BOUND('',#5021,.T.);
#3335=FACE_OUTER_BOUND('',#5022,.T.);
#3336=FACE_OUTER_BOUND('',#5023,.T.);
#3337=FACE_OUTER_BOUND('',#5024,.T.);
#3338=FACE_OUTER_BOUND('',#5025,.T.);
#3339=FACE_OUTER_BOUND('',#5026,.T.);
#3340=FACE_OUTER_BOUND('',#5027,.T.);
#3341=FACE_OUTER_BOUND('',#5029,.T.);
#3342=FACE_OUTER_BOUND('',#5030,.T.);
#3343=FACE_OUTER_BOUND('',#5031,.T.);
#3344=FACE_OUTER_BOUND('',#5032,.T.);
#3345=FACE_OUTER_BOUND('',#5033,.T.);
#3346=FACE_OUTER_BOUND('',#5034,.T.);
#3347=FACE_OUTER_BOUND('',#5035,.T.);
#3348=FACE_OUTER_BOUND('',#5036,.T.);
#3349=FACE_OUTER_BOUND('',#5037,.T.);
#3350=FACE_OUTER_BOUND('',#5038,.T.);
#3351=FACE_OUTER_BOUND('',#5039,.T.);
#3352=FACE_OUTER_BOUND('',#5041,.T.);
#3353=FACE_OUTER_BOUND('',#5043,.T.);
#3354=FACE_OUTER_BOUND('',#5044,.T.);
#3355=FACE_OUTER_BOUND('',#5045,.T.);
#3356=FACE_OUTER_BOUND('',#5046,.T.);
#3357=FACE_OUTER_BOUND('',#5047,.T.);
#3358=FACE_OUTER_BOUND('',#5048,.T.);
#3359=FACE_OUTER_BOUND('',#5049,.T.);
#3360=FACE_OUTER_BOUND('',#5050,.T.);
#3361=FACE_OUTER_BOUND('',#5051,.T.);
#3362=FACE_OUTER_BOUND('',#5052,.T.);
#3363=FACE_OUTER_BOUND('',#5053,.T.);
#3364=FACE_OUTER_BOUND('',#5054,.T.);
#3365=FACE_OUTER_BOUND('',#5055,.T.);
#3366=FACE_OUTER_BOUND('',#5056,.T.);
#3367=FACE_OUTER_BOUND('',#5057,.T.);
#3368=FACE_OUTER_BOUND('',#5058,.T.);
#3369=FACE_OUTER_BOUND('',#5059,.T.);
#3370=FACE_OUTER_BOUND('',#5060,.T.);
#3371=FACE_OUTER_BOUND('',#5062,.T.);
#3372=FACE_OUTER_BOUND('',#5064,.T.);
#3373=FACE_OUTER_BOUND('',#5065,.T.);
#3374=FACE_OUTER_BOUND('',#5066,.T.);
#3375=FACE_OUTER_BOUND('',#5067,.T.);
#3376=FACE_OUTER_BOUND('',#5068,.T.);
#3377=FACE_OUTER_BOUND('',#5069,.T.);
#3378=FACE_OUTER_BOUND('',#5070,.T.);
#3379=FACE_OUTER_BOUND('',#5071,.T.);
#3380=FACE_OUTER_BOUND('',#5072,.T.);
#3381=FACE_OUTER_BOUND('',#5073,.T.);
#3382=FACE_OUTER_BOUND('',#5074,.T.);
#3383=FACE_OUTER_BOUND('',#5075,.T.);
#3384=FACE_OUTER_BOUND('',#5076,.T.);
#3385=FACE_OUTER_BOUND('',#5077,.T.);
#3386=FACE_OUTER_BOUND('',#5078,.T.);
#3387=FACE_OUTER_BOUND('',#5079,.T.);
#3388=FACE_OUTER_BOUND('',#5080,.T.);
#3389=FACE_OUTER_BOUND('',#5081,.T.);
#3390=FACE_OUTER_BOUND('',#5082,.T.);
#3391=FACE_OUTER_BOUND('',#5083,.T.);
#3392=FACE_OUTER_BOUND('',#5084,.T.);
#3393=FACE_OUTER_BOUND('',#5085,.T.);
#3394=FACE_OUTER_BOUND('',#5086,.T.);
#3395=FACE_OUTER_BOUND('',#5087,.T.);
#3396=FACE_OUTER_BOUND('',#5088,.T.);
#3397=FACE_OUTER_BOUND('',#5089,.T.);
#3398=FACE_OUTER_BOUND('',#5090,.T.);
#3399=FACE_OUTER_BOUND('',#5091,.T.);
#3400=FACE_OUTER_BOUND('',#5092,.T.);
#3401=FACE_OUTER_BOUND('',#5093,.T.);
#3402=FACE_OUTER_BOUND('',#5095,.T.);
#3403=FACE_OUTER_BOUND('',#5096,.T.);
#3404=FACE_OUTER_BOUND('',#5097,.T.);
#3405=FACE_OUTER_BOUND('',#5098,.T.);
#3406=FACE_OUTER_BOUND('',#5099,.T.);
#3407=FACE_OUTER_BOUND('',#5100,.T.);
#3408=FACE_OUTER_BOUND('',#5101,.T.);
#3409=FACE_OUTER_BOUND('',#5102,.T.);
#3410=FACE_OUTER_BOUND('',#5103,.T.);
#3411=FACE_OUTER_BOUND('',#5104,.T.);
#3412=FACE_OUTER_BOUND('',#5105,.T.);
#3413=FACE_OUTER_BOUND('',#5106,.T.);
#3414=FACE_OUTER_BOUND('',#5107,.T.);
#3415=FACE_OUTER_BOUND('',#5108,.T.);
#3416=FACE_OUTER_BOUND('',#5109,.T.);
#3417=FACE_OUTER_BOUND('',#5110,.T.);
#3418=FACE_OUTER_BOUND('',#5111,.T.);
#3419=FACE_OUTER_BOUND('',#5112,.T.);
#3420=FACE_OUTER_BOUND('',#5113,.T.);
#3421=FACE_OUTER_BOUND('',#5114,.T.);
#3422=FACE_OUTER_BOUND('',#5115,.T.);
#3423=FACE_OUTER_BOUND('',#5116,.T.);
#3424=FACE_OUTER_BOUND('',#5117,.T.);
#3425=FACE_OUTER_BOUND('',#5118,.T.);
#3426=FACE_OUTER_BOUND('',#5119,.T.);
#3427=FACE_OUTER_BOUND('',#5128,.T.);
#3428=FACE_OUTER_BOUND('',#5129,.T.);
#3429=FACE_OUTER_BOUND('',#5130,.T.);
#3430=FACE_OUTER_BOUND('',#5131,.T.);
#3431=FACE_OUTER_BOUND('',#5132,.T.);
#3432=FACE_OUTER_BOUND('',#5133,.T.);
#3433=FACE_OUTER_BOUND('',#5134,.T.);
#3434=FACE_OUTER_BOUND('',#5135,.T.);
#3435=FACE_OUTER_BOUND('',#5136,.T.);
#3436=FACE_OUTER_BOUND('',#5138,.T.);
#3437=FACE_OUTER_BOUND('',#5139,.T.);
#3438=FACE_OUTER_BOUND('',#5141,.T.);
#3439=FACE_OUTER_BOUND('',#5143,.T.);
#3440=FACE_OUTER_BOUND('',#5144,.T.);
#3441=FACE_OUTER_BOUND('',#5145,.T.);
#3442=FACE_OUTER_BOUND('',#5146,.T.);
#3443=FACE_OUTER_BOUND('',#5147,.T.);
#3444=FACE_OUTER_BOUND('',#5148,.T.);
#3445=FACE_OUTER_BOUND('',#5149,.T.);
#3446=FACE_OUTER_BOUND('',#5150,.T.);
#3447=FACE_OUTER_BOUND('',#5151,.T.);
#3448=FACE_OUTER_BOUND('',#5152,.T.);
#3449=FACE_OUTER_BOUND('',#5153,.T.);
#3450=FACE_OUTER_BOUND('',#5154,.T.);
#3451=FACE_OUTER_BOUND('',#5155,.T.);
#3452=FACE_OUTER_BOUND('',#5156,.T.);
#3453=FACE_OUTER_BOUND('',#5157,.T.);
#3454=FACE_OUTER_BOUND('',#5159,.T.);
#3455=FACE_OUTER_BOUND('',#5161,.T.);
#3456=FACE_OUTER_BOUND('',#5162,.T.);
#3457=FACE_OUTER_BOUND('',#5163,.T.);
#3458=FACE_OUTER_BOUND('',#5164,.T.);
#3459=FACE_OUTER_BOUND('',#5165,.T.);
#3460=FACE_OUTER_BOUND('',#5166,.T.);
#3461=FACE_OUTER_BOUND('',#5167,.T.);
#3462=FACE_OUTER_BOUND('',#5168,.T.);
#3463=FACE_OUTER_BOUND('',#5169,.T.);
#3464=FACE_OUTER_BOUND('',#5170,.T.);
#3465=FACE_OUTER_BOUND('',#5171,.T.);
#3466=FACE_OUTER_BOUND('',#5172,.T.);
#3467=FACE_OUTER_BOUND('',#5174,.T.);
#3468=FACE_OUTER_BOUND('',#5176,.T.);
#3469=FACE_OUTER_BOUND('',#5177,.T.);
#3470=FACE_OUTER_BOUND('',#5178,.T.);
#3471=FACE_OUTER_BOUND('',#5179,.T.);
#3472=FACE_OUTER_BOUND('',#5180,.T.);
#3473=FACE_OUTER_BOUND('',#5181,.T.);
#3474=FACE_OUTER_BOUND('',#5182,.T.);
#3475=FACE_OUTER_BOUND('',#5183,.T.);
#3476=FACE_OUTER_BOUND('',#5184,.T.);
#3477=FACE_OUTER_BOUND('',#5185,.T.);
#3478=FACE_OUTER_BOUND('',#5186,.T.);
#3479=FACE_OUTER_BOUND('',#5187,.T.);
#3480=FACE_OUTER_BOUND('',#5188,.T.);
#3481=FACE_OUTER_BOUND('',#5190,.T.);
#3482=FACE_OUTER_BOUND('',#5191,.T.);
#3483=FACE_OUTER_BOUND('',#5193,.T.);
#3484=FACE_OUTER_BOUND('',#5195,.T.);
#3485=FACE_OUTER_BOUND('',#5196,.T.);
#3486=FACE_OUTER_BOUND('',#5197,.T.);
#3487=FACE_OUTER_BOUND('',#5198,.T.);
#3488=FACE_OUTER_BOUND('',#5199,.T.);
#3489=FACE_OUTER_BOUND('',#5200,.T.);
#3490=FACE_OUTER_BOUND('',#5201,.T.);
#3491=FACE_OUTER_BOUND('',#5202,.T.);
#3492=FACE_OUTER_BOUND('',#5203,.T.);
#3493=FACE_OUTER_BOUND('',#5204,.T.);
#3494=FACE_OUTER_BOUND('',#5205,.T.);
#3495=FACE_OUTER_BOUND('',#5206,.T.);
#3496=FACE_OUTER_BOUND('',#5207,.T.);
#3497=FACE_OUTER_BOUND('',#5208,.T.);
#3498=FACE_OUTER_BOUND('',#5209,.T.);
#3499=FACE_OUTER_BOUND('',#5211,.T.);
#3500=FACE_OUTER_BOUND('',#5213,.T.);
#3501=FACE_OUTER_BOUND('',#5214,.T.);
#3502=FACE_OUTER_BOUND('',#5215,.T.);
#3503=FACE_OUTER_BOUND('',#5216,.T.);
#3504=FACE_OUTER_BOUND('',#5217,.T.);
#3505=FACE_OUTER_BOUND('',#5218,.T.);
#3506=FACE_OUTER_BOUND('',#5219,.T.);
#3507=FACE_OUTER_BOUND('',#5220,.T.);
#3508=FACE_OUTER_BOUND('',#5221,.T.);
#3509=FACE_OUTER_BOUND('',#5222,.T.);
#3510=FACE_OUTER_BOUND('',#5223,.T.);
#3511=FACE_OUTER_BOUND('',#5224,.T.);
#3512=FACE_OUTER_BOUND('',#5226,.T.);
#3513=FACE_OUTER_BOUND('',#5228,.T.);
#3514=FACE_OUTER_BOUND('',#5229,.T.);
#3515=FACE_OUTER_BOUND('',#5230,.T.);
#3516=FACE_OUTER_BOUND('',#5231,.T.);
#3517=FACE_OUTER_BOUND('',#5232,.T.);
#3518=FACE_OUTER_BOUND('',#5233,.T.);
#3519=FACE_OUTER_BOUND('',#5234,.T.);
#3520=FACE_OUTER_BOUND('',#5235,.T.);
#3521=FACE_OUTER_BOUND('',#5236,.T.);
#3522=FACE_OUTER_BOUND('',#5237,.T.);
#3523=FACE_OUTER_BOUND('',#5238,.T.);
#3524=FACE_OUTER_BOUND('',#5239,.T.);
#3525=FACE_OUTER_BOUND('',#5240,.T.);
#3526=FACE_OUTER_BOUND('',#5242,.T.);
#3527=FACE_OUTER_BOUND('',#5244,.T.);
#3528=FACE_OUTER_BOUND('',#5245,.T.);
#3529=FACE_OUTER_BOUND('',#5246,.T.);
#3530=FACE_OUTER_BOUND('',#5247,.T.);
#3531=FACE_OUTER_BOUND('',#5248,.T.);
#3532=FACE_OUTER_BOUND('',#5249,.T.);
#3533=FACE_OUTER_BOUND('',#5250,.T.);
#3534=EDGE_LOOP('',(#15916,#15917,#15918,#15919));
#3535=EDGE_LOOP('',(#15920,#15921,#15922,#15923));
#3536=EDGE_LOOP('',(#15924,#15925,#15926,#15927));
#3537=EDGE_LOOP('',(#15928,#15929,#15930,#15931));
#3538=EDGE_LOOP('',(#15932,#15933,#15934,#15935));
#3539=EDGE_LOOP('',(#15936,#15937,#15938,#15939));
#3540=EDGE_LOOP('',(#15940,#15941,#15942,#15943));
#3541=EDGE_LOOP('',(#15944,#15945,#15946,#15947));
#3542=EDGE_LOOP('',(#15948,#15949,#15950,#15951));
#3543=EDGE_LOOP('',(#15952,#15953,#15954));
#3544=EDGE_LOOP('',(#15955,#15956,#15957,#15958));
#3545=EDGE_LOOP('',(#15959,#15960,#15961));
#3546=EDGE_LOOP('',(#15962,#15963,#15964,#15965));
#3547=EDGE_LOOP('',(#15966,#15967,#15968));
#3548=EDGE_LOOP('',(#15969,#15970,#15971,#15972));
#3549=EDGE_LOOP('',(#15973,#15974,#15975));
#3550=EDGE_LOOP('',(#15976,#15977,#15978,#15979));
#3551=EDGE_LOOP('',(#15980,#15981,#15982,#15983));
#3552=EDGE_LOOP('',(#15984,#15985,#15986,#15987));
#3553=EDGE_LOOP('',(#15988));
#3554=EDGE_LOOP('',(#15989));
#3555=EDGE_LOOP('',(#15990));
#3556=EDGE_LOOP('',(#15991));
#3557=EDGE_LOOP('',(#15992,#15993,#15994,#15995));
#3558=EDGE_LOOP('',(#15996,#15997,#15998,#15999));
#3559=EDGE_LOOP('',(#16000,#16001,#16002,#16003,#16004,#16005,#16006,#16007));
#3560=EDGE_LOOP('',(#16008));
#3561=EDGE_LOOP('',(#16009));
#3562=EDGE_LOOP('',(#16010));
#3563=EDGE_LOOP('',(#16011));
#3564=EDGE_LOOP('',(#16012));
#3565=EDGE_LOOP('',(#16013));
#3566=EDGE_LOOP('',(#16014));
#3567=EDGE_LOOP('',(#16015));
#3568=EDGE_LOOP('',(#16016,#16017,#16018,#16019,#16020,#16021,#16022,#16023));
#3569=EDGE_LOOP('',(#16024));
#3570=EDGE_LOOP('',(#16025));
#3571=EDGE_LOOP('',(#16026));
#3572=EDGE_LOOP('',(#16027));
#3573=EDGE_LOOP('',(#16028));
#3574=EDGE_LOOP('',(#16029));
#3575=EDGE_LOOP('',(#16030));
#3576=EDGE_LOOP('',(#16031));
#3577=EDGE_LOOP('',(#16032,#16033,#16034,#16035));
#3578=EDGE_LOOP('',(#16036,#16037,#16038,#16039));
#3579=EDGE_LOOP('',(#16040,#16041,#16042,#16043));
#3580=EDGE_LOOP('',(#16044,#16045,#16046,#16047,#16048,#16049,#16050,#16051));
#3581=EDGE_LOOP('',(#16052,#16053,#16054,#16055));
#3582=EDGE_LOOP('',(#16056,#16057,#16058,#16059));
#3583=EDGE_LOOP('',(#16060,#16061,#16062,#16063));
#3584=EDGE_LOOP('',(#16064,#16065,#16066,#16067));
#3585=EDGE_LOOP('',(#16068,#16069,#16070,#16071));
#3586=EDGE_LOOP('',(#16072,#16073,#16074,#16075,#16076));
#3587=EDGE_LOOP('',(#16077,#16078,#16079,#16080,#16081));
#3588=EDGE_LOOP('',(#16082,#16083,#16084,#16085));
#3589=EDGE_LOOP('',(#16086,#16087,#16088,#16089));
#3590=EDGE_LOOP('',(#16090,#16091,#16092,#16093));
#3591=EDGE_LOOP('',(#16094,#16095,#16096,#16097,#16098));
#3592=EDGE_LOOP('',(#16099,#16100,#16101,#16102,#16103));
#3593=EDGE_LOOP('',(#16104));
#3594=EDGE_LOOP('',(#16105));
#3595=EDGE_LOOP('',(#16106));
#3596=EDGE_LOOP('',(#16107));
#3597=EDGE_LOOP('',(#16108));
#3598=EDGE_LOOP('',(#16109));
#3599=EDGE_LOOP('',(#16110));
#3600=EDGE_LOOP('',(#16111));
#3601=EDGE_LOOP('',(#16112));
#3602=EDGE_LOOP('',(#16113));
#3603=EDGE_LOOP('',(#16114,#16115,#16116,#16117,#16118));
#3604=EDGE_LOOP('',(#16119,#16120,#16121,#16122));
#3605=EDGE_LOOP('',(#16123));
#3606=EDGE_LOOP('',(#16124,#16125,#16126,#16127,#16128));
#3607=EDGE_LOOP('',(#16129,#16130,#16131,#16132,#16133));
#3608=EDGE_LOOP('',(#16134,#16135,#16136,#16137));
#3609=EDGE_LOOP('',(#16138,#16139,#16140,#16141));
#3610=EDGE_LOOP('',(#16142,#16143,#16144,#16145));
#3611=EDGE_LOOP('',(#16146,#16147,#16148,#16149));
#3612=EDGE_LOOP('',(#16150,#16151,#16152,#16153));
#3613=EDGE_LOOP('',(#16154,#16155,#16156,#16157));
#3614=EDGE_LOOP('',(#16158,#16159,#16160,#16161));
#3615=EDGE_LOOP('',(#16162,#16163,#16164,#16165));
#3616=EDGE_LOOP('',(#16166,#16167,#16168,#16169));
#3617=EDGE_LOOP('',(#16170,#16171,#16172,#16173));
#3618=EDGE_LOOP('',(#16174,#16175,#16176,#16177));
#3619=EDGE_LOOP('',(#16178,#16179,#16180,#16181));
#3620=EDGE_LOOP('',(#16182,#16183,#16184,#16185));
#3621=EDGE_LOOP('',(#16186));
#3622=EDGE_LOOP('',(#16187,#16188,#16189,#16190));
#3623=EDGE_LOOP('',(#16191,#16192,#16193,#16194));
#3624=EDGE_LOOP('',(#16195,#16196,#16197,#16198));
#3625=EDGE_LOOP('',(#16199,#16200,#16201,#16202));
#3626=EDGE_LOOP('',(#16203));
#3627=EDGE_LOOP('',(#16204));
#3628=EDGE_LOOP('',(#16205));
#3629=EDGE_LOOP('',(#16206));
#3630=EDGE_LOOP('',(#16207));
#3631=EDGE_LOOP('',(#16208));
#3632=EDGE_LOOP('',(#16209));
#3633=EDGE_LOOP('',(#16210,#16211,#16212,#16213));
#3634=EDGE_LOOP('',(#16214,#16215,#16216,#16217));
#3635=EDGE_LOOP('',(#16218,#16219,#16220,#16221));
#3636=EDGE_LOOP('',(#16222));
#3637=EDGE_LOOP('',(#16223,#16224,#16225,#16226));
#3638=EDGE_LOOP('',(#16227,#16228,#16229,#16230));
#3639=EDGE_LOOP('',(#16231,#16232,#16233,#16234));
#3640=EDGE_LOOP('',(#16235,#16236,#16237,#16238));
#3641=EDGE_LOOP('',(#16239));
#3642=EDGE_LOOP('',(#16240));
#3643=EDGE_LOOP('',(#16241));
#3644=EDGE_LOOP('',(#16242));
#3645=EDGE_LOOP('',(#16243));
#3646=EDGE_LOOP('',(#16244));
#3647=EDGE_LOOP('',(#16245));
#3648=EDGE_LOOP('',(#16246));
#3649=EDGE_LOOP('',(#16247));
#3650=EDGE_LOOP('',(#16248));
#3651=EDGE_LOOP('',(#16249));
#3652=EDGE_LOOP('',(#16250));
#3653=EDGE_LOOP('',(#16251));
#3654=EDGE_LOOP('',(#16252));
#3655=EDGE_LOOP('',(#16253));
#3656=EDGE_LOOP('',(#16254));
#3657=EDGE_LOOP('',(#16255));
#3658=EDGE_LOOP('',(#16256,#16257,#16258,#16259,#16260,#16261,#16262,#16263));
#3659=EDGE_LOOP('',(#16264,#16265,#16266,#16267,#16268,#16269,#16270,#16271));
#3660=EDGE_LOOP('',(#16272,#16273,#16274,#16275));
#3661=EDGE_LOOP('',(#16276,#16277,#16278,#16279));
#3662=EDGE_LOOP('',(#16280,#16281,#16282,#16283));
#3663=EDGE_LOOP('',(#16284,#16285,#16286,#16287));
#3664=EDGE_LOOP('',(#16288,#16289,#16290,#16291));
#3665=EDGE_LOOP('',(#16292,#16293,#16294,#16295));
#3666=EDGE_LOOP('',(#16296,#16297,#16298,#16299));
#3667=EDGE_LOOP('',(#16300,#16301,#16302,#16303,#16304,#16305,#16306,#16307));
#3668=EDGE_LOOP('',(#16308,#16309,#16310,#16311,#16312,#16313,#16314,#16315));
#3669=EDGE_LOOP('',(#16316,#16317,#16318,#16319,#16320,#16321,#16322,#16323));
#3670=EDGE_LOOP('',(#16324,#16325,#16326,#16327,#16328,#16329,#16330,#16331));
#3671=EDGE_LOOP('',(#16332,#16333,#16334,#16335));
#3672=EDGE_LOOP('',(#16336,#16337,#16338,#16339));
#3673=EDGE_LOOP('',(#16340,#16341,#16342,#16343));
#3674=EDGE_LOOP('',(#16344,#16345,#16346,#16347));
#3675=EDGE_LOOP('',(#16348,#16349,#16350,#16351));
#3676=EDGE_LOOP('',(#16352,#16353,#16354,#16355));
#3677=EDGE_LOOP('',(#16356,#16357,#16358,#16359));
#3678=EDGE_LOOP('',(#16360,#16361,#16362,#16363));
#3679=EDGE_LOOP('',(#16364));
#3680=EDGE_LOOP('',(#16365));
#3681=EDGE_LOOP('',(#16366));
#3682=EDGE_LOOP('',(#16367));
#3683=EDGE_LOOP('',(#16368));
#3684=EDGE_LOOP('',(#16369));
#3685=EDGE_LOOP('',(#16370));
#3686=EDGE_LOOP('',(#16371));
#3687=EDGE_LOOP('',(#16372,#16373,#16374,#16375,#16376,#16377,#16378,#16379,
#16380,#16381,#16382,#16383));
#3688=EDGE_LOOP('',(#16384,#16385,#16386,#16387,#16388,#16389,#16390,#16391));
#3689=EDGE_LOOP('',(#16392,#16393,#16394,#16395));
#3690=EDGE_LOOP('',(#16396));
#3691=EDGE_LOOP('',(#16397,#16398,#16399,#16400));
#3692=EDGE_LOOP('',(#16401,#16402,#16403,#16404));
#3693=EDGE_LOOP('',(#16405,#16406,#16407,#16408));
#3694=EDGE_LOOP('',(#16409));
#3695=EDGE_LOOP('',(#16410));
#3696=EDGE_LOOP('',(#16411,#16412,#16413,#16414));
#3697=EDGE_LOOP('',(#16415,#16416,#16417,#16418));
#3698=EDGE_LOOP('',(#16419,#16420,#16421,#16422));
#3699=EDGE_LOOP('',(#16423));
#3700=EDGE_LOOP('',(#16424,#16425,#16426,#16427));
#3701=EDGE_LOOP('',(#16428,#16429,#16430,#16431));
#3702=EDGE_LOOP('',(#16432,#16433,#16434,#16435));
#3703=EDGE_LOOP('',(#16436,#16437,#16438,#16439));
#3704=EDGE_LOOP('',(#16440,#16441,#16442,#16443));
#3705=EDGE_LOOP('',(#16444,#16445,#16446,#16447,#16448,#16449,#16450,#16451,
#16452,#16453,#16454,#16455));
#3706=EDGE_LOOP('',(#16456));
#3707=EDGE_LOOP('',(#16457,#16458,#16459,#16460,#16461,#16462,#16463,#16464));
#3708=EDGE_LOOP('',(#16465));
#3709=EDGE_LOOP('',(#16466));
#3710=EDGE_LOOP('',(#16467));
#3711=EDGE_LOOP('',(#16468));
#3712=EDGE_LOOP('',(#16469));
#3713=EDGE_LOOP('',(#16470,#16471,#16472,#16473));
#3714=EDGE_LOOP('',(#16474,#16475,#16476,#16477));
#3715=EDGE_LOOP('',(#16478,#16479,#16480,#16481));
#3716=EDGE_LOOP('',(#16482,#16483,#16484,#16485));
#3717=EDGE_LOOP('',(#16486,#16487,#16488,#16489));
#3718=EDGE_LOOP('',(#16490,#16491,#16492,#16493));
#3719=EDGE_LOOP('',(#16494,#16495,#16496,#16497));
#3720=EDGE_LOOP('',(#16498,#16499,#16500,#16501));
#3721=EDGE_LOOP('',(#16502));
#3722=EDGE_LOOP('',(#16503,#16504,#16505,#16506,#16507,#16508));
#3723=EDGE_LOOP('',(#16509));
#3724=EDGE_LOOP('',(#16510,#16511,#16512,#16513,#16514,#16515));
#3725=EDGE_LOOP('',(#16516));
#3726=EDGE_LOOP('',(#16517,#16518,#16519,#16520,#16521,#16522));
#3727=EDGE_LOOP('',(#16523));
#3728=EDGE_LOOP('',(#16524,#16525,#16526,#16527,#16528,#16529));
#3729=EDGE_LOOP('',(#16530,#16531,#16532,#16533,#16534));
#3730=EDGE_LOOP('',(#16535,#16536,#16537,#16538,#16539));
#3731=EDGE_LOOP('',(#16540,#16541,#16542,#16543,#16544));
#3732=EDGE_LOOP('',(#16545,#16546,#16547,#16548,#16549));
#3733=EDGE_LOOP('',(#16550,#16551,#16552,#16553,#16554));
#3734=EDGE_LOOP('',(#16555,#16556,#16557,#16558,#16559));
#3735=EDGE_LOOP('',(#16560,#16561,#16562));
#3736=EDGE_LOOP('',(#16563,#16564,#16565));
#3737=EDGE_LOOP('',(#16566,#16567,#16568));
#3738=EDGE_LOOP('',(#16569,#16570,#16571));
#3739=EDGE_LOOP('',(#16572,#16573,#16574));
#3740=EDGE_LOOP('',(#16575,#16576,#16577));
#3741=EDGE_LOOP('',(#16578,#16579,#16580,#16581,#16582));
#3742=EDGE_LOOP('',(#16583,#16584,#16585,#16586,#16587));
#3743=EDGE_LOOP('',(#16588,#16589,#16590,#16591,#16592));
#3744=EDGE_LOOP('',(#16593,#16594,#16595,#16596,#16597));
#3745=EDGE_LOOP('',(#16598,#16599,#16600,#16601,#16602));
#3746=EDGE_LOOP('',(#16603,#16604,#16605,#16606,#16607));
#3747=EDGE_LOOP('',(#16608,#16609,#16610));
#3748=EDGE_LOOP('',(#16611,#16612,#16613));
#3749=EDGE_LOOP('',(#16614,#16615,#16616));
#3750=EDGE_LOOP('',(#16617,#16618,#16619));
#3751=EDGE_LOOP('',(#16620,#16621,#16622));
#3752=EDGE_LOOP('',(#16623,#16624,#16625));
#3753=EDGE_LOOP('',(#16626,#16627,#16628,#16629,#16630));
#3754=EDGE_LOOP('',(#16631,#16632,#16633,#16634,#16635));
#3755=EDGE_LOOP('',(#16636,#16637,#16638,#16639,#16640));
#3756=EDGE_LOOP('',(#16641,#16642,#16643,#16644,#16645));
#3757=EDGE_LOOP('',(#16646,#16647,#16648,#16649,#16650));
#3758=EDGE_LOOP('',(#16651,#16652,#16653,#16654,#16655));
#3759=EDGE_LOOP('',(#16656,#16657,#16658));
#3760=EDGE_LOOP('',(#16659,#16660,#16661));
#3761=EDGE_LOOP('',(#16662,#16663,#16664));
#3762=EDGE_LOOP('',(#16665,#16666,#16667));
#3763=EDGE_LOOP('',(#16668,#16669,#16670));
#3764=EDGE_LOOP('',(#16671,#16672,#16673));
#3765=EDGE_LOOP('',(#16674,#16675,#16676,#16677,#16678));
#3766=EDGE_LOOP('',(#16679,#16680,#16681,#16682,#16683));
#3767=EDGE_LOOP('',(#16684,#16685,#16686,#16687,#16688));
#3768=EDGE_LOOP('',(#16689,#16690,#16691,#16692,#16693));
#3769=EDGE_LOOP('',(#16694,#16695,#16696,#16697,#16698));
#3770=EDGE_LOOP('',(#16699,#16700,#16701,#16702,#16703));
#3771=EDGE_LOOP('',(#16704,#16705,#16706));
#3772=EDGE_LOOP('',(#16707,#16708,#16709));
#3773=EDGE_LOOP('',(#16710,#16711,#16712));
#3774=EDGE_LOOP('',(#16713,#16714,#16715));
#3775=EDGE_LOOP('',(#16716,#16717,#16718));
#3776=EDGE_LOOP('',(#16719,#16720,#16721));
#3777=EDGE_LOOP('',(#16722));
#3778=EDGE_LOOP('',(#16723));
#3779=EDGE_LOOP('',(#16724));
#3780=EDGE_LOOP('',(#16725));
#3781=EDGE_LOOP('',(#16726));
#3782=EDGE_LOOP('',(#16727));
#3783=EDGE_LOOP('',(#16728));
#3784=EDGE_LOOP('',(#16729));
#3785=EDGE_LOOP('',(#16730,#16731,#16732,#16733));
#3786=EDGE_LOOP('',(#16734,#16735,#16736,#16737,#16738));
#3787=EDGE_LOOP('',(#16739,#16740,#16741,#16742));
#3788=EDGE_LOOP('',(#16743,#16744,#16745,#16746,#16747));
#3789=EDGE_LOOP('',(#16748));
#3790=EDGE_LOOP('',(#16749,#16750,#16751,#16752));
#3791=EDGE_LOOP('',(#16753,#16754,#16755,#16756));
#3792=EDGE_LOOP('',(#16757,#16758,#16759,#16760));
#3793=EDGE_LOOP('',(#16761,#16762,#16763,#16764));
#3794=EDGE_LOOP('',(#16765,#16766,#16767,#16768));
#3795=EDGE_LOOP('',(#16769));
#3796=EDGE_LOOP('',(#16770));
#3797=EDGE_LOOP('',(#16771));
#3798=EDGE_LOOP('',(#16772,#16773,#16774,#16775,#16776,#16777,#16778,#16779));
#3799=EDGE_LOOP('',(#16780));
#3800=EDGE_LOOP('',(#16781,#16782,#16783,#16784,#16785,#16786,#16787,#16788));
#3801=EDGE_LOOP('',(#16789));
#3802=EDGE_LOOP('',(#16790,#16791,#16792,#16793));
#3803=EDGE_LOOP('',(#16794,#16795,#16796,#16797));
#3804=EDGE_LOOP('',(#16798,#16799,#16800,#16801));
#3805=EDGE_LOOP('',(#16802,#16803,#16804,#16805));
#3806=EDGE_LOOP('',(#16806,#16807,#16808,#16809));
#3807=EDGE_LOOP('',(#16810,#16811,#16812,#16813,#16814));
#3808=EDGE_LOOP('',(#16815,#16816,#16817,#16818,#16819));
#3809=EDGE_LOOP('',(#16820));
#3810=EDGE_LOOP('',(#16821));
#3811=EDGE_LOOP('',(#16822,#16823,#16824,#16825,#16826,#16827));
#3812=EDGE_LOOP('',(#16828,#16829,#16830,#16831));
#3813=EDGE_LOOP('',(#16832,#16833,#16834,#16835));
#3814=EDGE_LOOP('',(#16836,#16837,#16838,#16839));
#3815=EDGE_LOOP('',(#16840,#16841,#16842,#16843));
#3816=EDGE_LOOP('',(#16844,#16845,#16846,#16847));
#3817=EDGE_LOOP('',(#16848,#16849,#16850,#16851));
#3818=EDGE_LOOP('',(#16852,#16853,#16854,#16855,#16856,#16857));
#3819=EDGE_LOOP('',(#16858,#16859,#16860,#16861));
#3820=EDGE_LOOP('',(#16862,#16863,#16864,#16865));
#3821=EDGE_LOOP('',(#16866));
#3822=EDGE_LOOP('',(#16867));
#3823=EDGE_LOOP('',(#16868));
#3824=EDGE_LOOP('',(#16869));
#3825=EDGE_LOOP('',(#16870,#16871,#16872,#16873));
#3826=EDGE_LOOP('',(#16874,#16875,#16876,#16877));
#3827=EDGE_LOOP('',(#16878,#16879,#16880,#16881));
#3828=EDGE_LOOP('',(#16882,#16883,#16884,#16885,#16886,#16887,#16888,#16889,
#16890,#16891,#16892,#16893));
#3829=EDGE_LOOP('',(#16894));
#3830=EDGE_LOOP('',(#16895,#16896,#16897,#16898,#16899,#16900,#16901,#16902,
#16903,#16904,#16905,#16906));
#3831=EDGE_LOOP('',(#16907));
#3832=EDGE_LOOP('',(#16908,#16909,#16910,#16911));
#3833=EDGE_LOOP('',(#16912));
#3834=EDGE_LOOP('',(#16913,#16914,#16915,#16916));
#3835=EDGE_LOOP('',(#16917,#16918,#16919,#16920));
#3836=EDGE_LOOP('',(#16921,#16922,#16923,#16924));
#3837=EDGE_LOOP('',(#16925));
#3838=EDGE_LOOP('',(#16926));
#3839=EDGE_LOOP('',(#16927,#16928,#16929,#16930));
#3840=EDGE_LOOP('',(#16931,#16932,#16933,#16934));
#3841=EDGE_LOOP('',(#16935,#16936,#16937,#16938));
#3842=EDGE_LOOP('',(#16939));
#3843=EDGE_LOOP('',(#16940,#16941,#16942,#16943));
#3844=EDGE_LOOP('',(#16944,#16945,#16946,#16947));
#3845=EDGE_LOOP('',(#16948,#16949,#16950,#16951));
#3846=EDGE_LOOP('',(#16952,#16953,#16954,#16955));
#3847=EDGE_LOOP('',(#16956,#16957,#16958,#16959));
#3848=EDGE_LOOP('',(#16960,#16961,#16962,#16963));
#3849=EDGE_LOOP('',(#16964,#16965,#16966,#16967));
#3850=EDGE_LOOP('',(#16968,#16969,#16970,#16971));
#3851=EDGE_LOOP('',(#16972,#16973,#16974,#16975));
#3852=EDGE_LOOP('',(#16976,#16977,#16978,#16979));
#3853=EDGE_LOOP('',(#16980,#16981,#16982,#16983));
#3854=EDGE_LOOP('',(#16984,#16985,#16986,#16987));
#3855=EDGE_LOOP('',(#16988,#16989,#16990,#16991));
#3856=EDGE_LOOP('',(#16992,#16993,#16994,#16995));
#3857=EDGE_LOOP('',(#16996,#16997,#16998,#16999));
#3858=EDGE_LOOP('',(#17000));
#3859=EDGE_LOOP('',(#17001));
#3860=EDGE_LOOP('',(#17002));
#3861=EDGE_LOOP('',(#17003));
#3862=EDGE_LOOP('',(#17004));
#3863=EDGE_LOOP('',(#17005));
#3864=EDGE_LOOP('',(#17006));
#3865=EDGE_LOOP('',(#17007));
#3866=EDGE_LOOP('',(#17008));
#3867=EDGE_LOOP('',(#17009));
#3868=EDGE_LOOP('',(#17010));
#3869=EDGE_LOOP('',(#17011));
#3870=EDGE_LOOP('',(#17012,#17013,#17014,#17015));
#3871=EDGE_LOOP('',(#17016,#17017,#17018,#17019));
#3872=EDGE_LOOP('',(#17020,#17021,#17022,#17023));
#3873=EDGE_LOOP('',(#17024,#17025,#17026,#17027));
#3874=EDGE_LOOP('',(#17028,#17029,#17030,#17031,#17032,#17033,#17034,#17035,
#17036,#17037,#17038,#17039));
#3875=EDGE_LOOP('',(#17040));
#3876=EDGE_LOOP('',(#17041));
#3877=EDGE_LOOP('',(#17042,#17043,#17044,#17045,#17046,#17047,#17048,#17049,
#17050,#17051,#17052,#17053));
#3878=EDGE_LOOP('',(#17054));
#3879=EDGE_LOOP('',(#17055));
#3880=EDGE_LOOP('',(#17056,#17057,#17058,#17059));
#3881=EDGE_LOOP('',(#17060,#17061,#17062,#17063));
#3882=EDGE_LOOP('',(#17064,#17065,#17066,#17067));
#3883=EDGE_LOOP('',(#17068,#17069,#17070,#17071));
#3884=EDGE_LOOP('',(#17072,#17073,#17074,#17075));
#3885=EDGE_LOOP('',(#17076,#17077,#17078,#17079));
#3886=EDGE_LOOP('',(#17080,#17081,#17082,#17083));
#3887=EDGE_LOOP('',(#17084,#17085,#17086,#17087));
#3888=EDGE_LOOP('',(#17088,#17089,#17090,#17091));
#3889=EDGE_LOOP('',(#17092,#17093,#17094,#17095));
#3890=EDGE_LOOP('',(#17096,#17097,#17098,#17099));
#3891=EDGE_LOOP('',(#17100,#17101,#17102,#17103));
#3892=EDGE_LOOP('',(#17104,#17105,#17106,#17107));
#3893=EDGE_LOOP('',(#17108,#17109,#17110,#17111));
#3894=EDGE_LOOP('',(#17112,#17113,#17114,#17115));
#3895=EDGE_LOOP('',(#17116,#17117,#17118,#17119,#17120,#17121));
#3896=EDGE_LOOP('',(#17122,#17123,#17124,#17125,#17126,#17127));
#3897=EDGE_LOOP('',(#17128,#17129,#17130,#17131,#17132,#17133));
#3898=EDGE_LOOP('',(#17134,#17135,#17136,#17137,#17138,#17139));
#3899=EDGE_LOOP('',(#17140,#17141,#17142,#17143));
#3900=EDGE_LOOP('',(#17144,#17145,#17146,#17147));
#3901=EDGE_LOOP('',(#17148));
#3902=EDGE_LOOP('',(#17149));
#3903=EDGE_LOOP('',(#17150));
#3904=EDGE_LOOP('',(#17151));
#3905=EDGE_LOOP('',(#17152,#17153,#17154,#17155));
#3906=EDGE_LOOP('',(#17156,#17157,#17158,#17159));
#3907=EDGE_LOOP('',(#17160,#17161,#17162,#17163));
#3908=EDGE_LOOP('',(#17164,#17165,#17166,#17167));
#3909=EDGE_LOOP('',(#17168,#17169,#17170,#17171,#17172,#17173,#17174,#17175));
#3910=EDGE_LOOP('',(#17176));
#3911=EDGE_LOOP('',(#17177));
#3912=EDGE_LOOP('',(#17178));
#3913=EDGE_LOOP('',(#17179));
#3914=EDGE_LOOP('',(#17180,#17181,#17182,#17183));
#3915=EDGE_LOOP('',(#17184,#17185,#17186,#17187));
#3916=EDGE_LOOP('',(#17188,#17189,#17190,#17191));
#3917=EDGE_LOOP('',(#17192,#17193,#17194,#17195));
#3918=EDGE_LOOP('',(#17196,#17197,#17198,#17199));
#3919=EDGE_LOOP('',(#17200,#17201,#17202,#17203,#17204,#17205));
#3920=EDGE_LOOP('',(#17206,#17207,#17208,#17209,#17210,#17211));
#3921=EDGE_LOOP('',(#17212,#17213,#17214,#17215,#17216,#17217));
#3922=EDGE_LOOP('',(#17218,#17219,#17220,#17221,#17222,#17223));
#3923=EDGE_LOOP('',(#17224,#17225,#17226,#17227));
#3924=EDGE_LOOP('',(#17228,#17229,#17230,#17231));
#3925=EDGE_LOOP('',(#17232));
#3926=EDGE_LOOP('',(#17233));
#3927=EDGE_LOOP('',(#17234));
#3928=EDGE_LOOP('',(#17235));
#3929=EDGE_LOOP('',(#17236,#17237,#17238,#17239));
#3930=EDGE_LOOP('',(#17240,#17241,#17242,#17243));
#3931=EDGE_LOOP('',(#17244,#17245,#17246,#17247));
#3932=EDGE_LOOP('',(#17248,#17249,#17250,#17251));
#3933=EDGE_LOOP('',(#17252,#17253,#17254,#17255,#17256,#17257,#17258,#17259));
#3934=EDGE_LOOP('',(#17260));
#3935=EDGE_LOOP('',(#17261));
#3936=EDGE_LOOP('',(#17262));
#3937=EDGE_LOOP('',(#17263));
#3938=EDGE_LOOP('',(#17264,#17265,#17266,#17267));
#3939=EDGE_LOOP('',(#17268,#17269,#17270,#17271));
#3940=EDGE_LOOP('',(#17272,#17273,#17274,#17275));
#3941=EDGE_LOOP('',(#17276,#17277,#17278,#17279));
#3942=EDGE_LOOP('',(#17280,#17281,#17282,#17283));
#3943=EDGE_LOOP('',(#17284,#17285,#17286,#17287));
#3944=EDGE_LOOP('',(#17288,#17289,#17290,#17291));
#3945=EDGE_LOOP('',(#17292,#17293,#17294,#17295));
#3946=EDGE_LOOP('',(#17296,#17297,#17298,#17299));
#3947=EDGE_LOOP('',(#17300,#17301,#17302,#17303));
#3948=EDGE_LOOP('',(#17304,#17305,#17306,#17307));
#3949=EDGE_LOOP('',(#17308,#17309,#17310,#17311));
#3950=EDGE_LOOP('',(#17312,#17313,#17314,#17315));
#3951=EDGE_LOOP('',(#17316));
#3952=EDGE_LOOP('',(#17317));
#3953=EDGE_LOOP('',(#17318));
#3954=EDGE_LOOP('',(#17319));
#3955=EDGE_LOOP('',(#17320));
#3956=EDGE_LOOP('',(#17321));
#3957=EDGE_LOOP('',(#17322));
#3958=EDGE_LOOP('',(#17323));
#3959=EDGE_LOOP('',(#17324));
#3960=EDGE_LOOP('',(#17325,#17326,#17327,#17328));
#3961=EDGE_LOOP('',(#17329,#17330,#17331,#17332));
#3962=EDGE_LOOP('',(#17333,#17334,#17335,#17336));
#3963=EDGE_LOOP('',(#17337,#17338,#17339,#17340));
#3964=EDGE_LOOP('',(#17341,#17342,#17343,#17344));
#3965=EDGE_LOOP('',(#17345));
#3966=EDGE_LOOP('',(#17346));
#3967=EDGE_LOOP('',(#17347));
#3968=EDGE_LOOP('',(#17348));
#3969=EDGE_LOOP('',(#17349));
#3970=EDGE_LOOP('',(#17350));
#3971=EDGE_LOOP('',(#17351));
#3972=EDGE_LOOP('',(#17352));
#3973=EDGE_LOOP('',(#17353));
#3974=EDGE_LOOP('',(#17354));
#3975=EDGE_LOOP('',(#17355));
#3976=EDGE_LOOP('',(#17356));
#3977=EDGE_LOOP('',(#17357));
#3978=EDGE_LOOP('',(#17358));
#3979=EDGE_LOOP('',(#17359));
#3980=EDGE_LOOP('',(#17360));
#3981=EDGE_LOOP('',(#17361,#17362,#17363,#17364));
#3982=EDGE_LOOP('',(#17365,#17366,#17367,#17368));
#3983=EDGE_LOOP('',(#17369));
#3984=EDGE_LOOP('',(#17370,#17371,#17372,#17373));
#3985=EDGE_LOOP('',(#17374,#17375,#17376));
#3986=EDGE_LOOP('',(#17377,#17378,#17379,#17380));
#3987=EDGE_LOOP('',(#17381,#17382,#17383,#17384));
#3988=EDGE_LOOP('',(#17385,#17386,#17387,#17388));
#3989=EDGE_LOOP('',(#17389,#17390,#17391,#17392));
#3990=EDGE_LOOP('',(#17393,#17394,#17395,#17396));
#3991=EDGE_LOOP('',(#17397,#17398,#17399));
#3992=EDGE_LOOP('',(#17400,#17401,#17402,#17403));
#3993=EDGE_LOOP('',(#17404,#17405,#17406,#17407));
#3994=EDGE_LOOP('',(#17408,#17409,#17410,#17411));
#3995=EDGE_LOOP('',(#17412,#17413,#17414,#17415));
#3996=EDGE_LOOP('',(#17416,#17417,#17418,#17419));
#3997=EDGE_LOOP('',(#17420,#17421,#17422));
#3998=EDGE_LOOP('',(#17423,#17424,#17425,#17426));
#3999=EDGE_LOOP('',(#17427,#17428,#17429,#17430));
#4000=EDGE_LOOP('',(#17431,#17432,#17433));
#4001=EDGE_LOOP('',(#17434,#17435,#17436,#17437));
#4002=EDGE_LOOP('',(#17438,#17439,#17440,#17441));
#4003=EDGE_LOOP('',(#17442,#17443,#17444,#17445));
#4004=EDGE_LOOP('',(#17446,#17447,#17448));
#4005=EDGE_LOOP('',(#17449,#17450,#17451,#17452));
#4006=EDGE_LOOP('',(#17453,#17454,#17455,#17456));
#4007=EDGE_LOOP('',(#17457,#17458,#17459,#17460));
#4008=EDGE_LOOP('',(#17461,#17462,#17463,#17464));
#4009=EDGE_LOOP('',(#17465,#17466,#17467,#17468));
#4010=EDGE_LOOP('',(#17469,#17470,#17471,#17472));
#4011=EDGE_LOOP('',(#17473,#17474,#17475,#17476));
#4012=EDGE_LOOP('',(#17477,#17478,#17479));
#4013=EDGE_LOOP('',(#17480,#17481,#17482,#17483));
#4014=EDGE_LOOP('',(#17484,#17485,#17486,#17487));
#4015=EDGE_LOOP('',(#17488,#17489,#17490,#17491));
#4016=EDGE_LOOP('',(#17492,#17493,#17494,#17495));
#4017=EDGE_LOOP('',(#17496,#17497,#17498,#17499));
#4018=EDGE_LOOP('',(#17500,#17501,#17502));
#4019=EDGE_LOOP('',(#17503,#17504,#17505,#17506));
#4020=EDGE_LOOP('',(#17507,#17508,#17509,#17510));
#4021=EDGE_LOOP('',(#17511,#17512,#17513));
#4022=EDGE_LOOP('',(#17514,#17515,#17516,#17517));
#4023=EDGE_LOOP('',(#17518,#17519,#17520,#17521));
#4024=EDGE_LOOP('',(#17522,#17523,#17524,#17525));
#4025=EDGE_LOOP('',(#17526,#17527,#17528));
#4026=EDGE_LOOP('',(#17529,#17530,#17531,#17532));
#4027=EDGE_LOOP('',(#17533,#17534,#17535,#17536));
#4028=EDGE_LOOP('',(#17537,#17538,#17539,#17540));
#4029=EDGE_LOOP('',(#17541,#17542,#17543,#17544));
#4030=EDGE_LOOP('',(#17545,#17546,#17547,#17548));
#4031=EDGE_LOOP('',(#17549,#17550,#17551,#17552));
#4032=EDGE_LOOP('',(#17553,#17554,#17555,#17556));
#4033=EDGE_LOOP('',(#17557,#17558,#17559));
#4034=EDGE_LOOP('',(#17560,#17561,#17562,#17563));
#4035=EDGE_LOOP('',(#17564,#17565,#17566,#17567));
#4036=EDGE_LOOP('',(#17568,#17569,#17570,#17571));
#4037=EDGE_LOOP('',(#17572,#17573,#17574,#17575));
#4038=EDGE_LOOP('',(#17576,#17577,#17578,#17579));
#4039=EDGE_LOOP('',(#17580,#17581,#17582));
#4040=EDGE_LOOP('',(#17583,#17584,#17585,#17586));
#4041=EDGE_LOOP('',(#17587,#17588,#17589,#17590));
#4042=EDGE_LOOP('',(#17591,#17592,#17593));
#4043=EDGE_LOOP('',(#17594,#17595,#17596,#17597));
#4044=EDGE_LOOP('',(#17598,#17599,#17600,#17601));
#4045=EDGE_LOOP('',(#17602,#17603,#17604,#17605));
#4046=EDGE_LOOP('',(#17606,#17607,#17608));
#4047=EDGE_LOOP('',(#17609,#17610,#17611,#17612));
#4048=EDGE_LOOP('',(#17613,#17614,#17615,#17616));
#4049=EDGE_LOOP('',(#17617,#17618,#17619,#17620));
#4050=EDGE_LOOP('',(#17621,#17622,#17623,#17624));
#4051=EDGE_LOOP('',(#17625,#17626,#17627,#17628));
#4052=EDGE_LOOP('',(#17629,#17630,#17631,#17632));
#4053=EDGE_LOOP('',(#17633,#17634,#17635,#17636));
#4054=EDGE_LOOP('',(#17637,#17638,#17639));
#4055=EDGE_LOOP('',(#17640,#17641,#17642,#17643));
#4056=EDGE_LOOP('',(#17644,#17645,#17646,#17647));
#4057=EDGE_LOOP('',(#17648,#17649,#17650,#17651));
#4058=EDGE_LOOP('',(#17652,#17653,#17654,#17655));
#4059=EDGE_LOOP('',(#17656,#17657,#17658,#17659));
#4060=EDGE_LOOP('',(#17660,#17661,#17662));
#4061=EDGE_LOOP('',(#17663,#17664,#17665,#17666));
#4062=EDGE_LOOP('',(#17667,#17668,#17669,#17670));
#4063=EDGE_LOOP('',(#17671,#17672,#17673));
#4064=EDGE_LOOP('',(#17674,#17675,#17676,#17677));
#4065=EDGE_LOOP('',(#17678,#17679,#17680,#17681));
#4066=EDGE_LOOP('',(#17682,#17683,#17684,#17685));
#4067=EDGE_LOOP('',(#17686,#17687,#17688));
#4068=EDGE_LOOP('',(#17689,#17690,#17691,#17692));
#4069=EDGE_LOOP('',(#17693,#17694,#17695,#17696));
#4070=EDGE_LOOP('',(#17697,#17698,#17699,#17700));
#4071=EDGE_LOOP('',(#17701,#17702,#17703,#17704));
#4072=EDGE_LOOP('',(#17705,#17706,#17707));
#4073=EDGE_LOOP('',(#17708,#17709,#17710,#17711));
#4074=EDGE_LOOP('',(#17712,#17713,#17714));
#4075=EDGE_LOOP('',(#17715,#17716,#17717,#17718));
#4076=EDGE_LOOP('',(#17719,#17720,#17721,#17722));
#4077=EDGE_LOOP('',(#17723,#17724,#17725,#17726));
#4078=EDGE_LOOP('',(#17727,#17728,#17729,#17730));
#4079=EDGE_LOOP('',(#17731,#17732,#17733,#17734));
#4080=EDGE_LOOP('',(#17735,#17736,#17737));
#4081=EDGE_LOOP('',(#17738,#17739,#17740,#17741));
#4082=EDGE_LOOP('',(#17742,#17743,#17744,#17745));
#4083=EDGE_LOOP('',(#17746,#17747,#17748,#17749));
#4084=EDGE_LOOP('',(#17750,#17751,#17752,#17753));
#4085=EDGE_LOOP('',(#17754,#17755,#17756,#17757));
#4086=EDGE_LOOP('',(#17758,#17759,#17760));
#4087=EDGE_LOOP('',(#17761,#17762,#17763,#17764));
#4088=EDGE_LOOP('',(#17765,#17766,#17767,#17768));
#4089=EDGE_LOOP('',(#17769,#17770,#17771,#17772));
#4090=EDGE_LOOP('',(#17773,#17774,#17775,#17776));
#4091=EDGE_LOOP('',(#17777,#17778,#17779,#17780));
#4092=EDGE_LOOP('',(#17781,#17782,#17783));
#4093=EDGE_LOOP('',(#17784,#17785,#17786,#17787));
#4094=EDGE_LOOP('',(#17788,#17789,#17790,#17791));
#4095=EDGE_LOOP('',(#17792,#17793,#17794));
#4096=EDGE_LOOP('',(#17795,#17796,#17797,#17798));
#4097=EDGE_LOOP('',(#17799,#17800,#17801,#17802));
#4098=EDGE_LOOP('',(#17803,#17804,#17805,#17806));
#4099=EDGE_LOOP('',(#17807,#17808,#17809));
#4100=EDGE_LOOP('',(#17810,#17811,#17812,#17813));
#4101=EDGE_LOOP('',(#17814,#17815,#17816,#17817));
#4102=EDGE_LOOP('',(#17818,#17819,#17820,#17821));
#4103=EDGE_LOOP('',(#17822,#17823,#17824,#17825));
#4104=EDGE_LOOP('',(#17826,#17827,#17828,#17829,#17830,#17831,#17832,#17833));
#4105=EDGE_LOOP('',(#17834,#17835,#17836,#17837,#17838,#17839,#17840,#17841));
#4106=EDGE_LOOP('',(#17842,#17843,#17844,#17845,#17846,#17847,#17848,#17849));
#4107=EDGE_LOOP('',(#17850,#17851,#17852,#17853,#17854,#17855,#17856,#17857));
#4108=EDGE_LOOP('',(#17858,#17859,#17860,#17861,#17862,#17863,#17864,#17865));
#4109=EDGE_LOOP('',(#17866,#17867,#17868,#17869,#17870,#17871,#17872,#17873));
#4110=EDGE_LOOP('',(#17874));
#4111=EDGE_LOOP('',(#17875,#17876,#17877,#17878));
#4112=EDGE_LOOP('',(#17879));
#4113=EDGE_LOOP('',(#17880,#17881,#17882,#17883));
#4114=EDGE_LOOP('',(#17884,#17885,#17886,#17887,#17888,#17889,#17890,#17891,
#17892,#17893,#17894,#17895,#17896,#17897,#17898,#17899,#17900,#17901,#17902,
#17903,#17904,#17905,#17906,#17907,#17908,#17909,#17910,#17911,#17912,#17913,
#17914,#17915,#17916,#17917,#17918,#17919));
#4115=EDGE_LOOP('',(#17920));
#4116=EDGE_LOOP('',(#17921));
#4117=EDGE_LOOP('',(#17922));
#4118=EDGE_LOOP('',(#17923));
#4119=EDGE_LOOP('',(#17924,#17925,#17926,#17927));
#4120=EDGE_LOOP('',(#17928,#17929,#17930,#17931));
#4121=EDGE_LOOP('',(#17932,#17933,#17934,#17935));
#4122=EDGE_LOOP('',(#17936,#17937,#17938,#17939));
#4123=EDGE_LOOP('',(#17940,#17941,#17942,#17943));
#4124=EDGE_LOOP('',(#17944,#17945,#17946,#17947));
#4125=EDGE_LOOP('',(#17948,#17949,#17950,#17951));
#4126=EDGE_LOOP('',(#17952));
#4127=EDGE_LOOP('',(#17953,#17954,#17955,#17956));
#4128=EDGE_LOOP('',(#17957));
#4129=EDGE_LOOP('',(#17958,#17959,#17960,#17961));
#4130=EDGE_LOOP('',(#17962,#17963,#17964,#17965,#17966,#17967,#17968,#17969,
#17970,#17971,#17972,#17973,#17974,#17975,#17976,#17977,#17978,#17979,#17980,
#17981,#17982,#17983,#17984,#17985,#17986,#17987,#17988,#17989,#17990,#17991,
#17992,#17993,#17994,#17995,#17996,#17997));
#4131=EDGE_LOOP('',(#17998));
#4132=EDGE_LOOP('',(#17999));
#4133=EDGE_LOOP('',(#18000));
#4134=EDGE_LOOP('',(#18001));
#4135=EDGE_LOOP('',(#18002));
#4136=EDGE_LOOP('',(#18003,#18004,#18005,#18006,#18007,#18008));
#4137=EDGE_LOOP('',(#18009));
#4138=EDGE_LOOP('',(#18010,#18011,#18012,#18013));
#4139=EDGE_LOOP('',(#18014,#18015,#18016,#18017,#18018,#18019));
#4140=EDGE_LOOP('',(#18020,#18021,#18022,#18023));
#4141=EDGE_LOOP('',(#18024,#18025,#18026,#18027));
#4142=EDGE_LOOP('',(#18028,#18029,#18030,#18031));
#4143=EDGE_LOOP('',(#18032,#18033,#18034,#18035));
#4144=EDGE_LOOP('',(#18036,#18037,#18038,#18039));
#4145=EDGE_LOOP('',(#18040,#18041,#18042,#18043));
#4146=EDGE_LOOP('',(#18044,#18045,#18046,#18047));
#4147=EDGE_LOOP('',(#18048));
#4148=EDGE_LOOP('',(#18049,#18050,#18051,#18052));
#4149=EDGE_LOOP('',(#18053,#18054,#18055,#18056));
#4150=EDGE_LOOP('',(#18057,#18058,#18059,#18060));
#4151=EDGE_LOOP('',(#18061,#18062,#18063,#18064));
#4152=EDGE_LOOP('',(#18065,#18066,#18067,#18068));
#4153=EDGE_LOOP('',(#18069,#18070,#18071,#18072));
#4154=EDGE_LOOP('',(#18073,#18074,#18075,#18076));
#4155=EDGE_LOOP('',(#18077,#18078,#18079,#18080));
#4156=EDGE_LOOP('',(#18081,#18082,#18083,#18084));
#4157=EDGE_LOOP('',(#18085,#18086,#18087,#18088));
#4158=EDGE_LOOP('',(#18089,#18090,#18091,#18092));
#4159=EDGE_LOOP('',(#18093,#18094,#18095,#18096,#18097,#18098,#18099,#18100,
#18101,#18102,#18103,#18104,#18105));
#4160=EDGE_LOOP('',(#18106,#18107,#18108,#18109));
#4161=EDGE_LOOP('',(#18110,#18111,#18112,#18113));
#4162=EDGE_LOOP('',(#18114,#18115,#18116,#18117));
#4163=EDGE_LOOP('',(#18118,#18119,#18120,#18121));
#4164=EDGE_LOOP('',(#18122,#18123,#18124,#18125));
#4165=EDGE_LOOP('',(#18126,#18127,#18128,#18129));
#4166=EDGE_LOOP('',(#18130));
#4167=EDGE_LOOP('',(#18131,#18132,#18133,#18134));
#4168=EDGE_LOOP('',(#18135,#18136,#18137,#18138));
#4169=EDGE_LOOP('',(#18139,#18140,#18141,#18142,#18143,#18144));
#4170=EDGE_LOOP('',(#18145,#18146,#18147,#18148,#18149,#18150,#18151,#18152,
#18153,#18154,#18155,#18156,#18157,#18158,#18159,#18160,#18161,#18162,#18163,
#18164,#18165));
#4171=EDGE_LOOP('',(#18166,#18167,#18168,#18169,#18170,#18171,#18172,#18173,
#18174));
#4172=EDGE_LOOP('',(#18175,#18176,#18177,#18178,#18179,#18180,#18181,#18182));
#4173=EDGE_LOOP('',(#18183,#18184,#18185,#18186,#18187,#18188));
#4174=EDGE_LOOP('',(#18189,#18190,#18191,#18192,#18193,#18194,#18195,#18196,
#18197,#18198,#18199));
#4175=EDGE_LOOP('',(#18200,#18201,#18202,#18203,#18204,#18205));
#4176=EDGE_LOOP('',(#18206,#18207,#18208,#18209,#18210,#18211,#18212,#18213));
#4177=EDGE_LOOP('',(#18214,#18215,#18216,#18217));
#4178=EDGE_LOOP('',(#18218,#18219,#18220,#18221));
#4179=EDGE_LOOP('',(#18222,#18223,#18224,#18225));
#4180=EDGE_LOOP('',(#18226,#18227,#18228,#18229));
#4181=EDGE_LOOP('',(#18230,#18231,#18232,#18233));
#4182=EDGE_LOOP('',(#18234,#18235,#18236,#18237));
#4183=EDGE_LOOP('',(#18238,#18239,#18240,#18241));
#4184=EDGE_LOOP('',(#18242,#18243,#18244,#18245));
#4185=EDGE_LOOP('',(#18246,#18247,#18248,#18249));
#4186=EDGE_LOOP('',(#18250,#18251,#18252,#18253));
#4187=EDGE_LOOP('',(#18254,#18255,#18256,#18257));
#4188=EDGE_LOOP('',(#18258,#18259,#18260,#18261));
#4189=EDGE_LOOP('',(#18262,#18263,#18264,#18265));
#4190=EDGE_LOOP('',(#18266,#18267,#18268,#18269));
#4191=EDGE_LOOP('',(#18270,#18271,#18272,#18273));
#4192=EDGE_LOOP('',(#18274,#18275,#18276,#18277));
#4193=EDGE_LOOP('',(#18278,#18279,#18280,#18281));
#4194=EDGE_LOOP('',(#18282,#18283,#18284,#18285));
#4195=EDGE_LOOP('',(#18286,#18287,#18288,#18289));
#4196=EDGE_LOOP('',(#18290,#18291,#18292,#18293,#18294,#18295,#18296,#18297,
#18298,#18299,#18300));
#4197=EDGE_LOOP('',(#18301,#18302,#18303,#18304,#18305,#18306));
#4198=EDGE_LOOP('',(#18307,#18308,#18309,#18310));
#4199=EDGE_LOOP('',(#18311,#18312,#18313,#18314));
#4200=EDGE_LOOP('',(#18315,#18316,#18317,#18318));
#4201=EDGE_LOOP('',(#18319,#18320,#18321,#18322));
#4202=EDGE_LOOP('',(#18323,#18324,#18325,#18326));
#4203=EDGE_LOOP('',(#18327,#18328,#18329,#18330));
#4204=EDGE_LOOP('',(#18331,#18332,#18333,#18334));
#4205=EDGE_LOOP('',(#18335,#18336,#18337,#18338));
#4206=EDGE_LOOP('',(#18339,#18340,#18341,#18342));
#4207=EDGE_LOOP('',(#18343,#18344,#18345,#18346));
#4208=EDGE_LOOP('',(#18347,#18348,#18349,#18350));
#4209=EDGE_LOOP('',(#18351,#18352,#18353,#18354));
#4210=EDGE_LOOP('',(#18355,#18356,#18357,#18358,#18359,#18360));
#4211=EDGE_LOOP('',(#18361,#18362,#18363,#18364));
#4212=EDGE_LOOP('',(#18365,#18366,#18367,#18368));
#4213=EDGE_LOOP('',(#18369,#18370,#18371,#18372));
#4214=EDGE_LOOP('',(#18373,#18374,#18375,#18376));
#4215=EDGE_LOOP('',(#18377,#18378,#18379,#18380));
#4216=EDGE_LOOP('',(#18381,#18382,#18383,#18384));
#4217=EDGE_LOOP('',(#18385,#18386,#18387,#18388));
#4218=EDGE_LOOP('',(#18389,#18390,#18391,#18392));
#4219=EDGE_LOOP('',(#18393,#18394,#18395,#18396));
#4220=EDGE_LOOP('',(#18397,#18398,#18399,#18400));
#4221=EDGE_LOOP('',(#18401,#18402,#18403,#18404));
#4222=EDGE_LOOP('',(#18405,#18406,#18407,#18408));
#4223=EDGE_LOOP('',(#18409,#18410,#18411,#18412));
#4224=EDGE_LOOP('',(#18413,#18414,#18415,#18416,#18417,#18418,#18419,#18420,
#18421));
#4225=EDGE_LOOP('',(#18422,#18423,#18424,#18425));
#4226=EDGE_LOOP('',(#18426));
#4227=EDGE_LOOP('',(#18427,#18428,#18429,#18430,#18431,#18432));
#4228=EDGE_LOOP('',(#18433));
#4229=EDGE_LOOP('',(#18434,#18435,#18436,#18437));
#4230=EDGE_LOOP('',(#18438,#18439,#18440,#18441,#18442,#18443));
#4231=EDGE_LOOP('',(#18444,#18445,#18446,#18447));
#4232=EDGE_LOOP('',(#18448,#18449,#18450,#18451));
#4233=EDGE_LOOP('',(#18452,#18453,#18454,#18455));
#4234=EDGE_LOOP('',(#18456,#18457,#18458,#18459));
#4235=EDGE_LOOP('',(#18460,#18461,#18462,#18463));
#4236=EDGE_LOOP('',(#18464,#18465,#18466,#18467));
#4237=EDGE_LOOP('',(#18468,#18469,#18470,#18471));
#4238=EDGE_LOOP('',(#18472));
#4239=EDGE_LOOP('',(#18473,#18474,#18475,#18476));
#4240=EDGE_LOOP('',(#18477,#18478,#18479,#18480));
#4241=EDGE_LOOP('',(#18481,#18482,#18483,#18484));
#4242=EDGE_LOOP('',(#18485,#18486,#18487,#18488));
#4243=EDGE_LOOP('',(#18489,#18490,#18491,#18492));
#4244=EDGE_LOOP('',(#18493,#18494,#18495,#18496));
#4245=EDGE_LOOP('',(#18497,#18498,#18499,#18500));
#4246=EDGE_LOOP('',(#18501,#18502,#18503,#18504));
#4247=EDGE_LOOP('',(#18505,#18506,#18507,#18508));
#4248=EDGE_LOOP('',(#18509,#18510,#18511,#18512));
#4249=EDGE_LOOP('',(#18513,#18514,#18515,#18516));
#4250=EDGE_LOOP('',(#18517,#18518,#18519,#18520,#18521,#18522,#18523,#18524,
#18525,#18526,#18527,#18528,#18529));
#4251=EDGE_LOOP('',(#18530,#18531,#18532,#18533));
#4252=EDGE_LOOP('',(#18534,#18535,#18536,#18537));
#4253=EDGE_LOOP('',(#18538,#18539,#18540,#18541));
#4254=EDGE_LOOP('',(#18542,#18543,#18544,#18545));
#4255=EDGE_LOOP('',(#18546,#18547,#18548,#18549,#18550,#18551,#18552,#18553));
#4256=EDGE_LOOP('',(#18554,#18555,#18556,#18557));
#4257=EDGE_LOOP('',(#18558,#18559,#18560,#18561));
#4258=EDGE_LOOP('',(#18562,#18563,#18564,#18565));
#4259=EDGE_LOOP('',(#18566,#18567,#18568,#18569,#18570));
#4260=EDGE_LOOP('',(#18571,#18572,#18573,#18574));
#4261=EDGE_LOOP('',(#18575,#18576,#18577,#18578));
#4262=EDGE_LOOP('',(#18579,#18580,#18581,#18582,#18583,#18584,#18585,#18586,
#18587,#18588,#18589,#18590,#18591,#18592));
#4263=EDGE_LOOP('',(#18593,#18594,#18595,#18596,#18597,#18598,#18599,#18600,
#18601,#18602,#18603,#18604,#18605,#18606,#18607,#18608,#18609,#18610,#18611,
#18612,#18613));
#4264=EDGE_LOOP('',(#18614,#18615,#18616,#18617,#18618,#18619,#18620,#18621,
#18622));
#4265=EDGE_LOOP('',(#18623,#18624,#18625,#18626,#18627,#18628,#18629,#18630));
#4266=EDGE_LOOP('',(#18631,#18632,#18633,#18634,#18635,#18636));
#4267=EDGE_LOOP('',(#18637,#18638,#18639,#18640,#18641,#18642,#18643,#18644,
#18645,#18646,#18647));
#4268=EDGE_LOOP('',(#18648,#18649,#18650,#18651,#18652,#18653));
#4269=EDGE_LOOP('',(#18654,#18655,#18656,#18657,#18658,#18659,#18660,#18661));
#4270=EDGE_LOOP('',(#18662,#18663,#18664,#18665));
#4271=EDGE_LOOP('',(#18666,#18667,#18668,#18669));
#4272=EDGE_LOOP('',(#18670,#18671,#18672,#18673));
#4273=EDGE_LOOP('',(#18674,#18675,#18676,#18677));
#4274=EDGE_LOOP('',(#18678,#18679,#18680,#18681));
#4275=EDGE_LOOP('',(#18682,#18683,#18684,#18685));
#4276=EDGE_LOOP('',(#18686,#18687,#18688,#18689));
#4277=EDGE_LOOP('',(#18690,#18691,#18692,#18693));
#4278=EDGE_LOOP('',(#18694,#18695,#18696,#18697));
#4279=EDGE_LOOP('',(#18698,#18699,#18700,#18701));
#4280=EDGE_LOOP('',(#18702,#18703,#18704,#18705));
#4281=EDGE_LOOP('',(#18706,#18707,#18708,#18709));
#4282=EDGE_LOOP('',(#18710,#18711,#18712,#18713));
#4283=EDGE_LOOP('',(#18714,#18715,#18716,#18717));
#4284=EDGE_LOOP('',(#18718,#18719,#18720,#18721));
#4285=EDGE_LOOP('',(#18722,#18723,#18724,#18725));
#4286=EDGE_LOOP('',(#18726,#18727,#18728,#18729));
#4287=EDGE_LOOP('',(#18730,#18731,#18732,#18733));
#4288=EDGE_LOOP('',(#18734,#18735,#18736,#18737));
#4289=EDGE_LOOP('',(#18738,#18739,#18740,#18741,#18742,#18743,#18744,#18745,
#18746,#18747,#18748));
#4290=EDGE_LOOP('',(#18749,#18750,#18751,#18752,#18753,#18754));
#4291=EDGE_LOOP('',(#18755,#18756,#18757,#18758));
#4292=EDGE_LOOP('',(#18759,#18760,#18761,#18762));
#4293=EDGE_LOOP('',(#18763,#18764,#18765,#18766));
#4294=EDGE_LOOP('',(#18767,#18768,#18769,#18770));
#4295=EDGE_LOOP('',(#18771,#18772,#18773,#18774));
#4296=EDGE_LOOP('',(#18775,#18776,#18777,#18778));
#4297=EDGE_LOOP('',(#18779,#18780,#18781,#18782));
#4298=EDGE_LOOP('',(#18783,#18784,#18785,#18786));
#4299=EDGE_LOOP('',(#18787,#18788,#18789,#18790));
#4300=EDGE_LOOP('',(#18791,#18792,#18793,#18794));
#4301=EDGE_LOOP('',(#18795,#18796,#18797,#18798));
#4302=EDGE_LOOP('',(#18799,#18800,#18801,#18802));
#4303=EDGE_LOOP('',(#18803,#18804,#18805,#18806,#18807,#18808));
#4304=EDGE_LOOP('',(#18809,#18810,#18811,#18812));
#4305=EDGE_LOOP('',(#18813,#18814,#18815,#18816));
#4306=EDGE_LOOP('',(#18817,#18818,#18819,#18820));
#4307=EDGE_LOOP('',(#18821,#18822,#18823,#18824));
#4308=EDGE_LOOP('',(#18825,#18826,#18827,#18828));
#4309=EDGE_LOOP('',(#18829,#18830,#18831,#18832));
#4310=EDGE_LOOP('',(#18833,#18834,#18835,#18836));
#4311=EDGE_LOOP('',(#18837,#18838,#18839,#18840));
#4312=EDGE_LOOP('',(#18841,#18842,#18843,#18844));
#4313=EDGE_LOOP('',(#18845,#18846,#18847,#18848));
#4314=EDGE_LOOP('',(#18849,#18850,#18851,#18852));
#4315=EDGE_LOOP('',(#18853,#18854,#18855,#18856));
#4316=EDGE_LOOP('',(#18857,#18858,#18859,#18860));
#4317=EDGE_LOOP('',(#18861,#18862,#18863,#18864,#18865,#18866,#18867,#18868,
#18869));
#4318=EDGE_LOOP('',(#18870,#18871,#18872,#18873));
#4319=EDGE_LOOP('',(#18874,#18875,#18876,#18877));
#4320=EDGE_LOOP('',(#18878,#18879,#18880,#18881));
#4321=EDGE_LOOP('',(#18882,#18883,#18884,#18885));
#4322=EDGE_LOOP('',(#18886,#18887,#18888,#18889));
#4323=EDGE_LOOP('',(#18890,#18891,#18892,#18893));
#4324=EDGE_LOOP('',(#18894,#18895,#18896,#18897));
#4325=EDGE_LOOP('',(#18898,#18899,#18900,#18901));
#4326=EDGE_LOOP('',(#18902,#18903,#18904,#18905,#18906,#18907));
#4327=EDGE_LOOP('',(#18908));
#4328=EDGE_LOOP('',(#18909));
#4329=EDGE_LOOP('',(#18910));
#4330=EDGE_LOOP('',(#18911));
#4331=EDGE_LOOP('',(#18912));
#4332=EDGE_LOOP('',(#18913));
#4333=EDGE_LOOP('',(#18914));
#4334=EDGE_LOOP('',(#18915,#18916,#18917,#18918));
#4335=EDGE_LOOP('',(#18919,#18920,#18921,#18922,#18923,#18924));
#4336=EDGE_LOOP('',(#18925));
#4337=EDGE_LOOP('',(#18926));
#4338=EDGE_LOOP('',(#18927));
#4339=EDGE_LOOP('',(#18928));
#4340=EDGE_LOOP('',(#18929));
#4341=EDGE_LOOP('',(#18930));
#4342=EDGE_LOOP('',(#18931));
#4343=EDGE_LOOP('',(#18932,#18933,#18934,#18935));
#4344=EDGE_LOOP('',(#18936,#18937,#18938,#18939));
#4345=EDGE_LOOP('',(#18940,#18941,#18942,#18943));
#4346=EDGE_LOOP('',(#18944,#18945,#18946,#18947));
#4347=EDGE_LOOP('',(#18948,#18949,#18950,#18951));
#4348=EDGE_LOOP('',(#18952,#18953,#18954,#18955));
#4349=EDGE_LOOP('',(#18956,#18957,#18958,#18959));
#4350=EDGE_LOOP('',(#18960,#18961,#18962,#18963));
#4351=EDGE_LOOP('',(#18964,#18965,#18966,#18967));
#4352=EDGE_LOOP('',(#18968,#18969,#18970,#18971));
#4353=EDGE_LOOP('',(#18972,#18973,#18974,#18975));
#4354=EDGE_LOOP('',(#18976,#18977,#18978,#18979));
#4355=EDGE_LOOP('',(#18980,#18981,#18982,#18983));
#4356=EDGE_LOOP('',(#18984,#18985,#18986,#18987));
#4357=EDGE_LOOP('',(#18988,#18989,#18990,#18991));
#4358=EDGE_LOOP('',(#18992,#18993,#18994,#18995));
#4359=EDGE_LOOP('',(#18996));
#4360=EDGE_LOOP('',(#18997));
#4361=EDGE_LOOP('',(#18998));
#4362=EDGE_LOOP('',(#18999));
#4363=EDGE_LOOP('',(#19000));
#4364=EDGE_LOOP('',(#19001));
#4365=EDGE_LOOP('',(#19002,#19003,#19004,#19005));
#4366=EDGE_LOOP('',(#19006));
#4367=EDGE_LOOP('',(#19007));
#4368=EDGE_LOOP('',(#19008));
#4369=EDGE_LOOP('',(#19009));
#4370=EDGE_LOOP('',(#19010));
#4371=EDGE_LOOP('',(#19011));
#4372=EDGE_LOOP('',(#19012,#19013,#19014,#19015));
#4373=EDGE_LOOP('',(#19016,#19017,#19018,#19019));
#4374=EDGE_LOOP('',(#19020,#19021,#19022,#19023));
#4375=EDGE_LOOP('',(#19024,#19025,#19026,#19027));
#4376=EDGE_LOOP('',(#19028,#19029,#19030,#19031));
#4377=EDGE_LOOP('',(#19032,#19033,#19034,#19035));
#4378=EDGE_LOOP('',(#19036,#19037,#19038,#19039));
#4379=EDGE_LOOP('',(#19040,#19041,#19042,#19043));
#4380=EDGE_LOOP('',(#19044,#19045,#19046,#19047));
#4381=EDGE_LOOP('',(#19048,#19049,#19050,#19051));
#4382=EDGE_LOOP('',(#19052,#19053,#19054,#19055));
#4383=EDGE_LOOP('',(#19056));
#4384=EDGE_LOOP('',(#19057));
#4385=EDGE_LOOP('',(#19058));
#4386=EDGE_LOOP('',(#19059));
#4387=EDGE_LOOP('',(#19060));
#4388=EDGE_LOOP('',(#19061));
#4389=EDGE_LOOP('',(#19062,#19063,#19064,#19065));
#4390=EDGE_LOOP('',(#19066));
#4391=EDGE_LOOP('',(#19067));
#4392=EDGE_LOOP('',(#19068));
#4393=EDGE_LOOP('',(#19069));
#4394=EDGE_LOOP('',(#19070));
#4395=EDGE_LOOP('',(#19071));
#4396=EDGE_LOOP('',(#19072,#19073,#19074,#19075));
#4397=EDGE_LOOP('',(#19076,#19077,#19078,#19079));
#4398=EDGE_LOOP('',(#19080,#19081,#19082,#19083));
#4399=EDGE_LOOP('',(#19084,#19085,#19086,#19087));
#4400=EDGE_LOOP('',(#19088,#19089,#19090,#19091));
#4401=EDGE_LOOP('',(#19092,#19093,#19094,#19095,#19096));
#4402=EDGE_LOOP('',(#19097,#19098,#19099,#19100,#19101));
#4403=EDGE_LOOP('',(#19102,#19103,#19104,#19105));
#4404=EDGE_LOOP('',(#19106,#19107,#19108,#19109));
#4405=EDGE_LOOP('',(#19110,#19111,#19112,#19113));
#4406=EDGE_LOOP('',(#19114,#19115,#19116,#19117));
#4407=EDGE_LOOP('',(#19118,#19119,#19120,#19121));
#4408=EDGE_LOOP('',(#19122,#19123,#19124,#19125,#19126));
#4409=EDGE_LOOP('',(#19127,#19128,#19129,#19130,#19131));
#4410=EDGE_LOOP('',(#19132,#19133,#19134,#19135));
#4411=EDGE_LOOP('',(#19136,#19137,#19138,#19139));
#4412=EDGE_LOOP('',(#19140,#19141,#19142,#19143));
#4413=EDGE_LOOP('',(#19144,#19145,#19146,#19147));
#4414=EDGE_LOOP('',(#19148,#19149,#19150,#19151));
#4415=EDGE_LOOP('',(#19152,#19153,#19154,#19155));
#4416=EDGE_LOOP('',(#19156,#19157,#19158,#19159));
#4417=EDGE_LOOP('',(#19160,#19161,#19162,#19163));
#4418=EDGE_LOOP('',(#19164,#19165,#19166,#19167));
#4419=EDGE_LOOP('',(#19168,#19169,#19170,#19171));
#4420=EDGE_LOOP('',(#19172,#19173,#19174,#19175));
#4421=EDGE_LOOP('',(#19176,#19177,#19178,#19179));
#4422=EDGE_LOOP('',(#19180,#19181,#19182,#19183));
#4423=EDGE_LOOP('',(#19184,#19185,#19186,#19187));
#4424=EDGE_LOOP('',(#19188,#19189,#19190,#19191));
#4425=EDGE_LOOP('',(#19192,#19193,#19194,#19195));
#4426=EDGE_LOOP('',(#19196,#19197,#19198,#19199));
#4427=EDGE_LOOP('',(#19200,#19201,#19202,#19203));
#4428=EDGE_LOOP('',(#19204,#19205,#19206,#19207));
#4429=EDGE_LOOP('',(#19208,#19209,#19210,#19211));
#4430=EDGE_LOOP('',(#19212,#19213,#19214,#19215));
#4431=EDGE_LOOP('',(#19216,#19217,#19218,#19219));
#4432=EDGE_LOOP('',(#19220,#19221,#19222,#19223));
#4433=EDGE_LOOP('',(#19224,#19225,#19226,#19227));
#4434=EDGE_LOOP('',(#19228,#19229,#19230,#19231));
#4435=EDGE_LOOP('',(#19232,#19233,#19234,#19235));
#4436=EDGE_LOOP('',(#19236,#19237,#19238,#19239));
#4437=EDGE_LOOP('',(#19240,#19241,#19242,#19243));
#4438=EDGE_LOOP('',(#19244,#19245,#19246,#19247));
#4439=EDGE_LOOP('',(#19248,#19249,#19250,#19251));
#4440=EDGE_LOOP('',(#19252,#19253,#19254,#19255));
#4441=EDGE_LOOP('',(#19256,#19257,#19258,#19259));
#4442=EDGE_LOOP('',(#19260,#19261,#19262,#19263));
#4443=EDGE_LOOP('',(#19264,#19265,#19266,#19267));
#4444=EDGE_LOOP('',(#19268,#19269,#19270,#19271));
#4445=EDGE_LOOP('',(#19272,#19273,#19274,#19275));
#4446=EDGE_LOOP('',(#19276,#19277,#19278,#19279));
#4447=EDGE_LOOP('',(#19280,#19281,#19282,#19283));
#4448=EDGE_LOOP('',(#19284,#19285,#19286,#19287));
#4449=EDGE_LOOP('',(#19288,#19289,#19290,#19291));
#4450=EDGE_LOOP('',(#19292,#19293,#19294,#19295));
#4451=EDGE_LOOP('',(#19296,#19297,#19298,#19299));
#4452=EDGE_LOOP('',(#19300,#19301,#19302,#19303));
#4453=EDGE_LOOP('',(#19304,#19305,#19306,#19307));
#4454=EDGE_LOOP('',(#19308,#19309,#19310,#19311));
#4455=EDGE_LOOP('',(#19312,#19313,#19314,#19315));
#4456=EDGE_LOOP('',(#19316,#19317,#19318,#19319));
#4457=EDGE_LOOP('',(#19320,#19321,#19322,#19323));
#4458=EDGE_LOOP('',(#19324,#19325,#19326,#19327));
#4459=EDGE_LOOP('',(#19328,#19329,#19330,#19331,#19332,#19333,#19334,#19335));
#4460=EDGE_LOOP('',(#19336));
#4461=EDGE_LOOP('',(#19337));
#4462=EDGE_LOOP('',(#19338));
#4463=EDGE_LOOP('',(#19339));
#4464=EDGE_LOOP('',(#19340));
#4465=EDGE_LOOP('',(#19341));
#4466=EDGE_LOOP('',(#19342));
#4467=EDGE_LOOP('',(#19343));
#4468=EDGE_LOOP('',(#19344));
#4469=EDGE_LOOP('',(#19345));
#4470=EDGE_LOOP('',(#19346));
#4471=EDGE_LOOP('',(#19347));
#4472=EDGE_LOOP('',(#19348));
#4473=EDGE_LOOP('',(#19349));
#4474=EDGE_LOOP('',(#19350));
#4475=EDGE_LOOP('',(#19351));
#4476=EDGE_LOOP('',(#19352));
#4477=EDGE_LOOP('',(#19353));
#4478=EDGE_LOOP('',(#19354));
#4479=EDGE_LOOP('',(#19355));
#4480=EDGE_LOOP('',(#19356));
#4481=EDGE_LOOP('',(#19357));
#4482=EDGE_LOOP('',(#19358,#19359,#19360,#19361));
#4483=EDGE_LOOP('',(#19362,#19363,#19364,#19365));
#4484=EDGE_LOOP('',(#19366,#19367,#19368,#19369));
#4485=EDGE_LOOP('',(#19370,#19371,#19372,#19373,#19374,#19375));
#4486=EDGE_LOOP('',(#19376));
#4487=EDGE_LOOP('',(#19377));
#4488=EDGE_LOOP('',(#19378));
#4489=EDGE_LOOP('',(#19379));
#4490=EDGE_LOOP('',(#19380,#19381,#19382,#19383));
#4491=EDGE_LOOP('',(#19384));
#4492=EDGE_LOOP('',(#19385));
#4493=EDGE_LOOP('',(#19386));
#4494=EDGE_LOOP('',(#19387));
#4495=EDGE_LOOP('',(#19388));
#4496=EDGE_LOOP('',(#19389,#19390,#19391,#19392,#19393,#19394));
#4497=EDGE_LOOP('',(#19395,#19396,#19397,#19398));
#4498=EDGE_LOOP('',(#19399));
#4499=EDGE_LOOP('',(#19400));
#4500=EDGE_LOOP('',(#19401));
#4501=EDGE_LOOP('',(#19402));
#4502=EDGE_LOOP('',(#19403));
#4503=EDGE_LOOP('',(#19404));
#4504=EDGE_LOOP('',(#19405));
#4505=EDGE_LOOP('',(#19406));
#4506=EDGE_LOOP('',(#19407));
#4507=EDGE_LOOP('',(#19408,#19409,#19410,#19411,#19412,#19413,#19414,#19415));
#4508=EDGE_LOOP('',(#19416,#19417,#19418,#19419));
#4509=EDGE_LOOP('',(#19420));
#4510=EDGE_LOOP('',(#19421));
#4511=EDGE_LOOP('',(#19422));
#4512=EDGE_LOOP('',(#19423));
#4513=EDGE_LOOP('',(#19424));
#4514=EDGE_LOOP('',(#19425));
#4515=EDGE_LOOP('',(#19426));
#4516=EDGE_LOOP('',(#19427));
#4517=EDGE_LOOP('',(#19428));
#4518=EDGE_LOOP('',(#19429));
#4519=EDGE_LOOP('',(#19430));
#4520=EDGE_LOOP('',(#19431));
#4521=EDGE_LOOP('',(#19432));
#4522=EDGE_LOOP('',(#19433));
#4523=EDGE_LOOP('',(#19434));
#4524=EDGE_LOOP('',(#19435));
#4525=EDGE_LOOP('',(#19436));
#4526=EDGE_LOOP('',(#19437));
#4527=EDGE_LOOP('',(#19438));
#4528=EDGE_LOOP('',(#19439));
#4529=EDGE_LOOP('',(#19440));
#4530=EDGE_LOOP('',(#19441));
#4531=EDGE_LOOP('',(#19442,#19443,#19444,#19445));
#4532=EDGE_LOOP('',(#19446,#19447,#19448,#19449));
#4533=EDGE_LOOP('',(#19450,#19451,#19452,#19453));
#4534=EDGE_LOOP('',(#19454,#19455,#19456,#19457));
#4535=EDGE_LOOP('',(#19458));
#4536=EDGE_LOOP('',(#19459));
#4537=EDGE_LOOP('',(#19460));
#4538=EDGE_LOOP('',(#19461));
#4539=EDGE_LOOP('',(#19462));
#4540=EDGE_LOOP('',(#19463));
#4541=EDGE_LOOP('',(#19464));
#4542=EDGE_LOOP('',(#19465));
#4543=EDGE_LOOP('',(#19466));
#4544=EDGE_LOOP('',(#19467));
#4545=EDGE_LOOP('',(#19468));
#4546=EDGE_LOOP('',(#19469));
#4547=EDGE_LOOP('',(#19470));
#4548=EDGE_LOOP('',(#19471));
#4549=EDGE_LOOP('',(#19472));
#4550=EDGE_LOOP('',(#19473));
#4551=EDGE_LOOP('',(#19474));
#4552=EDGE_LOOP('',(#19475));
#4553=EDGE_LOOP('',(#19476));
#4554=EDGE_LOOP('',(#19477));
#4555=EDGE_LOOP('',(#19478));
#4556=EDGE_LOOP('',(#19479));
#4557=EDGE_LOOP('',(#19480));
#4558=EDGE_LOOP('',(#19481));
#4559=EDGE_LOOP('',(#19482));
#4560=EDGE_LOOP('',(#19483));
#4561=EDGE_LOOP('',(#19484));
#4562=EDGE_LOOP('',(#19485));
#4563=EDGE_LOOP('',(#19486));
#4564=EDGE_LOOP('',(#19487));
#4565=EDGE_LOOP('',(#19488));
#4566=EDGE_LOOP('',(#19489));
#4567=EDGE_LOOP('',(#19490));
#4568=EDGE_LOOP('',(#19491));
#4569=EDGE_LOOP('',(#19492,#19493,#19494,#19495));
#4570=EDGE_LOOP('',(#19496,#19497,#19498,#19499));
#4571=EDGE_LOOP('',(#19500,#19501,#19502,#19503));
#4572=EDGE_LOOP('',(#19504,#19505,#19506,#19507));
#4573=EDGE_LOOP('',(#19508,#19509,#19510,#19511));
#4574=EDGE_LOOP('',(#19512,#19513,#19514,#19515));
#4575=EDGE_LOOP('',(#19516,#19517,#19518,#19519));
#4576=EDGE_LOOP('',(#19520,#19521,#19522,#19523));
#4577=EDGE_LOOP('',(#19524,#19525,#19526,#19527));
#4578=EDGE_LOOP('',(#19528,#19529,#19530,#19531));
#4579=EDGE_LOOP('',(#19532,#19533,#19534,#19535,#19536,#19537,#19538,#19539,
#19540,#19541,#19542,#19543));
#4580=EDGE_LOOP('',(#19544,#19545,#19546,#19547));
#4581=EDGE_LOOP('',(#19548,#19549,#19550,#19551,#19552,#19553,#19554,#19555,
#19556,#19557,#19558,#19559));
#4582=EDGE_LOOP('',(#19560,#19561,#19562,#19563));
#4583=EDGE_LOOP('',(#19564,#19565,#19566,#19567,#19568,#19569,#19570,#19571,
#19572,#19573,#19574,#19575));
#4584=EDGE_LOOP('',(#19576,#19577,#19578,#19579));
#4585=EDGE_LOOP('',(#19580,#19581,#19582,#19583,#19584,#19585,#19586,#19587,
#19588,#19589,#19590,#19591));
#4586=EDGE_LOOP('',(#19592,#19593,#19594,#19595));
#4587=EDGE_LOOP('',(#19596,#19597,#19598,#19599,#19600,#19601,#19602,#19603,
#19604,#19605,#19606,#19607));
#4588=EDGE_LOOP('',(#19608,#19609,#19610,#19611));
#4589=EDGE_LOOP('',(#19612,#19613,#19614,#19615,#19616,#19617,#19618,#19619,
#19620,#19621,#19622,#19623));
#4590=EDGE_LOOP('',(#19624,#19625,#19626,#19627));
#4591=EDGE_LOOP('',(#19628,#19629,#19630,#19631,#19632,#19633,#19634,#19635,
#19636,#19637,#19638,#19639));
#4592=EDGE_LOOP('',(#19640,#19641,#19642,#19643));
#4593=EDGE_LOOP('',(#19644,#19645,#19646,#19647,#19648,#19649,#19650,#19651,
#19652,#19653,#19654,#19655));
#4594=EDGE_LOOP('',(#19656,#19657,#19658,#19659));
#4595=EDGE_LOOP('',(#19660,#19661,#19662,#19663,#19664));
#4596=EDGE_LOOP('',(#19665,#19666,#19667,#19668));
#4597=EDGE_LOOP('',(#19669,#19670,#19671,#19672,#19673,#19674,#19675,#19676,
#19677,#19678,#19679,#19680,#19681,#19682,#19683,#19684,#19685,#19686,#19687,
#19688));
#4598=EDGE_LOOP('',(#19689,#19690,#19691,#19692,#19693,#19694,#19695,#19696,
#19697,#19698,#19699,#19700,#19701,#19702,#19703,#19704,#19705,#19706,#19707,
#19708));
#4599=EDGE_LOOP('',(#19709,#19710,#19711,#19712));
#4600=EDGE_LOOP('',(#19713,#19714,#19715,#19716,#19717));
#4601=EDGE_LOOP('',(#19718,#19719,#19720,#19721));
#4602=EDGE_LOOP('',(#19722,#19723,#19724,#19725));
#4603=EDGE_LOOP('',(#19726,#19727,#19728,#19729,#19730));
#4604=EDGE_LOOP('',(#19731,#19732,#19733,#19734));
#4605=EDGE_LOOP('',(#19735,#19736,#19737,#19738));
#4606=EDGE_LOOP('',(#19739,#19740,#19741,#19742));
#4607=EDGE_LOOP('',(#19743,#19744,#19745,#19746,#19747));
#4608=EDGE_LOOP('',(#19748,#19749,#19750,#19751));
#4609=EDGE_LOOP('',(#19752,#19753,#19754,#19755,#19756));
#4610=EDGE_LOOP('',(#19757,#19758,#19759,#19760));
#4611=EDGE_LOOP('',(#19761,#19762,#19763,#19764));
#4612=EDGE_LOOP('',(#19765,#19766,#19767,#19768,#19769));
#4613=EDGE_LOOP('',(#19770,#19771,#19772,#19773));
#4614=EDGE_LOOP('',(#19774,#19775,#19776,#19777));
#4615=EDGE_LOOP('',(#19778,#19779,#19780,#19781,#19782));
#4616=EDGE_LOOP('',(#19783,#19784,#19785,#19786));
#4617=EDGE_LOOP('',(#19787,#19788,#19789,#19790));
#4618=EDGE_LOOP('',(#19791,#19792,#19793,#19794));
#4619=EDGE_LOOP('',(#19795,#19796,#19797,#19798));
#4620=EDGE_LOOP('',(#19799,#19800,#19801,#19802,#19803,#19804,#19805,#19806,
#19807,#19808,#19809,#19810,#19811,#19812,#19813,#19814,#19815,#19816,#19817,
#19818,#19819,#19820,#19821,#19822,#19823,#19824,#19825,#19826,#19827,#19828,
#19829,#19830,#19831,#19832,#19833,#19834,#19835,#19836,#19837,#19838,#19839,
#19840,#19841,#19842,#19843,#19844));
#4621=EDGE_LOOP('',(#19845,#19846,#19847,#19848,#19849,#19850,#19851,#19852,
#19853,#19854,#19855,#19856,#19857,#19858,#19859,#19860,#19861,#19862,#19863,
#19864,#19865,#19866,#19867,#19868,#19869,#19870,#19871,#19872,#19873,#19874,
#19875,#19876,#19877,#19878,#19879,#19880,#19881,#19882,#19883,#19884,#19885,
#19886,#19887,#19888,#19889,#19890));
#4622=EDGE_LOOP('',(#19891,#19892,#19893,#19894));
#4623=EDGE_LOOP('',(#19895,#19896,#19897,#19898));
#4624=EDGE_LOOP('',(#19899,#19900,#19901,#19902));
#4625=EDGE_LOOP('',(#19903,#19904,#19905,#19906));
#4626=EDGE_LOOP('',(#19907,#19908,#19909,#19910));
#4627=EDGE_LOOP('',(#19911,#19912,#19913,#19914));
#4628=EDGE_LOOP('',(#19915,#19916,#19917,#19918));
#4629=EDGE_LOOP('',(#19919));
#4630=EDGE_LOOP('',(#19920));
#4631=EDGE_LOOP('',(#19921));
#4632=EDGE_LOOP('',(#19922));
#4633=EDGE_LOOP('',(#19923));
#4634=EDGE_LOOP('',(#19924));
#4635=EDGE_LOOP('',(#19925));
#4636=EDGE_LOOP('',(#19926));
#4637=EDGE_LOOP('',(#19927,#19928,#19929,#19930));
#4638=EDGE_LOOP('',(#19931,#19932,#19933,#19934));
#4639=EDGE_LOOP('',(#19935,#19936,#19937,#19938));
#4640=EDGE_LOOP('',(#19939,#19940,#19941,#19942));
#4641=EDGE_LOOP('',(#19943,#19944,#19945,#19946));
#4642=EDGE_LOOP('',(#19947,#19948,#19949,#19950));
#4643=EDGE_LOOP('',(#19951,#19952,#19953,#19954));
#4644=EDGE_LOOP('',(#19955,#19956,#19957,#19958));
#4645=EDGE_LOOP('',(#19959,#19960,#19961,#19962));
#4646=EDGE_LOOP('',(#19963,#19964,#19965,#19966));
#4647=EDGE_LOOP('',(#19967,#19968,#19969,#19970));
#4648=EDGE_LOOP('',(#19971,#19972,#19973,#19974));
#4649=EDGE_LOOP('',(#19975,#19976,#19977,#19978));
#4650=EDGE_LOOP('',(#19979,#19980,#19981,#19982));
#4651=EDGE_LOOP('',(#19983,#19984,#19985,#19986));
#4652=EDGE_LOOP('',(#19987,#19988,#19989,#19990));
#4653=EDGE_LOOP('',(#19991,#19992,#19993,#19994));
#4654=EDGE_LOOP('',(#19995,#19996,#19997,#19998));
#4655=EDGE_LOOP('',(#19999,#20000,#20001,#20002));
#4656=EDGE_LOOP('',(#20003,#20004,#20005,#20006));
#4657=EDGE_LOOP('',(#20007,#20008,#20009,#20010));
#4658=EDGE_LOOP('',(#20011,#20012,#20013,#20014));
#4659=EDGE_LOOP('',(#20015,#20016,#20017,#20018));
#4660=EDGE_LOOP('',(#20019,#20020,#20021,#20022));
#4661=EDGE_LOOP('',(#20023,#20024,#20025,#20026));
#4662=EDGE_LOOP('',(#20027,#20028,#20029,#20030));
#4663=EDGE_LOOP('',(#20031,#20032,#20033,#20034));
#4664=EDGE_LOOP('',(#20035,#20036,#20037,#20038));
#4665=EDGE_LOOP('',(#20039,#20040,#20041,#20042));
#4666=EDGE_LOOP('',(#20043,#20044,#20045,#20046));
#4667=EDGE_LOOP('',(#20047,#20048,#20049,#20050));
#4668=EDGE_LOOP('',(#20051,#20052,#20053,#20054));
#4669=EDGE_LOOP('',(#20055,#20056,#20057,#20058));
#4670=EDGE_LOOP('',(#20059,#20060,#20061,#20062));
#4671=EDGE_LOOP('',(#20063,#20064,#20065,#20066));
#4672=EDGE_LOOP('',(#20067,#20068,#20069,#20070,#20071));
#4673=EDGE_LOOP('',(#20072,#20073,#20074,#20075));
#4674=EDGE_LOOP('',(#20076));
#4675=EDGE_LOOP('',(#20077));
#4676=EDGE_LOOP('',(#20078));
#4677=EDGE_LOOP('',(#20079));
#4678=EDGE_LOOP('',(#20080));
#4679=EDGE_LOOP('',(#20081));
#4680=EDGE_LOOP('',(#20082));
#4681=EDGE_LOOP('',(#20083));
#4682=EDGE_LOOP('',(#20084));
#4683=EDGE_LOOP('',(#20085));
#4684=EDGE_LOOP('',(#20086));
#4685=EDGE_LOOP('',(#20087));
#4686=EDGE_LOOP('',(#20088));
#4687=EDGE_LOOP('',(#20089));
#4688=EDGE_LOOP('',(#20090));
#4689=EDGE_LOOP('',(#20091));
#4690=EDGE_LOOP('',(#20092,#20093,#20094,#20095));
#4691=EDGE_LOOP('',(#20096,#20097,#20098,#20099));
#4692=EDGE_LOOP('',(#20100,#20101,#20102,#20103));
#4693=EDGE_LOOP('',(#20104,#20105,#20106));
#4694=EDGE_LOOP('',(#20107,#20108,#20109));
#4695=EDGE_LOOP('',(#20110,#20111,#20112,#20113));
#4696=EDGE_LOOP('',(#20114,#20115,#20116,#20117));
#4697=EDGE_LOOP('',(#20118,#20119,#20120,#20121));
#4698=EDGE_LOOP('',(#20122,#20123,#20124,#20125));
#4699=EDGE_LOOP('',(#20126,#20127,#20128,#20129));
#4700=EDGE_LOOP('',(#20130,#20131,#20132,#20133));
#4701=EDGE_LOOP('',(#20134,#20135,#20136,#20137));
#4702=EDGE_LOOP('',(#20138,#20139,#20140,#20141,#20142,#20143,#20144));
#4703=EDGE_LOOP('',(#20145,#20146,#20147));
#4704=EDGE_LOOP('',(#20148,#20149,#20150));
#4705=EDGE_LOOP('',(#20151,#20152,#20153,#20154,#20155,#20156,#20157));
#4706=EDGE_LOOP('',(#20158,#20159,#20160,#20161,#20162,#20163,#20164,#20165,
#20166,#20167));
#4707=EDGE_LOOP('',(#20168,#20169,#20170,#20171,#20172));
#4708=EDGE_LOOP('',(#20173,#20174,#20175,#20176));
#4709=EDGE_LOOP('',(#20177,#20178,#20179,#20180));
#4710=EDGE_LOOP('',(#20181,#20182,#20183,#20184));
#4711=EDGE_LOOP('',(#20185,#20186,#20187,#20188));
#4712=EDGE_LOOP('',(#20189,#20190,#20191,#20192));
#4713=EDGE_LOOP('',(#20193,#20194,#20195,#20196));
#4714=EDGE_LOOP('',(#20197,#20198,#20199,#20200));
#4715=EDGE_LOOP('',(#20201,#20202,#20203,#20204));
#4716=EDGE_LOOP('',(#20205,#20206,#20207,#20208));
#4717=EDGE_LOOP('',(#20209,#20210,#20211,#20212));
#4718=EDGE_LOOP('',(#20213,#20214,#20215,#20216));
#4719=EDGE_LOOP('',(#20217,#20218,#20219,#20220));
#4720=EDGE_LOOP('',(#20221,#20222,#20223,#20224));
#4721=EDGE_LOOP('',(#20225,#20226,#20227,#20228));
#4722=EDGE_LOOP('',(#20229,#20230,#20231,#20232));
#4723=EDGE_LOOP('',(#20233,#20234,#20235,#20236));
#4724=EDGE_LOOP('',(#20237,#20238,#20239,#20240));
#4725=EDGE_LOOP('',(#20241,#20242,#20243,#20244));
#4726=EDGE_LOOP('',(#20245,#20246,#20247,#20248));
#4727=EDGE_LOOP('',(#20249,#20250,#20251,#20252));
#4728=EDGE_LOOP('',(#20253,#20254,#20255,#20256));
#4729=EDGE_LOOP('',(#20257,#20258,#20259,#20260));
#4730=EDGE_LOOP('',(#20261,#20262,#20263,#20264));
#4731=EDGE_LOOP('',(#20265,#20266,#20267,#20268));
#4732=EDGE_LOOP('',(#20269,#20270,#20271,#20272));
#4733=EDGE_LOOP('',(#20273,#20274,#20275,#20276));
#4734=EDGE_LOOP('',(#20277,#20278,#20279,#20280));
#4735=EDGE_LOOP('',(#20281,#20282,#20283,#20284));
#4736=EDGE_LOOP('',(#20285,#20286,#20287,#20288));
#4737=EDGE_LOOP('',(#20289,#20290,#20291,#20292));
#4738=EDGE_LOOP('',(#20293,#20294,#20295,#20296));
#4739=EDGE_LOOP('',(#20297,#20298,#20299,#20300));
#4740=EDGE_LOOP('',(#20301,#20302,#20303,#20304));
#4741=EDGE_LOOP('',(#20305,#20306,#20307,#20308));
#4742=EDGE_LOOP('',(#20309,#20310,#20311,#20312));
#4743=EDGE_LOOP('',(#20313,#20314,#20315,#20316));
#4744=EDGE_LOOP('',(#20317,#20318,#20319,#20320));
#4745=EDGE_LOOP('',(#20321,#20322,#20323,#20324));
#4746=EDGE_LOOP('',(#20325,#20326,#20327,#20328));
#4747=EDGE_LOOP('',(#20329,#20330,#20331,#20332));
#4748=EDGE_LOOP('',(#20333,#20334,#20335,#20336));
#4749=EDGE_LOOP('',(#20337,#20338,#20339,#20340));
#4750=EDGE_LOOP('',(#20341));
#4751=EDGE_LOOP('',(#20342));
#4752=EDGE_LOOP('',(#20343,#20344,#20345,#20346));
#4753=EDGE_LOOP('',(#20347,#20348,#20349,#20350,#20351,#20352,#20353,#20354,
#20355,#20356,#20357,#20358,#20359,#20360,#20361,#20362,#20363,#20364,#20365,
#20366,#20367,#20368,#20369,#20370,#20371,#20372,#20373,#20374,#20375,#20376,
#20377,#20378,#20379,#20380,#20381,#20382,#20383,#20384,#20385,#20386,#20387,
#20388,#20389,#20390));
#4754=EDGE_LOOP('',(#20391));
#4755=EDGE_LOOP('',(#20392,#20393,#20394,#20395));
#4756=EDGE_LOOP('',(#20396,#20397,#20398,#20399));
#4757=EDGE_LOOP('',(#20400,#20401,#20402,#20403));
#4758=EDGE_LOOP('',(#20404,#20405,#20406,#20407));
#4759=EDGE_LOOP('',(#20408,#20409,#20410,#20411));
#4760=EDGE_LOOP('',(#20412,#20413,#20414,#20415));
#4761=EDGE_LOOP('',(#20416,#20417,#20418,#20419));
#4762=EDGE_LOOP('',(#20420,#20421,#20422,#20423));
#4763=EDGE_LOOP('',(#20424,#20425,#20426,#20427));
#4764=EDGE_LOOP('',(#20428,#20429,#20430,#20431));
#4765=EDGE_LOOP('',(#20432,#20433,#20434,#20435));
#4766=EDGE_LOOP('',(#20436,#20437,#20438,#20439));
#4767=EDGE_LOOP('',(#20440,#20441,#20442,#20443,#20444,#20445));
#4768=EDGE_LOOP('',(#20446,#20447,#20448,#20449,#20450,#20451,#20452,#20453,
#20454,#20455,#20456,#20457,#20458,#20459,#20460,#20461,#20462,#20463,#20464,
#20465,#20466,#20467,#20468,#20469,#20470,#20471,#20472,#20473,#20474,#20475,
#20476,#20477,#20478,#20479,#20480,#20481,#20482,#20483,#20484,#20485,#20486,
#20487,#20488,#20489));
#4769=EDGE_LOOP('',(#20490,#20491,#20492,#20493,#20494,#20495,#20496,#20497,
#20498,#20499,#20500,#20501,#20502,#20503,#20504,#20505,#20506,#20507,#20508,
#20509,#20510,#20511,#20512,#20513,#20514,#20515,#20516,#20517,#20518,#20519,
#20520,#20521,#20522,#20523,#20524,#20525,#20526,#20527,#20528,#20529,#20530,
#20531,#20532,#20533));
#4770=EDGE_LOOP('',(#20534,#20535,#20536,#20537));
#4771=EDGE_LOOP('',(#20538,#20539,#20540,#20541));
#4772=EDGE_LOOP('',(#20542,#20543,#20544,#20545));
#4773=EDGE_LOOP('',(#20546,#20547,#20548,#20549));
#4774=EDGE_LOOP('',(#20550,#20551,#20552,#20553));
#4775=EDGE_LOOP('',(#20554,#20555,#20556,#20557));
#4776=EDGE_LOOP('',(#20558,#20559,#20560,#20561));
#4777=EDGE_LOOP('',(#20562,#20563,#20564,#20565));
#4778=EDGE_LOOP('',(#20566,#20567,#20568,#20569));
#4779=EDGE_LOOP('',(#20570,#20571,#20572,#20573));
#4780=EDGE_LOOP('',(#20574,#20575,#20576,#20577));
#4781=EDGE_LOOP('',(#20578,#20579,#20580,#20581));
#4782=EDGE_LOOP('',(#20582,#20583,#20584,#20585));
#4783=EDGE_LOOP('',(#20586,#20587,#20588,#20589));
#4784=EDGE_LOOP('',(#20590,#20591,#20592,#20593));
#4785=EDGE_LOOP('',(#20594,#20595,#20596,#20597));
#4786=EDGE_LOOP('',(#20598,#20599,#20600,#20601));
#4787=EDGE_LOOP('',(#20602,#20603,#20604,#20605));
#4788=EDGE_LOOP('',(#20606,#20607,#20608,#20609));
#4789=EDGE_LOOP('',(#20610,#20611,#20612,#20613));
#4790=EDGE_LOOP('',(#20614,#20615,#20616,#20617));
#4791=EDGE_LOOP('',(#20618,#20619,#20620,#20621));
#4792=EDGE_LOOP('',(#20622,#20623,#20624,#20625));
#4793=EDGE_LOOP('',(#20626,#20627,#20628,#20629));
#4794=EDGE_LOOP('',(#20630,#20631,#20632,#20633));
#4795=EDGE_LOOP('',(#20634,#20635,#20636,#20637));
#4796=EDGE_LOOP('',(#20638,#20639,#20640,#20641));
#4797=EDGE_LOOP('',(#20642,#20643,#20644,#20645));
#4798=EDGE_LOOP('',(#20646,#20647,#20648,#20649));
#4799=EDGE_LOOP('',(#20650,#20651,#20652,#20653));
#4800=EDGE_LOOP('',(#20654,#20655,#20656,#20657));
#4801=EDGE_LOOP('',(#20658,#20659,#20660,#20661));
#4802=EDGE_LOOP('',(#20662,#20663,#20664,#20665));
#4803=EDGE_LOOP('',(#20666,#20667,#20668,#20669));
#4804=EDGE_LOOP('',(#20670,#20671,#20672,#20673));
#4805=EDGE_LOOP('',(#20674,#20675,#20676,#20677));
#4806=EDGE_LOOP('',(#20678,#20679,#20680,#20681));
#4807=EDGE_LOOP('',(#20682,#20683,#20684,#20685));
#4808=EDGE_LOOP('',(#20686,#20687,#20688,#20689));
#4809=EDGE_LOOP('',(#20690,#20691,#20692,#20693));
#4810=EDGE_LOOP('',(#20694,#20695,#20696,#20697));
#4811=EDGE_LOOP('',(#20698,#20699,#20700,#20701));
#4812=EDGE_LOOP('',(#20702,#20703,#20704,#20705));
#4813=EDGE_LOOP('',(#20706,#20707,#20708,#20709));
#4814=EDGE_LOOP('',(#20710));
#4815=EDGE_LOOP('',(#20711,#20712,#20713,#20714));
#4816=EDGE_LOOP('',(#20715,#20716,#20717,#20718,#20719,#20720,#20721,#20722,
#20723,#20724,#20725,#20726,#20727,#20728,#20729,#20730,#20731,#20732,#20733,
#20734,#20735,#20736,#20737,#20738,#20739,#20740,#20741,#20742,#20743,#20744,
#20745,#20746,#20747,#20748,#20749,#20750,#20751,#20752,#20753,#20754,#20755,
#20756,#20757,#20758,#20759,#20760,#20761,#20762));
#4817=EDGE_LOOP('',(#20763,#20764,#20765,#20766));
#4818=EDGE_LOOP('',(#20767,#20768,#20769,#20770));
#4819=EDGE_LOOP('',(#20771,#20772,#20773,#20774));
#4820=EDGE_LOOP('',(#20775));
#4821=EDGE_LOOP('',(#20776,#20777,#20778,#20779));
#4822=EDGE_LOOP('',(#20780,#20781,#20782,#20783));
#4823=EDGE_LOOP('',(#20784,#20785,#20786,#20787));
#4824=EDGE_LOOP('',(#20788,#20789,#20790,#20791));
#4825=EDGE_LOOP('',(#20792,#20793,#20794,#20795));
#4826=EDGE_LOOP('',(#20796,#20797,#20798,#20799,#20800,#20801,#20802,#20803));
#4827=EDGE_LOOP('',(#20804,#20805,#20806,#20807));
#4828=EDGE_LOOP('',(#20808,#20809,#20810,#20811));
#4829=EDGE_LOOP('',(#20812,#20813,#20814,#20815));
#4830=EDGE_LOOP('',(#20816,#20817,#20818,#20819));
#4831=EDGE_LOOP('',(#20820,#20821,#20822,#20823));
#4832=EDGE_LOOP('',(#20824,#20825,#20826,#20827));
#4833=EDGE_LOOP('',(#20828,#20829,#20830,#20831));
#4834=EDGE_LOOP('',(#20832,#20833,#20834,#20835));
#4835=EDGE_LOOP('',(#20836,#20837,#20838,#20839));
#4836=EDGE_LOOP('',(#20840,#20841,#20842,#20843));
#4837=EDGE_LOOP('',(#20844,#20845,#20846,#20847));
#4838=EDGE_LOOP('',(#20848,#20849,#20850,#20851));
#4839=EDGE_LOOP('',(#20852,#20853,#20854,#20855));
#4840=EDGE_LOOP('',(#20856,#20857,#20858,#20859));
#4841=EDGE_LOOP('',(#20860,#20861,#20862,#20863));
#4842=EDGE_LOOP('',(#20864,#20865,#20866,#20867));
#4843=EDGE_LOOP('',(#20868,#20869,#20870,#20871));
#4844=EDGE_LOOP('',(#20872,#20873,#20874,#20875));
#4845=EDGE_LOOP('',(#20876,#20877,#20878,#20879));
#4846=EDGE_LOOP('',(#20880,#20881,#20882,#20883));
#4847=EDGE_LOOP('',(#20884,#20885,#20886,#20887));
#4848=EDGE_LOOP('',(#20888,#20889,#20890,#20891));
#4849=EDGE_LOOP('',(#20892,#20893,#20894,#20895));
#4850=EDGE_LOOP('',(#20896,#20897,#20898,#20899));
#4851=EDGE_LOOP('',(#20900,#20901,#20902,#20903));
#4852=EDGE_LOOP('',(#20904,#20905,#20906,#20907));
#4853=EDGE_LOOP('',(#20908,#20909,#20910,#20911));
#4854=EDGE_LOOP('',(#20912,#20913,#20914,#20915));
#4855=EDGE_LOOP('',(#20916,#20917,#20918,#20919));
#4856=EDGE_LOOP('',(#20920,#20921,#20922,#20923));
#4857=EDGE_LOOP('',(#20924,#20925,#20926,#20927));
#4858=EDGE_LOOP('',(#20928,#20929,#20930,#20931));
#4859=EDGE_LOOP('',(#20932,#20933,#20934,#20935));
#4860=EDGE_LOOP('',(#20936,#20937,#20938,#20939));
#4861=EDGE_LOOP('',(#20940,#20941,#20942,#20943));
#4862=EDGE_LOOP('',(#20944,#20945,#20946,#20947));
#4863=EDGE_LOOP('',(#20948,#20949,#20950,#20951));
#4864=EDGE_LOOP('',(#20952,#20953,#20954,#20955));
#4865=EDGE_LOOP('',(#20956,#20957,#20958,#20959));
#4866=EDGE_LOOP('',(#20960));
#4867=EDGE_LOOP('',(#20961,#20962,#20963,#20964));
#4868=EDGE_LOOP('',(#20965,#20966,#20967,#20968));
#4869=EDGE_LOOP('',(#20969,#20970,#20971,#20972));
#4870=EDGE_LOOP('',(#20973,#20974,#20975,#20976));
#4871=EDGE_LOOP('',(#20977,#20978,#20979,#20980));
#4872=EDGE_LOOP('',(#20981,#20982,#20983,#20984));
#4873=EDGE_LOOP('',(#20985,#20986,#20987,#20988));
#4874=EDGE_LOOP('',(#20989,#20990,#20991,#20992,#20993,#20994));
#4875=EDGE_LOOP('',(#20995,#20996,#20997,#20998));
#4876=EDGE_LOOP('',(#20999,#21000,#21001,#21002));
#4877=EDGE_LOOP('',(#21003,#21004,#21005,#21006,#21007,#21008));
#4878=EDGE_LOOP('',(#21009,#21010,#21011,#21012));
#4879=EDGE_LOOP('',(#21013,#21014,#21015,#21016,#21017,#21018,#21019,#21020,
#21021,#21022,#21023,#21024,#21025,#21026,#21027,#21028,#21029,#21030,#21031,
#21032,#21033,#21034,#21035,#21036,#21037,#21038,#21039,#21040,#21041,#21042,
#21043,#21044,#21045,#21046,#21047,#21048,#21049,#21050,#21051,#21052,#21053,
#21054,#21055,#21056));
#4880=EDGE_LOOP('',(#21057,#21058,#21059,#21060,#21061,#21062,#21063,#21064,
#21065,#21066,#21067,#21068,#21069,#21070,#21071,#21072,#21073,#21074,#21075,
#21076,#21077,#21078,#21079,#21080,#21081,#21082,#21083,#21084,#21085,#21086,
#21087,#21088,#21089,#21090,#21091,#21092,#21093,#21094,#21095,#21096,#21097,
#21098,#21099,#21100));
#4881=EDGE_LOOP('',(#21101,#21102,#21103,#21104));
#4882=EDGE_LOOP('',(#21105,#21106,#21107,#21108));
#4883=EDGE_LOOP('',(#21109,#21110,#21111,#21112,#21113,#21114));
#4884=EDGE_LOOP('',(#21115,#21116,#21117,#21118));
#4885=EDGE_LOOP('',(#21119,#21120,#21121,#21122,#21123,#21124));
#4886=EDGE_LOOP('',(#21125,#21126,#21127,#21128));
#4887=EDGE_LOOP('',(#21129));
#4888=EDGE_LOOP('',(#21130,#21131,#21132,#21133));
#4889=EDGE_LOOP('',(#21134,#21135,#21136,#21137,#21138,#21139,#21140,#21141));
#4890=EDGE_LOOP('',(#21142,#21143,#21144,#21145,#21146,#21147));
#4891=EDGE_LOOP('',(#21148));
#4892=EDGE_LOOP('',(#21149,#21150,#21151,#21152));
#4893=EDGE_LOOP('',(#21153,#21154,#21155,#21156));
#4894=EDGE_LOOP('',(#21157,#21158,#21159,#21160));
#4895=EDGE_LOOP('',(#21161,#21162,#21163,#21164,#21165,#21166));
#4896=EDGE_LOOP('',(#21167));
#4897=EDGE_LOOP('',(#21168,#21169,#21170,#21171));
#4898=EDGE_LOOP('',(#21172,#21173,#21174,#21175,#21176,#21177,#21178,#21179));
#4899=EDGE_LOOP('',(#21180,#21181,#21182,#21183));
#4900=EDGE_LOOP('',(#21184,#21185,#21186,#21187));
#4901=EDGE_LOOP('',(#21188,#21189,#21190,#21191));
#4902=EDGE_LOOP('',(#21192,#21193,#21194,#21195));
#4903=EDGE_LOOP('',(#21196,#21197,#21198,#21199));
#4904=EDGE_LOOP('',(#21200,#21201,#21202,#21203));
#4905=EDGE_LOOP('',(#21204,#21205,#21206,#21207));
#4906=EDGE_LOOP('',(#21208,#21209,#21210,#21211));
#4907=EDGE_LOOP('',(#21212,#21213,#21214,#21215));
#4908=EDGE_LOOP('',(#21216,#21217,#21218,#21219));
#4909=EDGE_LOOP('',(#21220,#21221,#21222,#21223));
#4910=EDGE_LOOP('',(#21224,#21225,#21226,#21227));
#4911=EDGE_LOOP('',(#21228,#21229,#21230,#21231));
#4912=EDGE_LOOP('',(#21232,#21233,#21234,#21235));
#4913=EDGE_LOOP('',(#21236,#21237,#21238,#21239));
#4914=EDGE_LOOP('',(#21240,#21241,#21242,#21243));
#4915=EDGE_LOOP('',(#21244,#21245,#21246,#21247));
#4916=EDGE_LOOP('',(#21248,#21249,#21250,#21251));
#4917=EDGE_LOOP('',(#21252,#21253,#21254,#21255));
#4918=EDGE_LOOP('',(#21256,#21257,#21258,#21259));
#4919=EDGE_LOOP('',(#21260,#21261,#21262,#21263));
#4920=EDGE_LOOP('',(#21264,#21265,#21266,#21267));
#4921=EDGE_LOOP('',(#21268,#21269,#21270,#21271));
#4922=EDGE_LOOP('',(#21272,#21273,#21274,#21275));
#4923=EDGE_LOOP('',(#21276,#21277,#21278,#21279));
#4924=EDGE_LOOP('',(#21280,#21281,#21282,#21283));
#4925=EDGE_LOOP('',(#21284,#21285,#21286,#21287));
#4926=EDGE_LOOP('',(#21288,#21289,#21290,#21291));
#4927=EDGE_LOOP('',(#21292,#21293,#21294,#21295));
#4928=EDGE_LOOP('',(#21296,#21297,#21298,#21299));
#4929=EDGE_LOOP('',(#21300,#21301,#21302,#21303));
#4930=EDGE_LOOP('',(#21304,#21305,#21306,#21307));
#4931=EDGE_LOOP('',(#21308,#21309,#21310,#21311));
#4932=EDGE_LOOP('',(#21312,#21313,#21314,#21315));
#4933=EDGE_LOOP('',(#21316,#21317,#21318,#21319));
#4934=EDGE_LOOP('',(#21320,#21321,#21322,#21323));
#4935=EDGE_LOOP('',(#21324,#21325,#21326,#21327));
#4936=EDGE_LOOP('',(#21328,#21329,#21330,#21331));
#4937=EDGE_LOOP('',(#21332,#21333,#21334,#21335));
#4938=EDGE_LOOP('',(#21336,#21337,#21338,#21339));
#4939=EDGE_LOOP('',(#21340,#21341,#21342,#21343));
#4940=EDGE_LOOP('',(#21344,#21345,#21346,#21347));
#4941=EDGE_LOOP('',(#21348,#21349,#21350,#21351));
#4942=EDGE_LOOP('',(#21352,#21353,#21354,#21355));
#4943=EDGE_LOOP('',(#21356,#21357,#21358,#21359));
#4944=EDGE_LOOP('',(#21360));
#4945=EDGE_LOOP('',(#21361,#21362,#21363,#21364));
#4946=EDGE_LOOP('',(#21365,#21366,#21367,#21368));
#4947=EDGE_LOOP('',(#21369,#21370,#21371,#21372));
#4948=EDGE_LOOP('',(#21373,#21374,#21375,#21376));
#4949=EDGE_LOOP('',(#21377));
#4950=EDGE_LOOP('',(#21378,#21379,#21380,#21381));
#4951=EDGE_LOOP('',(#21382));
#4952=EDGE_LOOP('',(#21383,#21384,#21385,#21386));
#4953=EDGE_LOOP('',(#21387,#21388,#21389,#21390));
#4954=EDGE_LOOP('',(#21391,#21392,#21393,#21394));
#4955=EDGE_LOOP('',(#21395,#21396,#21397,#21398,#21399,#21400));
#4956=EDGE_LOOP('',(#21401,#21402,#21403,#21404));
#4957=EDGE_LOOP('',(#21405,#21406,#21407,#21408));
#4958=EDGE_LOOP('',(#21409));
#4959=EDGE_LOOP('',(#21410));
#4960=EDGE_LOOP('',(#21411,#21412,#21413,#21414));
#4961=EDGE_LOOP('',(#21415,#21416,#21417,#21418));
#4962=EDGE_LOOP('',(#21419,#21420,#21421,#21422));
#4963=EDGE_LOOP('',(#21423,#21424,#21425,#21426));
#4964=EDGE_LOOP('',(#21427,#21428,#21429,#21430));
#4965=EDGE_LOOP('',(#21431,#21432,#21433,#21434));
#4966=EDGE_LOOP('',(#21435,#21436,#21437,#21438));
#4967=EDGE_LOOP('',(#21439,#21440,#21441,#21442));
#4968=EDGE_LOOP('',(#21443));
#4969=EDGE_LOOP('',(#21444));
#4970=EDGE_LOOP('',(#21445,#21446,#21447,#21448));
#4971=EDGE_LOOP('',(#21449,#21450,#21451,#21452));
#4972=EDGE_LOOP('',(#21453,#21454,#21455,#21456));
#4973=EDGE_LOOP('',(#21457,#21458,#21459,#21460,#21461,#21462));
#4974=EDGE_LOOP('',(#21463,#21464,#21465,#21466,#21467,#21468));
#4975=EDGE_LOOP('',(#21469));
#4976=EDGE_LOOP('',(#21470,#21471,#21472,#21473));
#4977=EDGE_LOOP('',(#21474,#21475,#21476,#21477));
#4978=EDGE_LOOP('',(#21478,#21479,#21480,#21481));
#4979=EDGE_LOOP('',(#21482,#21483,#21484,#21485));
#4980=EDGE_LOOP('',(#21486,#21487,#21488,#21489,#21490,#21491));
#4981=EDGE_LOOP('',(#21492));
#4982=EDGE_LOOP('',(#21493,#21494,#21495,#21496));
#4983=EDGE_LOOP('',(#21497,#21498,#21499,#21500));
#4984=EDGE_LOOP('',(#21501,#21502,#21503,#21504));
#4985=EDGE_LOOP('',(#21505,#21506,#21507,#21508,#21509,#21510,#21511,#21512,
#21513,#21514,#21515,#21516,#21517,#21518,#21519,#21520,#21521,#21522,#21523,
#21524,#21525,#21526,#21527,#21528,#21529,#21530,#21531,#21532,#21533,#21534,
#21535,#21536,#21537,#21538,#21539,#21540));
#4986=EDGE_LOOP('',(#21541,#21542,#21543,#21544));
#4987=EDGE_LOOP('',(#21545,#21546,#21547,#21548,#21549,#21550,#21551,#21552,
#21553,#21554,#21555,#21556,#21557,#21558,#21559,#21560,#21561,#21562,#21563,
#21564,#21565,#21566,#21567,#21568,#21569,#21570,#21571,#21572,#21573,#21574,
#21575,#21576,#21577,#21578,#21579,#21580,#21581,#21582,#21583,#21584,#21585,
#21586,#21587,#21588,#21589,#21590,#21591,#21592));
#4988=EDGE_LOOP('',(#21593,#21594,#21595,#21596,#21597,#21598,#21599,#21600,
#21601,#21602,#21603,#21604,#21605,#21606,#21607,#21608,#21609,#21610,#21611,
#21612,#21613,#21614,#21615,#21616,#21617,#21618,#21619,#21620,#21621,#21622,
#21623,#21624,#21625,#21626,#21627,#21628,#21629,#21630,#21631,#21632,#21633,
#21634,#21635,#21636));
#4989=EDGE_LOOP('',(#21637,#21638,#21639,#21640,#21641,#21642,#21643,#21644,
#21645,#21646,#21647,#21648,#21649,#21650,#21651,#21652,#21653,#21654,#21655,
#21656,#21657,#21658,#21659,#21660,#21661,#21662,#21663,#21664,#21665,#21666,
#21667,#21668,#21669,#21670,#21671,#21672));
#4990=EDGE_LOOP('',(#21673,#21674,#21675,#21676));
#4991=EDGE_LOOP('',(#21677,#21678,#21679,#21680));
#4992=EDGE_LOOP('',(#21681,#21682,#21683,#21684));
#4993=EDGE_LOOP('',(#21685));
#4994=EDGE_LOOP('',(#21686,#21687,#21688,#21689));
#4995=EDGE_LOOP('',(#21690,#21691,#21692,#21693));
#4996=EDGE_LOOP('',(#21694,#21695,#21696,#21697));
#4997=EDGE_LOOP('',(#21698,#21699,#21700,#21701));
#4998=EDGE_LOOP('',(#21702,#21703,#21704,#21705));
#4999=EDGE_LOOP('',(#21706,#21707,#21708,#21709));
#5000=EDGE_LOOP('',(#21710,#21711,#21712,#21713,#21714,#21715,#21716,#21717,
#21718,#21719));
#5001=EDGE_LOOP('',(#21720,#21721,#21722,#21723));
#5002=EDGE_LOOP('',(#21724,#21725,#21726,#21727));
#5003=EDGE_LOOP('',(#21728,#21729,#21730,#21731));
#5004=EDGE_LOOP('',(#21732,#21733,#21734,#21735));
#5005=EDGE_LOOP('',(#21736,#21737,#21738,#21739));
#5006=EDGE_LOOP('',(#21740,#21741,#21742,#21743));
#5007=EDGE_LOOP('',(#21744,#21745,#21746,#21747));
#5008=EDGE_LOOP('',(#21748,#21749,#21750,#21751));
#5009=EDGE_LOOP('',(#21752,#21753,#21754,#21755));
#5010=EDGE_LOOP('',(#21756,#21757,#21758,#21759));
#5011=EDGE_LOOP('',(#21760,#21761,#21762,#21763));
#5012=EDGE_LOOP('',(#21764,#21765,#21766,#21767));
#5013=EDGE_LOOP('',(#21768,#21769,#21770,#21771));
#5014=EDGE_LOOP('',(#21772,#21773,#21774,#21775));
#5015=EDGE_LOOP('',(#21776,#21777,#21778,#21779));
#5016=EDGE_LOOP('',(#21780,#21781,#21782,#21783));
#5017=EDGE_LOOP('',(#21784,#21785,#21786,#21787));
#5018=EDGE_LOOP('',(#21788,#21789,#21790,#21791));
#5019=EDGE_LOOP('',(#21792,#21793,#21794,#21795));
#5020=EDGE_LOOP('',(#21796,#21797,#21798,#21799));
#5021=EDGE_LOOP('',(#21800,#21801,#21802,#21803));
#5022=EDGE_LOOP('',(#21804,#21805,#21806,#21807));
#5023=EDGE_LOOP('',(#21808,#21809,#21810,#21811));
#5024=EDGE_LOOP('',(#21812,#21813,#21814,#21815));
#5025=EDGE_LOOP('',(#21816,#21817,#21818,#21819));
#5026=EDGE_LOOP('',(#21820,#21821,#21822,#21823));
#5027=EDGE_LOOP('',(#21824,#21825,#21826,#21827));
#5028=EDGE_LOOP('',(#21828));
#5029=EDGE_LOOP('',(#21829,#21830,#21831,#21832));
#5030=EDGE_LOOP('',(#21833,#21834,#21835,#21836));
#5031=EDGE_LOOP('',(#21837,#21838,#21839,#21840,#21841,#21842,#21843,#21844,
#21845,#21846));
#5032=EDGE_LOOP('',(#21847,#21848,#21849,#21850));
#5033=EDGE_LOOP('',(#21851,#21852,#21853,#21854));
#5034=EDGE_LOOP('',(#21855,#21856,#21857,#21858));
#5035=EDGE_LOOP('',(#21859,#21860,#21861,#21862));
#5036=EDGE_LOOP('',(#21863,#21864,#21865,#21866));
#5037=EDGE_LOOP('',(#21867,#21868,#21869,#21870));
#5038=EDGE_LOOP('',(#21871,#21872,#21873,#21874));
#5039=EDGE_LOOP('',(#21875,#21876,#21877,#21878));
#5040=EDGE_LOOP('',(#21879));
#5041=EDGE_LOOP('',(#21880,#21881,#21882,#21883,#21884,#21885,#21886,#21887,
#21888,#21889,#21890,#21891,#21892,#21893,#21894,#21895,#21896,#21897,#21898,
#21899,#21900,#21901,#21902,#21903,#21904,#21905,#21906,#21907,#21908,#21909,
#21910,#21911,#21912,#21913,#21914,#21915,#21916,#21917,#21918,#21919,#21920,
#21921,#21922,#21923,#21924,#21925,#21926,#21927));
#5042=EDGE_LOOP('',(#21928,#21929,#21930,#21931,#21932,#21933,#21934,#21935,
#21936,#21937,#21938,#21939,#21940,#21941,#21942,#21943,#21944,#21945,#21946,
#21947,#21948,#21949,#21950,#21951,#21952,#21953,#21954,#21955,#21956,#21957,
#21958,#21959,#21960,#21961,#21962,#21963,#21964,#21965,#21966,#21967,#21968,
#21969,#21970,#21971));
#5043=EDGE_LOOP('',(#21972,#21973,#21974,#21975));
#5044=EDGE_LOOP('',(#21976,#21977,#21978,#21979));
#5045=EDGE_LOOP('',(#21980,#21981,#21982,#21983));
#5046=EDGE_LOOP('',(#21984,#21985,#21986,#21987));
#5047=EDGE_LOOP('',(#21988,#21989,#21990,#21991,#21992,#21993,#21994));
#5048=EDGE_LOOP('',(#21995,#21996,#21997,#21998,#21999,#22000,#22001));
#5049=EDGE_LOOP('',(#22002,#22003,#22004,#22005,#22006,#22007,#22008));
#5050=EDGE_LOOP('',(#22009,#22010,#22011,#22012,#22013,#22014,#22015));
#5051=EDGE_LOOP('',(#22016,#22017,#22018,#22019));
#5052=EDGE_LOOP('',(#22020,#22021,#22022,#22023));
#5053=EDGE_LOOP('',(#22024,#22025,#22026,#22027));
#5054=EDGE_LOOP('',(#22028));
#5055=EDGE_LOOP('',(#22029,#22030,#22031));
#5056=EDGE_LOOP('',(#22032,#22033,#22034));
#5057=EDGE_LOOP('',(#22035,#22036,#22037,#22038,#22039,#22040));
#5058=EDGE_LOOP('',(#22041,#22042,#22043,#22044,#22045,#22046,#22047,#22048,
#22049,#22050,#22051,#22052,#22053));
#5059=EDGE_LOOP('',(#22054,#22055,#22056,#22057,#22058,#22059));
#5060=EDGE_LOOP('',(#22060,#22061,#22062,#22063,#22064,#22065));
#5061=EDGE_LOOP('',(#22066));
#5062=EDGE_LOOP('',(#22067,#22068,#22069,#22070,#22071,#22072));
#5063=EDGE_LOOP('',(#22073));
#5064=EDGE_LOOP('',(#22074,#22075,#22076));
#5065=EDGE_LOOP('',(#22077,#22078,#22079));
#5066=EDGE_LOOP('',(#22080,#22081,#22082));
#5067=EDGE_LOOP('',(#22083,#22084,#22085));
#5068=EDGE_LOOP('',(#22086,#22087,#22088));
#5069=EDGE_LOOP('',(#22089,#22090,#22091));
#5070=EDGE_LOOP('',(#22092,#22093,#22094,#22095,#22096));
#5071=EDGE_LOOP('',(#22097,#22098,#22099,#22100,#22101));
#5072=EDGE_LOOP('',(#22102,#22103,#22104,#22105,#22106));
#5073=EDGE_LOOP('',(#22107,#22108,#22109,#22110,#22111));
#5074=EDGE_LOOP('',(#22112,#22113,#22114,#22115,#22116));
#5075=EDGE_LOOP('',(#22117,#22118,#22119,#22120,#22121));
#5076=EDGE_LOOP('',(#22122,#22123,#22124,#22125,#22126,#22127));
#5077=EDGE_LOOP('',(#22128,#22129,#22130));
#5078=EDGE_LOOP('',(#22131,#22132,#22133));
#5079=EDGE_LOOP('',(#22134,#22135,#22136));
#5080=EDGE_LOOP('',(#22137,#22138,#22139));
#5081=EDGE_LOOP('',(#22140,#22141,#22142));
#5082=EDGE_LOOP('',(#22143,#22144,#22145));
#5083=EDGE_LOOP('',(#22146,#22147,#22148));
#5084=EDGE_LOOP('',(#22149,#22150,#22151));
#5085=EDGE_LOOP('',(#22152,#22153,#22154));
#5086=EDGE_LOOP('',(#22155,#22156,#22157));
#5087=EDGE_LOOP('',(#22158,#22159,#22160,#22161,#22162,#22163));
#5088=EDGE_LOOP('',(#22164,#22165,#22166,#22167,#22168,#22169));
#5089=EDGE_LOOP('',(#22170,#22171,#22172,#22173,#22174,#22175));
#5090=EDGE_LOOP('',(#22176,#22177,#22178,#22179,#22180,#22181));
#5091=EDGE_LOOP('',(#22182,#22183,#22184,#22185,#22186,#22187));
#5092=EDGE_LOOP('',(#22188,#22189,#22190,#22191,#22192,#22193));
#5093=EDGE_LOOP('',(#22194));
#5094=EDGE_LOOP('',(#22195));
#5095=EDGE_LOOP('',(#22196,#22197,#22198,#22199));
#5096=EDGE_LOOP('',(#22200,#22201,#22202));
#5097=EDGE_LOOP('',(#22203,#22204,#22205,#22206));
#5098=EDGE_LOOP('',(#22207,#22208,#22209));
#5099=EDGE_LOOP('',(#22210,#22211,#22212,#22213));
#5100=EDGE_LOOP('',(#22214,#22215,#22216));
#5101=EDGE_LOOP('',(#22217,#22218,#22219,#22220));
#5102=EDGE_LOOP('',(#22221,#22222,#22223));
#5103=EDGE_LOOP('',(#22224,#22225,#22226,#22227));
#5104=EDGE_LOOP('',(#22228,#22229,#22230));
#5105=EDGE_LOOP('',(#22231,#22232,#22233,#22234));
#5106=EDGE_LOOP('',(#22235,#22236,#22237));
#5107=EDGE_LOOP('',(#22238,#22239,#22240,#22241));
#5108=EDGE_LOOP('',(#22242,#22243,#22244));
#5109=EDGE_LOOP('',(#22245,#22246,#22247,#22248));
#5110=EDGE_LOOP('',(#22249,#22250,#22251));
#5111=EDGE_LOOP('',(#22252,#22253,#22254,#22255));
#5112=EDGE_LOOP('',(#22256,#22257,#22258,#22259,#22260,#22261,#22262,#22263,
#22264,#22265));
#5113=EDGE_LOOP('',(#22266,#22267,#22268,#22269));
#5114=EDGE_LOOP('',(#22270,#22271,#22272,#22273,#22274,#22275,#22276,#22277,
#22278,#22279));
#5115=EDGE_LOOP('',(#22280,#22281,#22282,#22283));
#5116=EDGE_LOOP('',(#22284,#22285,#22286,#22287));
#5117=EDGE_LOOP('',(#22288,#22289,#22290,#22291));
#5118=EDGE_LOOP('',(#22292,#22293,#22294,#22295));
#5119=EDGE_LOOP('',(#22296,#22297,#22298,#22299));
#5120=EDGE_LOOP('',(#22300));
#5121=EDGE_LOOP('',(#22301));
#5122=EDGE_LOOP('',(#22302));
#5123=EDGE_LOOP('',(#22303));
#5124=EDGE_LOOP('',(#22304));
#5125=EDGE_LOOP('',(#22305));
#5126=EDGE_LOOP('',(#22306));
#5127=EDGE_LOOP('',(#22307));
#5128=EDGE_LOOP('',(#22308,#22309,#22310,#22311));
#5129=EDGE_LOOP('',(#22312,#22313,#22314,#22315));
#5130=EDGE_LOOP('',(#22316,#22317,#22318,#22319));
#5131=EDGE_LOOP('',(#22320,#22321,#22322,#22323,#22324));
#5132=EDGE_LOOP('',(#22325,#22326,#22327,#22328,#22329,#22330,#22331,#22332,
#22333));
#5133=EDGE_LOOP('',(#22334,#22335,#22336,#22337,#22338));
#5134=EDGE_LOOP('',(#22339,#22340,#22341,#22342));
#5135=EDGE_LOOP('',(#22343,#22344,#22345,#22346));
#5136=EDGE_LOOP('',(#22347));
#5137=EDGE_LOOP('',(#22348,#22349,#22350,#22351,#22352,#22353));
#5138=EDGE_LOOP('',(#22354));
#5139=EDGE_LOOP('',(#22355));
#5140=EDGE_LOOP('',(#22356));
#5141=EDGE_LOOP('',(#22357));
#5142=EDGE_LOOP('',(#22358));
#5143=EDGE_LOOP('',(#22359,#22360,#22361,#22362,#22363));
#5144=EDGE_LOOP('',(#22364,#22365,#22366,#22367,#22368));
#5145=EDGE_LOOP('',(#22369,#22370,#22371,#22372,#22373));
#5146=EDGE_LOOP('',(#22374,#22375,#22376,#22377,#22378));
#5147=EDGE_LOOP('',(#22379,#22380,#22381,#22382,#22383));
#5148=EDGE_LOOP('',(#22384,#22385,#22386,#22387,#22388));
#5149=EDGE_LOOP('',(#22389,#22390,#22391));
#5150=EDGE_LOOP('',(#22392,#22393,#22394,#22395));
#5151=EDGE_LOOP('',(#22396,#22397,#22398));
#5152=EDGE_LOOP('',(#22399,#22400,#22401));
#5153=EDGE_LOOP('',(#22402,#22403,#22404));
#5154=EDGE_LOOP('',(#22405,#22406,#22407));
#5155=EDGE_LOOP('',(#22408,#22409,#22410,#22411));
#5156=EDGE_LOOP('',(#22412,#22413,#22414,#22415));
#5157=EDGE_LOOP('',(#22416));
#5158=EDGE_LOOP('',(#22417));
#5159=EDGE_LOOP('',(#22418));
#5160=EDGE_LOOP('',(#22419));
#5161=EDGE_LOOP('',(#22420,#22421,#22422,#22423));
#5162=EDGE_LOOP('',(#22424,#22425,#22426,#22427));
#5163=EDGE_LOOP('',(#22428,#22429,#22430,#22431));
#5164=EDGE_LOOP('',(#22432,#22433,#22434,#22435));
#5165=EDGE_LOOP('',(#22436,#22437,#22438,#22439));
#5166=EDGE_LOOP('',(#22440,#22441,#22442,#22443));
#5167=EDGE_LOOP('',(#22444,#22445,#22446,#22447));
#5168=EDGE_LOOP('',(#22448,#22449,#22450,#22451));
#5169=EDGE_LOOP('',(#22452,#22453,#22454,#22455,#22456));
#5170=EDGE_LOOP('',(#22457,#22458,#22459,#22460,#22461));
#5171=EDGE_LOOP('',(#22462));
#5172=EDGE_LOOP('',(#22463));
#5173=EDGE_LOOP('',(#22464,#22465,#22466,#22467,#22468,#22469));
#5174=EDGE_LOOP('',(#22470));
#5175=EDGE_LOOP('',(#22471));
#5176=EDGE_LOOP('',(#22472,#22473,#22474,#22475));
#5177=EDGE_LOOP('',(#22476,#22477,#22478,#22479));
#5178=EDGE_LOOP('',(#22480,#22481,#22482,#22483));
#5179=EDGE_LOOP('',(#22484,#22485,#22486,#22487));
#5180=EDGE_LOOP('',(#22488,#22489,#22490,#22491));
#5181=EDGE_LOOP('',(#22492,#22493,#22494,#22495));
#5182=EDGE_LOOP('',(#22496,#22497,#22498,#22499,#22500,#22501));
#5183=EDGE_LOOP('',(#22502,#22503,#22504,#22505,#22506));
#5184=EDGE_LOOP('',(#22507,#22508,#22509,#22510,#22511,#22512,#22513,#22514,
#22515));
#5185=EDGE_LOOP('',(#22516,#22517,#22518,#22519,#22520));
#5186=EDGE_LOOP('',(#22521,#22522,#22523,#22524));
#5187=EDGE_LOOP('',(#22525,#22526,#22527,#22528));
#5188=EDGE_LOOP('',(#22529));
#5189=EDGE_LOOP('',(#22530,#22531,#22532,#22533,#22534,#22535));
#5190=EDGE_LOOP('',(#22536));
#5191=EDGE_LOOP('',(#22537));
#5192=EDGE_LOOP('',(#22538));
#5193=EDGE_LOOP('',(#22539));
#5194=EDGE_LOOP('',(#22540));
#5195=EDGE_LOOP('',(#22541,#22542,#22543,#22544,#22545));
#5196=EDGE_LOOP('',(#22546,#22547,#22548,#22549,#22550));
#5197=EDGE_LOOP('',(#22551,#22552,#22553,#22554,#22555));
#5198=EDGE_LOOP('',(#22556,#22557,#22558,#22559,#22560));
#5199=EDGE_LOOP('',(#22561,#22562,#22563,#22564,#22565));
#5200=EDGE_LOOP('',(#22566,#22567,#22568,#22569,#22570));
#5201=EDGE_LOOP('',(#22571,#22572,#22573));
#5202=EDGE_LOOP('',(#22574,#22575,#22576,#22577));
#5203=EDGE_LOOP('',(#22578,#22579,#22580));
#5204=EDGE_LOOP('',(#22581,#22582,#22583));
#5205=EDGE_LOOP('',(#22584,#22585,#22586));
#5206=EDGE_LOOP('',(#22587,#22588,#22589));
#5207=EDGE_LOOP('',(#22590,#22591,#22592,#22593));
#5208=EDGE_LOOP('',(#22594,#22595,#22596,#22597));
#5209=EDGE_LOOP('',(#22598));
#5210=EDGE_LOOP('',(#22599));
#5211=EDGE_LOOP('',(#22600));
#5212=EDGE_LOOP('',(#22601));
#5213=EDGE_LOOP('',(#22602,#22603,#22604,#22605));
#5214=EDGE_LOOP('',(#22606,#22607,#22608,#22609));
#5215=EDGE_LOOP('',(#22610,#22611,#22612,#22613));
#5216=EDGE_LOOP('',(#22614,#22615,#22616,#22617));
#5217=EDGE_LOOP('',(#22618,#22619,#22620,#22621));
#5218=EDGE_LOOP('',(#22622,#22623,#22624,#22625));
#5219=EDGE_LOOP('',(#22626,#22627,#22628,#22629));
#5220=EDGE_LOOP('',(#22630,#22631,#22632,#22633));
#5221=EDGE_LOOP('',(#22634,#22635,#22636,#22637,#22638));
#5222=EDGE_LOOP('',(#22639,#22640,#22641,#22642,#22643));
#5223=EDGE_LOOP('',(#22644));
#5224=EDGE_LOOP('',(#22645));
#5225=EDGE_LOOP('',(#22646,#22647,#22648,#22649,#22650,#22651));
#5226=EDGE_LOOP('',(#22652));
#5227=EDGE_LOOP('',(#22653));
#5228=EDGE_LOOP('',(#22654,#22655,#22656,#22657));
#5229=EDGE_LOOP('',(#22658,#22659,#22660,#22661));
#5230=EDGE_LOOP('',(#22662,#22663,#22664,#22665));
#5231=EDGE_LOOP('',(#22666,#22667,#22668,#22669));
#5232=EDGE_LOOP('',(#22670,#22671,#22672,#22673));
#5233=EDGE_LOOP('',(#22674,#22675,#22676,#22677));
#5234=EDGE_LOOP('',(#22678,#22679,#22680,#22681,#22682,#22683));
#5235=EDGE_LOOP('',(#22684,#22685,#22686,#22687));
#5236=EDGE_LOOP('',(#22688,#22689,#22690,#22691));
#5237=EDGE_LOOP('',(#22692,#22693,#22694,#22695,#22696));
#5238=EDGE_LOOP('',(#22697,#22698,#22699,#22700,#22701));
#5239=EDGE_LOOP('',(#22702));
#5240=EDGE_LOOP('',(#22703));
#5241=EDGE_LOOP('',(#22704,#22705,#22706,#22707,#22708,#22709));
#5242=EDGE_LOOP('',(#22710));
#5243=EDGE_LOOP('',(#22711));
#5244=EDGE_LOOP('',(#22712,#22713,#22714,#22715));
#5245=EDGE_LOOP('',(#22716,#22717,#22718,#22719));
#5246=EDGE_LOOP('',(#22720,#22721,#22722,#22723));
#5247=EDGE_LOOP('',(#22724,#22725,#22726,#22727));
#5248=EDGE_LOOP('',(#22728,#22729,#22730,#22731));
#5249=EDGE_LOOP('',(#22732,#22733,#22734,#22735));
#5250=EDGE_LOOP('',(#22736,#22737,#22738,#22739,#22740,#22741));
#5251=LINE('',#34638,#7218);
#5252=LINE('',#34644,#7219);
#5253=LINE('',#34650,#7220);
#5254=LINE('',#34656,#7221);
#5255=LINE('',#34662,#7222);
#5256=LINE('',#34668,#7223);
#5257=LINE('',#34674,#7224);
#5258=LINE('',#34680,#7225);
#5259=LINE('',#34686,#7226);
#5260=LINE('',#34690,#7227);
#5261=LINE('',#34695,#7228);
#5262=LINE('',#34699,#7229);
#5263=LINE('',#34704,#7230);
#5264=LINE('',#34708,#7231);
#5265=LINE('',#34713,#7232);
#5266=LINE('',#34717,#7233);
#5267=LINE('',#34721,#7234);
#5268=LINE('',#34723,#7235);
#5269=LINE('',#34725,#7236);
#5270=LINE('',#34726,#7237);
#5271=LINE('',#34730,#7238);
#5272=LINE('',#34732,#7239);
#5273=LINE('',#34734,#7240);
#5274=LINE('',#34735,#7241);
#5275=LINE('',#34738,#7242);
#5276=LINE('',#34740,#7243);
#5277=LINE('',#34741,#7244);
#5278=LINE('',#34743,#7245);
#5279=LINE('',#34744,#7246);
#5280=LINE('',#34747,#7247);
#5281=LINE('',#34749,#7248);
#5282=LINE('',#34750,#7249);
#5283=LINE('',#34753,#7250);
#5284=LINE('',#34755,#7251);
#5285=LINE('',#34756,#7252);
#5286=LINE('',#34759,#7253);
#5287=LINE('',#34761,#7254);
#5288=LINE('',#34762,#7255);
#5289=LINE('',#34764,#7256);
#5290=LINE('',#34766,#7257);
#5291=LINE('',#34775,#7258);
#5292=LINE('',#34779,#7259);
#5293=LINE('',#34800,#7260);
#5294=LINE('',#34810,#7261);
#5295=LINE('',#34815,#7262);
#5296=LINE('',#34824,#7263);
#5297=LINE('',#34831,#7264);
#5298=LINE('',#34834,#7265);
#5299=LINE('',#34845,#7266);
#5300=LINE('',#34850,#7267);
#5301=LINE('',#34858,#7268);
#5302=LINE('',#34862,#7269);
#5303=LINE('',#34883,#7270);
#5304=LINE('',#34885,#7271);
#5305=LINE('',#34886,#7272);
#5306=LINE('',#34890,#7273);
#5307=LINE('',#34891,#7274);
#5308=LINE('',#34894,#7275);
#5309=LINE('',#34895,#7276);
#5310=LINE('',#34937,#7277);
#5311=LINE('',#34976,#7278);
#5312=LINE('',#34982,#7279);
#5313=LINE('',#34988,#7280);
#5314=LINE('',#34994,#7281);
#5315=LINE('',#35000,#7282);
#5316=LINE('',#35006,#7283);
#5317=LINE('',#35012,#7284);
#5318=LINE('',#35018,#7285);
#5319=LINE('',#35024,#7286);
#5320=LINE('',#35030,#7287);
#5321=LINE('',#35036,#7288);
#5322=LINE('',#35042,#7289);
#5323=LINE('',#35051,#7290);
#5324=LINE('',#35055,#7291);
#5325=LINE('',#35107,#7292);
#5326=LINE('',#35110,#7293);
#5327=LINE('',#35113,#7294);
#5328=LINE('',#35115,#7295);
#5329=LINE('',#35166,#7296);
#5330=LINE('',#35167,#7297);
#5331=LINE('',#35183,#7298);
#5332=LINE('',#35189,#7299);
#5333=LINE('',#35195,#7300);
#5334=LINE('',#35201,#7301);
#5335=LINE('',#35207,#7302);
#5336=LINE('',#35213,#7303);
#5337=LINE('',#35219,#7304);
#5338=LINE('',#35224,#7305);
#5339=LINE('',#35239,#7306);
#5340=LINE('',#35254,#7307);
#5341=LINE('',#35269,#7308);
#5342=LINE('',#35285,#7309);
#5343=LINE('',#35291,#7310);
#5344=LINE('',#35297,#7311);
#5345=LINE('',#35303,#7312);
#5346=LINE('',#35309,#7313);
#5347=LINE('',#35315,#7314);
#5348=LINE('',#35321,#7315);
#5349=LINE('',#35327,#7316);
#5350=LINE('',#35336,#7317);
#5351=LINE('',#35338,#7318);
#5352=LINE('',#35340,#7319);
#5353=LINE('',#35342,#7320);
#5354=LINE('',#35344,#7321);
#5355=LINE('',#35346,#7322);
#5356=LINE('',#35348,#7323);
#5357=LINE('',#35350,#7324);
#5358=LINE('',#35352,#7325);
#5359=LINE('',#35354,#7326);
#5360=LINE('',#35356,#7327);
#5361=LINE('',#35357,#7328);
#5362=LINE('',#35360,#7329);
#5363=LINE('',#35362,#7330);
#5364=LINE('',#35364,#7331);
#5365=LINE('',#35366,#7332);
#5366=LINE('',#35368,#7333);
#5367=LINE('',#35370,#7334);
#5368=LINE('',#35372,#7335);
#5369=LINE('',#35373,#7336);
#5370=LINE('',#35377,#7337);
#5371=LINE('',#35378,#7338);
#5372=LINE('',#35379,#7339);
#5373=LINE('',#35382,#7340);
#5374=LINE('',#35383,#7341);
#5375=LINE('',#35386,#7342);
#5376=LINE('',#35387,#7343);
#5377=LINE('',#35390,#7344);
#5378=LINE('',#35391,#7345);
#5379=LINE('',#35394,#7346);
#5380=LINE('',#35395,#7347);
#5381=LINE('',#35398,#7348);
#5382=LINE('',#35399,#7349);
#5383=LINE('',#35402,#7350);
#5384=LINE('',#35403,#7351);
#5385=LINE('',#35406,#7352);
#5386=LINE('',#35407,#7353);
#5387=LINE('',#35410,#7354);
#5388=LINE('',#35411,#7355);
#5389=LINE('',#35414,#7356);
#5390=LINE('',#35415,#7357);
#5391=LINE('',#35418,#7358);
#5392=LINE('',#35419,#7359);
#5393=LINE('',#35421,#7360);
#5394=LINE('',#35426,#7361);
#5395=LINE('',#35428,#7362);
#5396=LINE('',#35430,#7363);
#5397=LINE('',#35432,#7364);
#5398=LINE('',#35434,#7365);
#5399=LINE('',#35436,#7366);
#5400=LINE('',#35438,#7367);
#5401=LINE('',#35439,#7368);
#5402=LINE('',#35441,#7369);
#5403=LINE('',#35442,#7370);
#5404=LINE('',#35444,#7371);
#5405=LINE('',#35446,#7372);
#5406=LINE('',#35448,#7373);
#5407=LINE('',#35450,#7374);
#5408=LINE('',#35452,#7375);
#5409=LINE('',#35454,#7376);
#5410=LINE('',#35459,#7377);
#5411=LINE('',#35461,#7378);
#5412=LINE('',#35463,#7379);
#5413=LINE('',#35465,#7380);
#5414=LINE('',#35467,#7381);
#5415=LINE('',#35468,#7382);
#5416=LINE('',#35472,#7383);
#5417=LINE('',#35474,#7384);
#5418=LINE('',#35476,#7385);
#5419=LINE('',#35478,#7386);
#5420=LINE('',#35480,#7387);
#5421=LINE('',#35481,#7388);
#5422=LINE('',#35485,#7389);
#5423=LINE('',#35487,#7390);
#5424=LINE('',#35489,#7391);
#5425=LINE('',#35491,#7392);
#5426=LINE('',#35493,#7393);
#5427=LINE('',#35494,#7394);
#5428=LINE('',#35498,#7395);
#5429=LINE('',#35500,#7396);
#5430=LINE('',#35502,#7397);
#5431=LINE('',#35504,#7398);
#5432=LINE('',#35506,#7399);
#5433=LINE('',#35507,#7400);
#5434=LINE('',#35510,#7401);
#5435=LINE('',#35511,#7402);
#5436=LINE('',#35513,#7403);
#5437=LINE('',#35514,#7404);
#5438=LINE('',#35516,#7405);
#5439=LINE('',#35518,#7406);
#5440=LINE('',#35519,#7407);
#5441=LINE('',#35521,#7408);
#5442=LINE('',#35523,#7409);
#5443=LINE('',#35524,#7410);
#5444=LINE('',#35526,#7411);
#5445=LINE('',#35528,#7412);
#5446=LINE('',#35529,#7413);
#5447=LINE('',#35531,#7414);
#5448=LINE('',#35533,#7415);
#5449=LINE('',#35534,#7416);
#5450=LINE('',#35536,#7417);
#5451=LINE('',#35537,#7418);
#5452=LINE('',#35546,#7419);
#5453=LINE('',#35547,#7420);
#5454=LINE('',#35549,#7421);
#5455=LINE('',#35550,#7422);
#5456=LINE('',#35552,#7423);
#5457=LINE('',#35554,#7424);
#5458=LINE('',#35555,#7425);
#5459=LINE('',#35557,#7426);
#5460=LINE('',#35559,#7427);
#5461=LINE('',#35560,#7428);
#5462=LINE('',#35562,#7429);
#5463=LINE('',#35564,#7430);
#5464=LINE('',#35565,#7431);
#5465=LINE('',#35567,#7432);
#5466=LINE('',#35569,#7433);
#5467=LINE('',#35570,#7434);
#5468=LINE('',#35572,#7435);
#5469=LINE('',#35573,#7436);
#5470=LINE('',#35582,#7437);
#5471=LINE('',#35583,#7438);
#5472=LINE('',#35585,#7439);
#5473=LINE('',#35586,#7440);
#5474=LINE('',#35588,#7441);
#5475=LINE('',#35590,#7442);
#5476=LINE('',#35591,#7443);
#5477=LINE('',#35593,#7444);
#5478=LINE('',#35595,#7445);
#5479=LINE('',#35596,#7446);
#5480=LINE('',#35598,#7447);
#5481=LINE('',#35600,#7448);
#5482=LINE('',#35601,#7449);
#5483=LINE('',#35603,#7450);
#5484=LINE('',#35605,#7451);
#5485=LINE('',#35606,#7452);
#5486=LINE('',#35608,#7453);
#5487=LINE('',#35609,#7454);
#5488=LINE('',#35618,#7455);
#5489=LINE('',#35619,#7456);
#5490=LINE('',#35621,#7457);
#5491=LINE('',#35622,#7458);
#5492=LINE('',#35624,#7459);
#5493=LINE('',#35626,#7460);
#5494=LINE('',#35627,#7461);
#5495=LINE('',#35629,#7462);
#5496=LINE('',#35631,#7463);
#5497=LINE('',#35632,#7464);
#5498=LINE('',#35634,#7465);
#5499=LINE('',#35636,#7466);
#5500=LINE('',#35637,#7467);
#5501=LINE('',#35639,#7468);
#5502=LINE('',#35641,#7469);
#5503=LINE('',#35642,#7470);
#5504=LINE('',#35644,#7471);
#5505=LINE('',#35645,#7472);
#5506=LINE('',#35694,#7473);
#5507=LINE('',#35734,#7474);
#5508=LINE('',#35741,#7475);
#5509=LINE('',#35744,#7476);
#5510=LINE('',#35750,#7477);
#5511=LINE('',#35753,#7478);
#5512=LINE('',#35758,#7479);
#5513=LINE('',#35765,#7480);
#5514=LINE('',#35768,#7481);
#5515=LINE('',#35774,#7482);
#5516=LINE('',#35777,#7483);
#5517=LINE('',#35783,#7484);
#5518=LINE('',#35786,#7485);
#5519=LINE('',#35789,#7486);
#5520=LINE('',#35790,#7487);
#5521=LINE('',#35791,#7488);
#5522=LINE('',#35792,#7489);
#5523=LINE('',#35794,#7490);
#5524=LINE('',#35795,#7491);
#5525=LINE('',#35796,#7492);
#5526=LINE('',#35797,#7493);
#5527=LINE('',#35806,#7494);
#5528=LINE('',#35813,#7495);
#5529=LINE('',#35817,#7496);
#5530=LINE('',#35822,#7497);
#5531=LINE('',#35824,#7498);
#5532=LINE('',#35826,#7499);
#5533=LINE('',#35828,#7500);
#5534=LINE('',#35830,#7501);
#5535=LINE('',#35831,#7502);
#5536=LINE('',#35834,#7503);
#5537=LINE('',#35836,#7504);
#5538=LINE('',#35837,#7505);
#5539=LINE('',#35840,#7506);
#5540=LINE('',#35841,#7507);
#5541=LINE('',#35844,#7508);
#5542=LINE('',#35845,#7509);
#5543=LINE('',#35848,#7510);
#5544=LINE('',#35849,#7511);
#5545=LINE('',#35852,#7512);
#5546=LINE('',#35853,#7513);
#5547=LINE('',#35855,#7514);
#5548=LINE('',#35862,#7515);
#5549=LINE('',#35868,#7516);
#5550=LINE('',#35882,#7517);
#5551=LINE('',#35888,#7518);
#5552=LINE('',#35894,#7519);
#5553=LINE('',#35899,#7520);
#5554=LINE('',#35901,#7521);
#5555=LINE('',#35903,#7522);
#5556=LINE('',#35905,#7523);
#5557=LINE('',#35907,#7524);
#5558=LINE('',#35909,#7525);
#5559=LINE('',#35911,#7526);
#5560=LINE('',#35913,#7527);
#5561=LINE('',#35915,#7528);
#5562=LINE('',#35917,#7529);
#5563=LINE('',#35919,#7530);
#5564=LINE('',#35920,#7531);
#5565=LINE('',#35924,#7532);
#5566=LINE('',#35926,#7533);
#5567=LINE('',#35928,#7534);
#5568=LINE('',#35930,#7535);
#5569=LINE('',#35932,#7536);
#5570=LINE('',#35934,#7537);
#5571=LINE('',#35936,#7538);
#5572=LINE('',#35938,#7539);
#5573=LINE('',#35940,#7540);
#5574=LINE('',#35942,#7541);
#5575=LINE('',#35944,#7542);
#5576=LINE('',#35945,#7543);
#5577=LINE('',#35947,#7544);
#5578=LINE('',#35948,#7545);
#5579=LINE('',#35950,#7546);
#5580=LINE('',#35952,#7547);
#5581=LINE('',#35954,#7548);
#5582=LINE('',#35956,#7549);
#5583=LINE('',#35958,#7550);
#5584=LINE('',#35960,#7551);
#5585=LINE('',#35962,#7552);
#5586=LINE('',#35964,#7553);
#5587=LINE('',#35966,#7554);
#5588=LINE('',#35968,#7555);
#5589=LINE('',#35978,#7556);
#5590=LINE('',#35988,#7557);
#5591=LINE('',#35994,#7558);
#5592=LINE('',#36004,#7559);
#5593=LINE('',#36014,#7560);
#5594=LINE('',#36020,#7561);
#5595=LINE('',#36033,#7562);
#5596=LINE('',#36039,#7563);
#5597=LINE('',#36046,#7564);
#5598=LINE('',#36049,#7565);
#5599=LINE('',#36055,#7566);
#5600=LINE('',#36058,#7567);
#5601=LINE('',#36062,#7568);
#5602=LINE('',#36066,#7569);
#5603=LINE('',#36071,#7570);
#5604=LINE('',#36075,#7571);
#5605=LINE('',#36076,#7572);
#5606=LINE('',#36077,#7573);
#5607=LINE('',#36081,#7574);
#5608=LINE('',#36082,#7575);
#5609=LINE('',#36084,#7576);
#5610=LINE('',#36086,#7577);
#5611=LINE('',#36090,#7578);
#5612=LINE('',#36095,#7579);
#5613=LINE('',#36098,#7580);
#5614=LINE('',#36099,#7581);
#5615=LINE('',#36101,#7582);
#5616=LINE('',#36103,#7583);
#5617=LINE('',#36106,#7584);
#5618=LINE('',#36108,#7585);
#5619=LINE('',#36110,#7586);
#5620=LINE('',#36112,#7587);
#5621=LINE('',#36122,#7588);
#5622=LINE('',#36128,#7589);
#5623=LINE('',#36134,#7590);
#5624=LINE('',#36140,#7591);
#5625=LINE('',#36145,#7592);
#5626=LINE('',#36147,#7593);
#5627=LINE('',#36149,#7594);
#5628=LINE('',#36150,#7595);
#5629=LINE('',#36153,#7596);
#5630=LINE('',#36155,#7597);
#5631=LINE('',#36157,#7598);
#5632=LINE('',#36159,#7599);
#5633=LINE('',#36160,#7600);
#5634=LINE('',#36164,#7601);
#5635=LINE('',#36165,#7602);
#5636=LINE('',#36167,#7603);
#5637=LINE('',#36168,#7604);
#5638=LINE('',#36172,#7605);
#5639=LINE('',#36174,#7606);
#5640=LINE('',#36175,#7607);
#5641=LINE('',#36177,#7608);
#5642=LINE('',#36178,#7609);
#5643=LINE('',#36181,#7610);
#5644=LINE('',#36183,#7611);
#5645=LINE('',#36184,#7612);
#5646=LINE('',#36185,#7613);
#5647=LINE('',#36188,#7614);
#5648=LINE('',#36189,#7615);
#5649=LINE('',#36193,#7616);
#5650=LINE('',#36194,#7617);
#5651=LINE('',#36196,#7618);
#5652=LINE('',#36199,#7619);
#5653=LINE('',#36200,#7620);
#5654=LINE('',#36202,#7621);
#5655=LINE('',#36209,#7622);
#5656=LINE('',#36215,#7623);
#5657=LINE('',#36221,#7624);
#5658=LINE('',#36227,#7625);
#5659=LINE('',#36232,#7626);
#5660=LINE('',#36234,#7627);
#5661=LINE('',#36236,#7628);
#5662=LINE('',#36237,#7629);
#5663=LINE('',#36240,#7630);
#5664=LINE('',#36242,#7631);
#5665=LINE('',#36244,#7632);
#5666=LINE('',#36246,#7633);
#5667=LINE('',#36247,#7634);
#5668=LINE('',#36251,#7635);
#5669=LINE('',#36252,#7636);
#5670=LINE('',#36254,#7637);
#5671=LINE('',#36255,#7638);
#5672=LINE('',#36259,#7639);
#5673=LINE('',#36261,#7640);
#5674=LINE('',#36262,#7641);
#5675=LINE('',#36264,#7642);
#5676=LINE('',#36265,#7643);
#5677=LINE('',#36268,#7644);
#5678=LINE('',#36270,#7645);
#5679=LINE('',#36271,#7646);
#5680=LINE('',#36272,#7647);
#5681=LINE('',#36275,#7648);
#5682=LINE('',#36276,#7649);
#5683=LINE('',#36280,#7650);
#5684=LINE('',#36281,#7651);
#5685=LINE('',#36283,#7652);
#5686=LINE('',#36286,#7653);
#5687=LINE('',#36287,#7654);
#5688=LINE('',#36289,#7655);
#5689=LINE('',#36296,#7656);
#5690=LINE('',#36302,#7657);
#5691=LINE('',#36308,#7658);
#5692=LINE('',#36314,#7659);
#5693=LINE('',#36320,#7660);
#5694=LINE('',#36326,#7661);
#5695=LINE('',#36332,#7662);
#5696=LINE('',#36338,#7663);
#5697=LINE('',#36344,#7664);
#5698=LINE('',#36350,#7665);
#5699=LINE('',#36356,#7666);
#5700=LINE('',#36362,#7667);
#5701=LINE('',#36367,#7668);
#5702=LINE('',#36369,#7669);
#5703=LINE('',#36371,#7670);
#5704=LINE('',#36372,#7671);
#5705=LINE('',#36376,#7672);
#5706=LINE('',#36377,#7673);
#5707=LINE('',#36378,#7674);
#5708=LINE('',#36381,#7675);
#5709=LINE('',#36382,#7676);
#5710=LINE('',#36385,#7677);
#5711=LINE('',#36386,#7678);
#5712=LINE('',#36388,#7679);
#5713=LINE('',#36401,#7680);
#5714=LINE('',#36407,#7681);
#5715=LINE('',#36415,#7682);
#5716=LINE('',#50658,#7683);
#5717=LINE('',#50665,#7684);
#5718=LINE('',#51649,#7685);
#5719=LINE('',#51656,#7686);
#5720=LINE('',#51665,#7687);
#5721=LINE('',#51667,#7688);
#5722=LINE('',#51669,#7689);
#5723=LINE('',#51671,#7690);
#5724=LINE('',#51673,#7691);
#5725=LINE('',#51674,#7692);
#5726=LINE('',#51679,#7693);
#5727=LINE('',#51683,#7694);
#5728=LINE('',#51685,#7695);
#5729=LINE('',#51687,#7696);
#5730=LINE('',#51689,#7697);
#5731=LINE('',#51691,#7698);
#5732=LINE('',#51692,#7699);
#5733=LINE('',#51694,#7700);
#5734=LINE('',#51695,#7701);
#5735=LINE('',#51697,#7702);
#5736=LINE('',#51699,#7703);
#5737=LINE('',#51701,#7704);
#5738=LINE('',#51703,#7705);
#5739=LINE('',#51720,#7706);
#5740=LINE('',#51724,#7707);
#5741=LINE('',#51725,#7708);
#5742=LINE('',#51729,#7709);
#5743=LINE('',#51733,#7710);
#5744=LINE('',#51754,#7711);
#5745=LINE('',#51778,#7712);
#5746=LINE('',#51779,#7713);
#5747=LINE('',#51782,#7714);
#5748=LINE('',#51785,#7715);
#5749=LINE('',#51788,#7716);
#5750=LINE('',#51791,#7717);
#5751=LINE('',#51794,#7718);
#5752=LINE('',#51798,#7719);
#5753=LINE('',#51803,#7720);
#5754=LINE('',#51818,#7721);
#5755=LINE('',#51820,#7722);
#5756=LINE('',#51822,#7723);
#5757=LINE('',#51825,#7724);
#5758=LINE('',#51827,#7725);
#5759=LINE('',#51829,#7726);
#5760=LINE('',#51831,#7727);
#5761=LINE('',#51832,#7728);
#5762=LINE('',#51834,#7729);
#5763=LINE('',#51835,#7730);
#5764=LINE('',#51842,#7731);
#5765=LINE('',#51884,#7732);
#5766=LINE('',#51885,#7733);
#5767=LINE('',#51907,#7734);
#5768=LINE('',#51911,#7735);
#5769=LINE('',#51915,#7736);
#5770=LINE('',#51918,#7737);
#5771=LINE('',#51923,#7738);
#5772=LINE('',#51927,#7739);
#5773=LINE('',#51931,#7740);
#5774=LINE('',#51934,#7741);
#5775=LINE('',#51937,#7742);
#5776=LINE('',#51943,#7743);
#5777=LINE('',#51951,#7744);
#5778=LINE('',#51957,#7745);
#5779=LINE('',#51961,#7746);
#5780=LINE('',#51967,#7747);
#5781=LINE('',#51973,#7748);
#5782=LINE('',#51979,#7749);
#5783=LINE('',#51986,#7750);
#5784=LINE('',#51990,#7751);
#5785=LINE('',#51994,#7752);
#5786=LINE('',#51997,#7753);
#5787=LINE('',#51999,#7754);
#5788=LINE('',#52000,#7755);
#5789=LINE('',#52002,#7756);
#5790=LINE('',#52004,#7757);
#5791=LINE('',#52006,#7758);
#5792=LINE('',#52008,#7759);
#5793=LINE('',#52010,#7760);
#5794=LINE('',#52012,#7761);
#5795=LINE('',#52016,#7762);
#5796=LINE('',#52019,#7763);
#5797=LINE('',#52022,#7764);
#5798=LINE('',#52023,#7765);
#5799=LINE('',#52026,#7766);
#5800=LINE('',#52030,#7767);
#5801=LINE('',#52032,#7768);
#5802=LINE('',#52033,#7769);
#5803=LINE('',#52036,#7770);
#5804=LINE('',#52040,#7771);
#5805=LINE('',#52044,#7772);
#5806=LINE('',#52045,#7773);
#5807=LINE('',#52048,#7774);
#5808=LINE('',#52052,#7775);
#5809=LINE('',#52053,#7776);
#5810=LINE('',#52064,#7777);
#5811=LINE('',#52070,#7778);
#5812=LINE('',#52073,#7779);
#5813=LINE('',#52074,#7780);
#5814=LINE('',#52076,#7781);
#5815=LINE('',#52078,#7782);
#5816=LINE('',#52080,#7783);
#5817=LINE('',#52082,#7784);
#5818=LINE('',#52086,#7785);
#5819=LINE('',#52088,#7786);
#5820=LINE('',#52089,#7787);
#5821=LINE('',#52092,#7788);
#5822=LINE('',#52096,#7789);
#5823=LINE('',#52100,#7790);
#5824=LINE('',#52101,#7791);
#5825=LINE('',#52105,#7792);
#5826=LINE('',#52111,#7793);
#5827=LINE('',#52114,#7794);
#5828=LINE('',#52117,#7795);
#5829=LINE('',#52118,#7796);
#5830=LINE('',#52121,#7797);
#5831=LINE('',#52125,#7798);
#5832=LINE('',#52144,#7799);
#5833=LINE('',#52145,#7800);
#5834=LINE('',#52148,#7801);
#5835=LINE('',#52151,#7802);
#5836=LINE('',#52154,#7803);
#5837=LINE('',#52155,#7804);
#5838=LINE('',#52158,#7805);
#5839=LINE('',#52162,#7806);
#5840=LINE('',#52163,#7807);
#5841=LINE('',#52166,#7808);
#5842=LINE('',#52169,#7809);
#5843=LINE('',#52172,#7810);
#5844=LINE('',#52192,#7811);
#5845=LINE('',#52200,#7812);
#5846=LINE('',#52202,#7813);
#5847=LINE('',#52204,#7814);
#5848=LINE('',#52206,#7815);
#5849=LINE('',#52208,#7816);
#5850=LINE('',#52209,#7817);
#5851=LINE('',#52214,#7818);
#5852=LINE('',#52218,#7819);
#5853=LINE('',#52220,#7820);
#5854=LINE('',#52222,#7821);
#5855=LINE('',#52224,#7822);
#5856=LINE('',#52226,#7823);
#5857=LINE('',#52227,#7824);
#5858=LINE('',#52229,#7825);
#5859=LINE('',#52230,#7826);
#5860=LINE('',#52232,#7827);
#5861=LINE('',#52234,#7828);
#5862=LINE('',#52236,#7829);
#5863=LINE('',#52238,#7830);
#5864=LINE('',#52255,#7831);
#5865=LINE('',#52257,#7832);
#5866=LINE('',#52259,#7833);
#5867=LINE('',#52264,#7834);
#5868=LINE('',#52268,#7835);
#5869=LINE('',#52289,#7836);
#5870=LINE('',#52313,#7837);
#5871=LINE('',#52314,#7838);
#5872=LINE('',#52317,#7839);
#5873=LINE('',#52320,#7840);
#5874=LINE('',#52323,#7841);
#5875=LINE('',#52326,#7842);
#5876=LINE('',#52329,#7843);
#5877=LINE('',#52333,#7844);
#5878=LINE('',#52338,#7845);
#5879=LINE('',#52353,#7846);
#5880=LINE('',#52357,#7847);
#5881=LINE('',#52358,#7848);
#5882=LINE('',#52360,#7849);
#5883=LINE('',#52362,#7850);
#5884=LINE('',#52364,#7851);
#5885=LINE('',#52367,#7852);
#5886=LINE('',#52380,#7853);
#5887=LINE('',#52382,#7854);
#5888=LINE('',#52394,#7855);
#5889=LINE('',#52397,#7856);
#5890=LINE('',#52398,#7857);
#5891=LINE('',#52401,#7858);
#5892=LINE('',#52402,#7859);
#5893=LINE('',#52406,#7860);
#5894=LINE('',#52411,#7861);
#5895=LINE('',#52414,#7862);
#5896=LINE('',#52416,#7863);
#5897=LINE('',#52419,#7864);
#5898=LINE('',#52461,#7865);
#5899=LINE('',#52462,#7866);
#5900=LINE('',#52484,#7867);
#5901=LINE('',#52488,#7868);
#5902=LINE('',#52492,#7869);
#5903=LINE('',#52495,#7870);
#5904=LINE('',#52500,#7871);
#5905=LINE('',#52504,#7872);
#5906=LINE('',#52508,#7873);
#5907=LINE('',#52511,#7874);
#5908=LINE('',#52514,#7875);
#5909=LINE('',#52520,#7876);
#5910=LINE('',#52528,#7877);
#5911=LINE('',#52534,#7878);
#5912=LINE('',#52538,#7879);
#5913=LINE('',#52544,#7880);
#5914=LINE('',#52550,#7881);
#5915=LINE('',#52556,#7882);
#5916=LINE('',#52563,#7883);
#5917=LINE('',#52567,#7884);
#5918=LINE('',#52571,#7885);
#5919=LINE('',#52574,#7886);
#5920=LINE('',#52576,#7887);
#5921=LINE('',#52577,#7888);
#5922=LINE('',#52579,#7889);
#5923=LINE('',#52581,#7890);
#5924=LINE('',#52583,#7891);
#5925=LINE('',#52585,#7892);
#5926=LINE('',#52587,#7893);
#5927=LINE('',#52589,#7894);
#5928=LINE('',#52593,#7895);
#5929=LINE('',#52596,#7896);
#5930=LINE('',#52599,#7897);
#5931=LINE('',#52600,#7898);
#5932=LINE('',#52603,#7899);
#5933=LINE('',#52607,#7900);
#5934=LINE('',#52609,#7901);
#5935=LINE('',#52610,#7902);
#5936=LINE('',#52613,#7903);
#5937=LINE('',#52617,#7904);
#5938=LINE('',#52621,#7905);
#5939=LINE('',#52622,#7906);
#5940=LINE('',#52625,#7907);
#5941=LINE('',#52629,#7908);
#5942=LINE('',#52630,#7909);
#5943=LINE('',#52641,#7910);
#5944=LINE('',#52647,#7911);
#5945=LINE('',#52650,#7912);
#5946=LINE('',#52651,#7913);
#5947=LINE('',#52653,#7914);
#5948=LINE('',#52655,#7915);
#5949=LINE('',#52657,#7916);
#5950=LINE('',#52659,#7917);
#5951=LINE('',#52663,#7918);
#5952=LINE('',#52665,#7919);
#5953=LINE('',#52666,#7920);
#5954=LINE('',#52669,#7921);
#5955=LINE('',#52673,#7922);
#5956=LINE('',#52677,#7923);
#5957=LINE('',#52678,#7924);
#5958=LINE('',#52682,#7925);
#5959=LINE('',#52688,#7926);
#5960=LINE('',#52691,#7927);
#5961=LINE('',#52694,#7928);
#5962=LINE('',#52695,#7929);
#5963=LINE('',#52698,#7930);
#5964=LINE('',#52702,#7931);
#5965=LINE('',#52721,#7932);
#5966=LINE('',#52722,#7933);
#5967=LINE('',#52725,#7934);
#5968=LINE('',#52728,#7935);
#5969=LINE('',#52731,#7936);
#5970=LINE('',#52732,#7937);
#5971=LINE('',#52735,#7938);
#5972=LINE('',#52739,#7939);
#5973=LINE('',#52740,#7940);
#5974=LINE('',#52743,#7941);
#5975=LINE('',#52746,#7942);
#5976=LINE('',#52749,#7943);
#5977=LINE('',#52769,#7944);
#5978=LINE('',#52783,#7945);
#5979=LINE('',#52789,#7946);
#5980=LINE('',#52795,#7947);
#5981=LINE('',#52801,#7948);
#5982=LINE('',#52807,#7949);
#5983=LINE('',#52813,#7950);
#5984=LINE('',#52819,#7951);
#5985=LINE('',#52824,#7952);
#5986=LINE('',#52828,#7953);
#5987=LINE('',#52830,#7954);
#5988=LINE('',#52832,#7955);
#5989=LINE('',#52837,#7956);
#5990=LINE('',#52838,#7957);
#5991=LINE('',#52839,#7958);
#5992=LINE('',#52843,#7959);
#5993=LINE('',#52848,#7960);
#5994=LINE('',#52849,#7961);
#5995=LINE('',#52851,#7962);
#5996=LINE('',#52852,#7963);
#5997=LINE('',#52854,#7964);
#5998=LINE('',#52856,#7965);
#5999=LINE('',#52864,#7966);
#6000=LINE('',#52870,#7967);
#6001=LINE('',#52876,#7968);
#6002=LINE('',#52882,#7969);
#6003=LINE('',#52888,#7970);
#6004=LINE('',#52894,#7971);
#6005=LINE('',#52899,#7972);
#6006=LINE('',#52901,#7973);
#6007=LINE('',#52903,#7974);
#6008=LINE('',#52904,#7975);
#6009=LINE('',#52907,#7976);
#6010=LINE('',#52909,#7977);
#6011=LINE('',#52910,#7978);
#6012=LINE('',#52913,#7979);
#6013=LINE('',#52915,#7980);
#6014=LINE('',#52916,#7981);
#6015=LINE('',#52918,#7982);
#6016=LINE('',#52919,#7983);
#6017=LINE('',#52929,#7984);
#6018=LINE('',#52935,#7985);
#6019=LINE('',#52941,#7986);
#6020=LINE('',#52947,#7987);
#6021=LINE('',#52953,#7988);
#6022=LINE('',#52959,#7989);
#6023=LINE('',#52964,#7990);
#6024=LINE('',#52966,#7991);
#6025=LINE('',#52968,#7992);
#6026=LINE('',#52969,#7993);
#6027=LINE('',#52972,#7994);
#6028=LINE('',#52974,#7995);
#6029=LINE('',#52975,#7996);
#6030=LINE('',#52978,#7997);
#6031=LINE('',#52980,#7998);
#6032=LINE('',#52981,#7999);
#6033=LINE('',#52983,#8000);
#6034=LINE('',#52984,#8001);
#6035=LINE('',#52991,#8002);
#6036=LINE('',#52993,#8003);
#6037=LINE('',#52995,#8004);
#6038=LINE('',#52996,#8005);
#6039=LINE('',#52999,#8006);
#6040=LINE('',#53001,#8007);
#6041=LINE('',#53002,#8008);
#6042=LINE('',#53005,#8009);
#6043=LINE('',#53007,#8010);
#6044=LINE('',#53008,#8011);
#6045=LINE('',#53011,#8012);
#6046=LINE('',#53013,#8013);
#6047=LINE('',#53014,#8014);
#6048=LINE('',#53016,#8015);
#6049=LINE('',#53017,#8016);
#6050=LINE('',#53023,#8017);
#6051=LINE('',#53025,#8018);
#6052=LINE('',#53027,#8019);
#6053=LINE('',#53028,#8020);
#6054=LINE('',#53031,#8021);
#6055=LINE('',#53033,#8022);
#6056=LINE('',#53034,#8023);
#6057=LINE('',#53037,#8024);
#6058=LINE('',#53039,#8025);
#6059=LINE('',#53040,#8026);
#6060=LINE('',#53043,#8027);
#6061=LINE('',#53045,#8028);
#6062=LINE('',#53046,#8029);
#6063=LINE('',#53048,#8030);
#6064=LINE('',#53049,#8031);
#6065=LINE('',#53057,#8032);
#6066=LINE('',#53060,#8033);
#6067=LINE('',#53065,#8034);
#6068=LINE('',#53071,#8035);
#6069=LINE('',#53077,#8036);
#6070=LINE('',#53083,#8037);
#6071=LINE('',#53089,#8038);
#6072=LINE('',#53095,#8039);
#6073=LINE('',#53101,#8040);
#6074=LINE('',#53107,#8041);
#6075=LINE('',#53113,#8042);
#6076=LINE('',#53119,#8043);
#6077=LINE('',#53125,#8044);
#6078=LINE('',#53131,#8045);
#6079=LINE('',#53137,#8046);
#6080=LINE('',#53143,#8047);
#6081=LINE('',#53149,#8048);
#6082=LINE('',#53155,#8049);
#6083=LINE('',#53161,#8050);
#6084=LINE('',#53167,#8051);
#6085=LINE('',#53173,#8052);
#6086=LINE('',#53179,#8053);
#6087=LINE('',#53185,#8054);
#6088=LINE('',#53191,#8055);
#6089=LINE('',#53197,#8056);
#6090=LINE('',#53203,#8057);
#6091=LINE('',#53209,#8058);
#6092=LINE('',#53215,#8059);
#6093=LINE('',#53221,#8060);
#6094=LINE('',#53227,#8061);
#6095=LINE('',#53233,#8062);
#6096=LINE('',#53239,#8063);
#6097=LINE('',#53245,#8064);
#6098=LINE('',#53251,#8065);
#6099=LINE('',#53257,#8066);
#6100=LINE('',#53263,#8067);
#6101=LINE('',#53269,#8068);
#6102=LINE('',#53275,#8069);
#6103=LINE('',#53281,#8070);
#6104=LINE('',#53287,#8071);
#6105=LINE('',#53293,#8072);
#6106=LINE('',#53299,#8073);
#6107=LINE('',#53305,#8074);
#6108=LINE('',#53311,#8075);
#6109=LINE('',#53317,#8076);
#6110=LINE('',#53323,#8077);
#6111=LINE('',#53329,#8078);
#6112=LINE('',#53335,#8079);
#6113=LINE('',#53341,#8080);
#6114=LINE('',#53347,#8081);
#6115=LINE('',#53352,#8082);
#6116=LINE('',#53354,#8083);
#6117=LINE('',#53356,#8084);
#6118=LINE('',#53358,#8085);
#6119=LINE('',#53360,#8086);
#6120=LINE('',#53362,#8087);
#6121=LINE('',#53364,#8088);
#6122=LINE('',#53365,#8089);
#6123=LINE('',#53369,#8090);
#6124=LINE('',#53371,#8091);
#6125=LINE('',#53373,#8092);
#6126=LINE('',#53374,#8093);
#6127=LINE('',#53378,#8094);
#6128=LINE('',#53380,#8095);
#6129=LINE('',#53382,#8096);
#6130=LINE('',#53383,#8097);
#6131=LINE('',#53387,#8098);
#6132=LINE('',#53389,#8099);
#6133=LINE('',#53391,#8100);
#6134=LINE('',#53392,#8101);
#6135=LINE('',#53394,#8102);
#6136=LINE('',#53395,#8103);
#6137=LINE('',#53396,#8104);
#6138=LINE('',#53398,#8105);
#6139=LINE('',#53400,#8106);
#6140=LINE('',#53403,#8107);
#6141=LINE('',#53404,#8108);
#6142=LINE('',#53405,#8109);
#6143=LINE('',#53407,#8110);
#6144=LINE('',#53410,#8111);
#6145=LINE('',#53414,#8112);
#6146=LINE('',#53416,#8113);
#6147=LINE('',#53418,#8114);
#6148=LINE('',#53420,#8115);
#6149=LINE('',#53422,#8116);
#6150=LINE('',#53424,#8117);
#6151=LINE('',#53426,#8118);
#6152=LINE('',#53427,#8119);
#6153=LINE('',#53429,#8120);
#6154=LINE('',#53430,#8121);
#6155=LINE('',#53432,#8122);
#6156=LINE('',#53433,#8123);
#6157=LINE('',#53435,#8124);
#6158=LINE('',#53436,#8125);
#6159=LINE('',#53438,#8126);
#6160=LINE('',#53439,#8127);
#6161=LINE('',#53460,#8128);
#6162=LINE('',#53462,#8129);
#6163=LINE('',#53474,#8130);
#6164=LINE('',#53489,#8131);
#6165=LINE('',#53502,#8132);
#6166=LINE('',#53517,#8133);
#6167=LINE('',#53530,#8134);
#6168=LINE('',#53545,#8135);
#6169=LINE('',#53558,#8136);
#6170=LINE('',#53573,#8137);
#6171=LINE('',#53586,#8138);
#6172=LINE('',#53601,#8139);
#6173=LINE('',#53614,#8140);
#6174=LINE('',#53629,#8141);
#6175=LINE('',#53642,#8142);
#6176=LINE('',#53657,#8143);
#6177=LINE('',#53670,#8144);
#6178=LINE('',#53685,#8145);
#6179=LINE('',#53696,#8146);
#6180=LINE('',#53698,#8147);
#6181=LINE('',#53699,#8148);
#6182=LINE('',#53701,#8149);
#6183=LINE('',#53702,#8150);
#6184=LINE('',#53704,#8151);
#6185=LINE('',#53706,#8152);
#6186=LINE('',#53707,#8153);
#6187=LINE('',#53708,#8154);
#6188=LINE('',#53709,#8155);
#6189=LINE('',#53710,#8156);
#6190=LINE('',#53711,#8157);
#6191=LINE('',#53712,#8158);
#6192=LINE('',#53714,#8159);
#6193=LINE('',#53716,#8160);
#6194=LINE('',#53718,#8161);
#6195=LINE('',#53719,#8162);
#6196=LINE('',#53722,#8163);
#6197=LINE('',#53724,#8164);
#6198=LINE('',#53726,#8165);
#6199=LINE('',#53728,#8166);
#6200=LINE('',#53729,#8167);
#6201=LINE('',#53730,#8168);
#6202=LINE('',#53731,#8169);
#6203=LINE('',#53732,#8170);
#6204=LINE('',#53733,#8171);
#6205=LINE('',#53734,#8172);
#6206=LINE('',#53735,#8173);
#6207=LINE('',#53738,#8174);
#6208=LINE('',#53739,#8175);
#6209=LINE('',#53743,#8176);
#6210=LINE('',#53744,#8177);
#6211=LINE('',#53748,#8178);
#6212=LINE('',#53750,#8179);
#6213=LINE('',#53753,#8180);
#6214=LINE('',#53754,#8181);
#6215=LINE('',#53758,#8182);
#6216=LINE('',#53759,#8183);
#6217=LINE('',#53763,#8184);
#6218=LINE('',#53764,#8185);
#6219=LINE('',#53769,#8186);
#6220=LINE('',#53771,#8187);
#6221=LINE('',#53772,#8188);
#6222=LINE('',#53774,#8189);
#6223=LINE('',#53777,#8190);
#6224=LINE('',#53779,#8191);
#6225=LINE('',#53783,#8192);
#6226=LINE('',#53787,#8193);
#6227=LINE('',#53791,#8194);
#6228=LINE('',#53799,#8195);
#6229=LINE('',#53803,#8196);
#6230=LINE('',#53807,#8197);
#6231=LINE('',#53815,#8198);
#6232=LINE('',#53817,#8199);
#6233=LINE('',#53819,#8200);
#6234=LINE('',#53827,#8201);
#6235=LINE('',#53831,#8202);
#6236=LINE('',#53835,#8203);
#6237=LINE('',#53843,#8204);
#6238=LINE('',#53847,#8205);
#6239=LINE('',#53851,#8206);
#6240=LINE('',#53855,#8207);
#6241=LINE('',#53856,#8208);
#6242=LINE('',#53858,#8209);
#6243=LINE('',#53859,#8210);
#6244=LINE('',#53861,#8211);
#6245=LINE('',#53863,#8212);
#6246=LINE('',#53865,#8213);
#6247=LINE('',#53869,#8214);
#6248=LINE('',#53873,#8215);
#6249=LINE('',#53877,#8216);
#6250=LINE('',#53885,#8217);
#6251=LINE('',#53889,#8218);
#6252=LINE('',#53893,#8219);
#6253=LINE('',#53901,#8220);
#6254=LINE('',#53903,#8221);
#6255=LINE('',#53905,#8222);
#6256=LINE('',#53913,#8223);
#6257=LINE('',#53917,#8224);
#6258=LINE('',#53921,#8225);
#6259=LINE('',#53929,#8226);
#6260=LINE('',#53933,#8227);
#6261=LINE('',#53937,#8228);
#6262=LINE('',#53941,#8229);
#6263=LINE('',#53942,#8230);
#6264=LINE('',#53944,#8231);
#6265=LINE('',#53945,#8232);
#6266=LINE('',#53947,#8233);
#6267=LINE('',#53948,#8234);
#6268=LINE('',#53950,#8235);
#6269=LINE('',#53951,#8236);
#6270=LINE('',#53953,#8237);
#6271=LINE('',#53954,#8238);
#6272=LINE('',#53956,#8239);
#6273=LINE('',#53957,#8240);
#6274=LINE('',#53959,#8241);
#6275=LINE('',#53960,#8242);
#6276=LINE('',#53962,#8243);
#6277=LINE('',#53964,#8244);
#6278=LINE('',#53966,#8245);
#6279=LINE('',#53968,#8246);
#6280=LINE('',#53969,#8247);
#6281=LINE('',#53971,#8248);
#6282=LINE('',#53972,#8249);
#6283=LINE('',#53974,#8250);
#6284=LINE('',#53975,#8251);
#6285=LINE('',#53977,#8252);
#6286=LINE('',#53978,#8253);
#6287=LINE('',#53980,#8254);
#6288=LINE('',#53982,#8255);
#6289=LINE('',#53983,#8256);
#6290=LINE('',#53985,#8257);
#6291=LINE('',#53986,#8258);
#6292=LINE('',#53997,#8259);
#6293=LINE('',#53998,#8260);
#6294=LINE('',#54000,#8261);
#6295=LINE('',#54001,#8262);
#6296=LINE('',#54003,#8263);
#6297=LINE('',#54004,#8264);
#6298=LINE('',#54006,#8265);
#6299=LINE('',#54007,#8266);
#6300=LINE('',#54010,#8267);
#6301=LINE('',#54011,#8268);
#6302=LINE('',#54013,#8269);
#6303=LINE('',#54014,#8270);
#6304=LINE('',#54026,#8271);
#6305=LINE('',#54041,#8272);
#6306=LINE('',#54047,#8273);
#6307=LINE('',#54053,#8274);
#6308=LINE('',#54057,#8275);
#6309=LINE('',#54060,#8276);
#6310=LINE('',#54065,#8277);
#6311=LINE('',#54071,#8278);
#6312=LINE('',#54077,#8279);
#6313=LINE('',#54083,#8280);
#6314=LINE('',#54089,#8281);
#6315=LINE('',#54095,#8282);
#6316=LINE('',#54101,#8283);
#6317=LINE('',#54107,#8284);
#6318=LINE('',#54111,#8285);
#6319=LINE('',#54114,#8286);
#6320=LINE('',#54117,#8287);
#6321=LINE('',#54120,#8288);
#6322=LINE('',#54125,#8289);
#6323=LINE('',#54127,#8290);
#6324=LINE('',#54131,#8291);
#6325=LINE('',#54236,#8292);
#6326=LINE('',#54241,#8293);
#6327=LINE('',#54248,#8294);
#6328=LINE('',#54250,#8295);
#6329=LINE('',#54251,#8296);
#6330=LINE('',#54256,#8297);
#6331=LINE('',#54259,#8298);
#6332=LINE('',#54265,#8299);
#6333=LINE('',#54268,#8300);
#6334=LINE('',#54273,#8301);
#6335=LINE('',#54275,#8302);
#6336=LINE('',#54276,#8303);
#6337=LINE('',#54280,#8304);
#6338=LINE('',#54282,#8305);
#6339=LINE('',#54284,#8306);
#6340=LINE('',#54285,#8307);
#6341=LINE('',#54289,#8308);
#6342=LINE('',#54291,#8309);
#6343=LINE('',#54293,#8310);
#6344=LINE('',#54294,#8311);
#6345=LINE('',#54298,#8312);
#6346=LINE('',#54300,#8313);
#6347=LINE('',#54302,#8314);
#6348=LINE('',#54303,#8315);
#6349=LINE('',#54307,#8316);
#6350=LINE('',#54309,#8317);
#6351=LINE('',#54311,#8318);
#6352=LINE('',#54312,#8319);
#6353=LINE('',#54316,#8320);
#6354=LINE('',#54318,#8321);
#6355=LINE('',#54320,#8322);
#6356=LINE('',#54321,#8323);
#6357=LINE('',#54325,#8324);
#6358=LINE('',#54327,#8325);
#6359=LINE('',#54329,#8326);
#6360=LINE('',#54330,#8327);
#6361=LINE('',#54334,#8328);
#6362=LINE('',#54336,#8329);
#6363=LINE('',#54338,#8330);
#6364=LINE('',#54339,#8331);
#6365=LINE('',#54343,#8332);
#6366=LINE('',#54345,#8333);
#6367=LINE('',#54347,#8334);
#6368=LINE('',#54348,#8335);
#6369=LINE('',#54352,#8336);
#6370=LINE('',#54354,#8337);
#6371=LINE('',#54356,#8338);
#6372=LINE('',#54357,#8339);
#6373=LINE('',#54360,#8340);
#6374=LINE('',#54362,#8341);
#6375=LINE('',#54363,#8342);
#6376=LINE('',#54367,#8343);
#6377=LINE('',#54369,#8344);
#6378=LINE('',#54371,#8345);
#6379=LINE('',#54372,#8346);
#6380=LINE('',#54375,#8347);
#6381=LINE('',#54377,#8348);
#6382=LINE('',#54378,#8349);
#6383=LINE('',#54382,#8350);
#6384=LINE('',#54384,#8351);
#6385=LINE('',#54386,#8352);
#6386=LINE('',#54387,#8353);
#6387=LINE('',#54391,#8354);
#6388=LINE('',#54393,#8355);
#6389=LINE('',#54395,#8356);
#6390=LINE('',#54396,#8357);
#6391=LINE('',#54400,#8358);
#6392=LINE('',#54402,#8359);
#6393=LINE('',#54404,#8360);
#6394=LINE('',#54405,#8361);
#6395=LINE('',#54409,#8362);
#6396=LINE('',#54411,#8363);
#6397=LINE('',#54413,#8364);
#6398=LINE('',#54414,#8365);
#6399=LINE('',#54416,#8366);
#6400=LINE('',#54417,#8367);
#6401=LINE('',#54423,#8368);
#6402=LINE('',#54426,#8369);
#6403=LINE('',#54432,#8370);
#6404=LINE('',#54435,#8371);
#6405=LINE('',#54441,#8372);
#6406=LINE('',#54444,#8373);
#6407=LINE('',#54450,#8374);
#6408=LINE('',#54453,#8375);
#6409=LINE('',#54506,#8376);
#6410=LINE('',#54508,#8377);
#6411=LINE('',#54510,#8378);
#6412=LINE('',#54511,#8379);
#6413=LINE('',#54514,#8380);
#6414=LINE('',#54516,#8381);
#6415=LINE('',#54517,#8382);
#6416=LINE('',#54519,#8383);
#6417=LINE('',#54521,#8384);
#6418=LINE('',#54522,#8385);
#6419=LINE('',#54525,#8386);
#6420=LINE('',#54526,#8387);
#6421=LINE('',#54529,#8388);
#6422=LINE('',#54530,#8389);
#6423=LINE('',#54532,#8390);
#6424=LINE('',#54535,#8391);
#6425=LINE('',#54536,#8392);
#6426=LINE('',#54539,#8393);
#6427=LINE('',#54540,#8394);
#6428=LINE('',#54542,#8395);
#6429=LINE('',#54545,#8396);
#6430=LINE('',#54547,#8397);
#6431=LINE('',#54548,#8398);
#6432=LINE('',#54551,#8399);
#6433=LINE('',#54552,#8400);
#6434=LINE('',#54555,#8401);
#6435=LINE('',#54556,#8402);
#6436=LINE('',#54559,#8403);
#6437=LINE('',#54560,#8404);
#6438=LINE('',#54563,#8405);
#6439=LINE('',#54564,#8406);
#6440=LINE('',#54566,#8407);
#6441=LINE('',#54571,#8408);
#6442=LINE('',#54575,#8409);
#6443=LINE('',#54579,#8410);
#6444=LINE('',#54587,#8411);
#6445=LINE('',#54591,#8412);
#6446=LINE('',#54595,#8413);
#6447=LINE('',#54603,#8414);
#6448=LINE('',#54605,#8415);
#6449=LINE('',#54607,#8416);
#6450=LINE('',#54615,#8417);
#6451=LINE('',#54619,#8418);
#6452=LINE('',#54623,#8419);
#6453=LINE('',#54631,#8420);
#6454=LINE('',#54635,#8421);
#6455=LINE('',#54639,#8422);
#6456=LINE('',#54641,#8423);
#6457=LINE('',#54643,#8424);
#6458=LINE('',#54645,#8425);
#6459=LINE('',#54647,#8426);
#6460=LINE('',#54649,#8427);
#6461=LINE('',#54651,#8428);
#6462=LINE('',#54653,#8429);
#6463=LINE('',#54655,#8430);
#6464=LINE('',#54656,#8431);
#6465=LINE('',#54660,#8432);
#6466=LINE('',#54661,#8433);
#6467=LINE('',#54662,#8434);
#6468=LINE('',#54666,#8435);
#6469=LINE('',#54669,#8436);
#6470=LINE('',#54670,#8437);
#6471=LINE('',#54674,#8438);
#6472=LINE('',#54677,#8439);
#6473=LINE('',#54678,#8440);
#6474=LINE('',#54682,#8441);
#6475=LINE('',#54686,#8442);
#6476=LINE('',#54690,#8443);
#6477=LINE('',#54693,#8444);
#6478=LINE('',#54694,#8445);
#6479=LINE('',#54698,#8446);
#6480=LINE('',#54701,#8447);
#6481=LINE('',#54702,#8448);
#6482=LINE('',#54706,#8449);
#6483=LINE('',#54709,#8450);
#6484=LINE('',#54710,#8451);
#6485=LINE('',#54714,#8452);
#6486=LINE('',#54718,#8453);
#6487=LINE('',#54722,#8454);
#6488=LINE('',#54725,#8455);
#6489=LINE('',#54726,#8456);
#6490=LINE('',#54729,#8457);
#6491=LINE('',#54730,#8458);
#6492=LINE('',#54733,#8459);
#6493=LINE('',#54734,#8460);
#6494=LINE('',#54738,#8461);
#6495=LINE('',#54742,#8462);
#6496=LINE('',#54746,#8463);
#6497=LINE('',#54749,#8464);
#6498=LINE('',#54750,#8465);
#6499=LINE('',#54754,#8466);
#6500=LINE('',#54757,#8467);
#6501=LINE('',#54758,#8468);
#6502=LINE('',#54762,#8469);
#6503=LINE('',#54765,#8470);
#6504=LINE('',#54766,#8471);
#6505=LINE('',#54770,#8472);
#6506=LINE('',#54774,#8473);
#6507=LINE('',#54778,#8474);
#6508=LINE('',#54781,#8475);
#6509=LINE('',#54782,#8476);
#6510=LINE('',#54786,#8477);
#6511=LINE('',#54789,#8478);
#6512=LINE('',#54790,#8479);
#6513=LINE('',#54794,#8480);
#6514=LINE('',#54797,#8481);
#6515=LINE('',#54798,#8482);
#6516=LINE('',#54801,#8483);
#6517=LINE('',#54802,#8484);
#6518=LINE('',#54805,#8485);
#6519=LINE('',#54806,#8486);
#6520=LINE('',#54809,#8487);
#6521=LINE('',#54810,#8488);
#6522=LINE('',#54813,#8489);
#6523=LINE('',#54814,#8490);
#6524=LINE('',#54817,#8491);
#6525=LINE('',#54818,#8492);
#6526=LINE('',#54821,#8493);
#6527=LINE('',#54822,#8494);
#6528=LINE('',#54825,#8495);
#6529=LINE('',#54826,#8496);
#6530=LINE('',#54829,#8497);
#6531=LINE('',#54830,#8498);
#6532=LINE('',#54832,#8499);
#6533=LINE('',#54836,#8500);
#6534=LINE('',#54839,#8501);
#6535=LINE('',#54843,#8502);
#6536=LINE('',#54845,#8503);
#6537=LINE('',#54849,#8504);
#6538=LINE('',#54851,#8505);
#6539=LINE('',#54853,#8506);
#6540=LINE('',#54855,#8507);
#6541=LINE('',#54857,#8508);
#6542=LINE('',#54859,#8509);
#6543=LINE('',#54861,#8510);
#6544=LINE('',#54865,#8511);
#6545=LINE('',#54869,#8512);
#6546=LINE('',#54877,#8513);
#6547=LINE('',#54881,#8514);
#6548=LINE('',#54885,#8515);
#6549=LINE('',#54893,#8516);
#6550=LINE('',#54895,#8517);
#6551=LINE('',#54897,#8518);
#6552=LINE('',#54905,#8519);
#6553=LINE('',#54909,#8520);
#6554=LINE('',#54913,#8521);
#6555=LINE('',#54921,#8522);
#6556=LINE('',#54925,#8523);
#6557=LINE('',#54929,#8524);
#6558=LINE('',#54931,#8525);
#6559=LINE('',#54933,#8526);
#6560=LINE('',#54935,#8527);
#6561=LINE('',#54936,#8528);
#6562=LINE('',#54939,#8529);
#6563=LINE('',#54940,#8530);
#6564=LINE('',#54943,#8531);
#6565=LINE('',#54944,#8532);
#6566=LINE('',#54950,#8533);
#6567=LINE('',#54953,#8534);
#6568=LINE('',#54957,#8535);
#6569=LINE('',#54958,#8536);
#6570=LINE('',#54959,#8537);
#6571=LINE('',#54962,#8538);
#6572=LINE('',#54963,#8539);
#6573=LINE('',#54966,#8540);
#6574=LINE('',#54967,#8541);
#6575=LINE('',#54970,#8542);
#6576=LINE('',#54971,#8543);
#6577=LINE('',#54975,#8544);
#6578=LINE('',#54976,#8545);
#6579=LINE('',#54978,#8546);
#6580=LINE('',#54979,#8547);
#6581=LINE('',#54980,#8548);
#6582=LINE('',#54983,#8549);
#6583=LINE('',#54984,#8550);
#6584=LINE('',#54987,#8551);
#6585=LINE('',#54988,#8552);
#6586=LINE('',#54991,#8553);
#6587=LINE('',#54992,#8554);
#6588=LINE('',#54995,#8555);
#6589=LINE('',#54996,#8556);
#6590=LINE('',#54999,#8557);
#6591=LINE('',#55000,#8558);
#6592=LINE('',#55004,#8559);
#6593=LINE('',#55007,#8560);
#6594=LINE('',#55008,#8561);
#6595=LINE('',#55012,#8562);
#6596=LINE('',#55015,#8563);
#6597=LINE('',#55016,#8564);
#6598=LINE('',#55020,#8565);
#6599=LINE('',#55024,#8566);
#6600=LINE('',#55028,#8567);
#6601=LINE('',#55031,#8568);
#6602=LINE('',#55032,#8569);
#6603=LINE('',#55036,#8570);
#6604=LINE('',#55039,#8571);
#6605=LINE('',#55040,#8572);
#6606=LINE('',#55044,#8573);
#6607=LINE('',#55047,#8574);
#6608=LINE('',#55048,#8575);
#6609=LINE('',#55052,#8576);
#6610=LINE('',#55056,#8577);
#6611=LINE('',#55060,#8578);
#6612=LINE('',#55063,#8579);
#6613=LINE('',#55064,#8580);
#6614=LINE('',#55067,#8581);
#6615=LINE('',#55068,#8582);
#6616=LINE('',#55071,#8583);
#6617=LINE('',#55072,#8584);
#6618=LINE('',#55076,#8585);
#6619=LINE('',#55080,#8586);
#6620=LINE('',#55084,#8587);
#6621=LINE('',#55087,#8588);
#6622=LINE('',#55088,#8589);
#6623=LINE('',#55092,#8590);
#6624=LINE('',#55095,#8591);
#6625=LINE('',#55096,#8592);
#6626=LINE('',#55100,#8593);
#6627=LINE('',#55103,#8594);
#6628=LINE('',#55104,#8595);
#6629=LINE('',#55108,#8596);
#6630=LINE('',#55112,#8597);
#6631=LINE('',#55116,#8598);
#6632=LINE('',#55119,#8599);
#6633=LINE('',#55120,#8600);
#6634=LINE('',#55124,#8601);
#6635=LINE('',#55127,#8602);
#6636=LINE('',#55128,#8603);
#6637=LINE('',#55132,#8604);
#6638=LINE('',#55134,#8605);
#6639=LINE('',#55139,#8606);
#6640=LINE('',#55141,#8607);
#6641=LINE('',#55143,#8608);
#6642=LINE('',#55144,#8609);
#6643=LINE('',#55148,#8610);
#6644=LINE('',#55150,#8611);
#6645=LINE('',#55152,#8612);
#6646=LINE('',#55153,#8613);
#6647=LINE('',#55156,#8614);
#6648=LINE('',#55157,#8615);
#6649=LINE('',#55160,#8616);
#6650=LINE('',#55161,#8617);
#6651=LINE('',#55169,#8618);
#6652=LINE('',#55172,#8619);
#6653=LINE('',#55174,#8620);
#6654=LINE('',#55176,#8621);
#6655=LINE('',#55177,#8622);
#6656=LINE('',#55180,#8623);
#6657=LINE('',#55182,#8624);
#6658=LINE('',#55183,#8625);
#6659=LINE('',#55187,#8626);
#6660=LINE('',#55189,#8627);
#6661=LINE('',#55191,#8628);
#6662=LINE('',#55192,#8629);
#6663=LINE('',#55195,#8630);
#6664=LINE('',#55198,#8631);
#6665=LINE('',#55199,#8632);
#6666=LINE('',#55202,#8633);
#6667=LINE('',#55207,#8634);
#6668=LINE('',#55209,#8635);
#6669=LINE('',#55211,#8636);
#6670=LINE('',#55213,#8637);
#6671=LINE('',#55215,#8638);
#6672=LINE('',#55217,#8639);
#6673=LINE('',#55219,#8640);
#6674=LINE('',#55221,#8641);
#6675=LINE('',#55223,#8642);
#6676=LINE('',#55225,#8643);
#6677=LINE('',#55229,#8644);
#6678=LINE('',#55233,#8645);
#6679=LINE('',#55241,#8646);
#6680=LINE('',#55245,#8647);
#6681=LINE('',#55249,#8648);
#6682=LINE('',#55257,#8649);
#6683=LINE('',#55259,#8650);
#6684=LINE('',#55261,#8651);
#6685=LINE('',#55269,#8652);
#6686=LINE('',#55273,#8653);
#6687=LINE('',#55277,#8654);
#6688=LINE('',#55285,#8655);
#6689=LINE('',#55289,#8656);
#6690=LINE('',#55292,#8657);
#6691=LINE('',#55295,#8658);
#6692=LINE('',#55296,#8659);
#6693=LINE('',#55299,#8660);
#6694=LINE('',#55300,#8661);
#6695=LINE('',#55304,#8662);
#6696=LINE('',#55305,#8663);
#6697=LINE('',#55306,#8664);
#6698=LINE('',#55309,#8665);
#6699=LINE('',#55311,#8666);
#6700=LINE('',#55312,#8667);
#6701=LINE('',#55315,#8668);
#6702=LINE('',#55317,#8669);
#6703=LINE('',#55318,#8670);
#6704=LINE('',#55321,#8671);
#6705=LINE('',#55323,#8672);
#6706=LINE('',#55324,#8673);
#6707=LINE('',#55333,#8674);
#6708=LINE('',#55335,#8675);
#6709=LINE('',#55336,#8676);
#6710=LINE('',#55340,#8677);
#6711=LINE('',#55341,#8678);
#6712=LINE('',#55342,#8679);
#6713=LINE('',#55347,#8680);
#6714=LINE('',#55348,#8681);
#6715=LINE('',#55352,#8682);
#6716=LINE('',#55353,#8683);
#6717=LINE('',#55354,#8684);
#6718=LINE('',#55357,#8685);
#6719=LINE('',#55358,#8686);
#6720=LINE('',#55364,#8687);
#6721=LINE('',#55365,#8688);
#6722=LINE('',#55372,#8689);
#6723=LINE('',#55373,#8690);
#6724=LINE('',#55374,#8691);
#6725=LINE('',#55377,#8692);
#6726=LINE('',#55378,#8693);
#6727=LINE('',#55381,#8694);
#6728=LINE('',#55382,#8695);
#6729=LINE('',#55385,#8696);
#6730=LINE('',#55386,#8697);
#6731=LINE('',#55389,#8698);
#6732=LINE('',#55390,#8699);
#6733=LINE('',#55393,#8700);
#6734=LINE('',#55394,#8701);
#6735=LINE('',#55397,#8702);
#6736=LINE('',#55398,#8703);
#6737=LINE('',#55401,#8704);
#6738=LINE('',#55402,#8705);
#6739=LINE('',#55405,#8706);
#6740=LINE('',#55406,#8707);
#6741=LINE('',#55409,#8708);
#6742=LINE('',#55410,#8709);
#6743=LINE('',#55414,#8710);
#6744=LINE('',#55417,#8711);
#6745=LINE('',#55418,#8712);
#6746=LINE('',#55422,#8713);
#6747=LINE('',#55425,#8714);
#6748=LINE('',#55426,#8715);
#6749=LINE('',#55430,#8716);
#6750=LINE('',#55434,#8717);
#6751=LINE('',#55438,#8718);
#6752=LINE('',#55441,#8719);
#6753=LINE('',#55442,#8720);
#6754=LINE('',#55446,#8721);
#6755=LINE('',#55449,#8722);
#6756=LINE('',#55450,#8723);
#6757=LINE('',#55454,#8724);
#6758=LINE('',#55457,#8725);
#6759=LINE('',#55458,#8726);
#6760=LINE('',#55462,#8727);
#6761=LINE('',#55466,#8728);
#6762=LINE('',#55470,#8729);
#6763=LINE('',#55473,#8730);
#6764=LINE('',#55474,#8731);
#6765=LINE('',#55477,#8732);
#6766=LINE('',#55478,#8733);
#6767=LINE('',#55481,#8734);
#6768=LINE('',#55482,#8735);
#6769=LINE('',#55486,#8736);
#6770=LINE('',#55490,#8737);
#6771=LINE('',#55494,#8738);
#6772=LINE('',#55497,#8739);
#6773=LINE('',#55498,#8740);
#6774=LINE('',#55502,#8741);
#6775=LINE('',#55505,#8742);
#6776=LINE('',#55506,#8743);
#6777=LINE('',#55510,#8744);
#6778=LINE('',#55513,#8745);
#6779=LINE('',#55514,#8746);
#6780=LINE('',#55518,#8747);
#6781=LINE('',#55522,#8748);
#6782=LINE('',#55526,#8749);
#6783=LINE('',#55529,#8750);
#6784=LINE('',#55530,#8751);
#6785=LINE('',#55534,#8752);
#6786=LINE('',#55537,#8753);
#6787=LINE('',#55538,#8754);
#6788=LINE('',#55542,#8755);
#6789=LINE('',#55544,#8756);
#6790=LINE('',#55548,#8757);
#6791=LINE('',#55550,#8758);
#6792=LINE('',#55552,#8759);
#6793=LINE('',#55553,#8760);
#6794=LINE('',#55556,#8761);
#6795=LINE('',#55558,#8762);
#6796=LINE('',#55559,#8763);
#6797=LINE('',#55562,#8764);
#6798=LINE('',#55564,#8765);
#6799=LINE('',#55565,#8766);
#6800=LINE('',#55568,#8767);
#6801=LINE('',#55570,#8768);
#6802=LINE('',#55571,#8769);
#6803=LINE('',#55574,#8770);
#6804=LINE('',#55576,#8771);
#6805=LINE('',#55577,#8772);
#6806=LINE('',#55581,#8773);
#6807=LINE('',#55583,#8774);
#6808=LINE('',#55585,#8775);
#6809=LINE('',#55586,#8776);
#6810=LINE('',#55589,#8777);
#6811=LINE('',#55591,#8778);
#6812=LINE('',#55592,#8779);
#6813=LINE('',#55595,#8780);
#6814=LINE('',#55597,#8781);
#6815=LINE('',#55598,#8782);
#6816=LINE('',#55600,#8783);
#6817=LINE('',#55601,#8784);
#6818=LINE('',#55604,#8785);
#6819=LINE('',#55606,#8786);
#6820=LINE('',#55608,#8787);
#6821=LINE('',#55609,#8788);
#6822=LINE('',#55612,#8789);
#6823=LINE('',#55614,#8790);
#6824=LINE('',#55615,#8791);
#6825=LINE('',#55619,#8792);
#6826=LINE('',#55620,#8793);
#6827=LINE('',#55621,#8794);
#6828=LINE('',#55625,#8795);
#6829=LINE('',#55626,#8796);
#6830=LINE('',#55627,#8797);
#6831=LINE('',#55631,#8798);
#6832=LINE('',#55632,#8799);
#6833=LINE('',#55633,#8800);
#6834=LINE('',#55637,#8801);
#6835=LINE('',#55638,#8802);
#6836=LINE('',#55639,#8803);
#6837=LINE('',#55642,#8804);
#6838=LINE('',#55644,#8805);
#6839=LINE('',#55645,#8806);
#6840=LINE('',#55649,#8807);
#6841=LINE('',#55650,#8808);
#6842=LINE('',#55651,#8809);
#6843=LINE('',#55655,#8810);
#6844=LINE('',#55656,#8811);
#6845=LINE('',#55657,#8812);
#6846=LINE('',#55661,#8813);
#6847=LINE('',#55662,#8814);
#6848=LINE('',#55663,#8815);
#6849=LINE('',#55666,#8816);
#6850=LINE('',#55668,#8817);
#6851=LINE('',#55669,#8818);
#6852=LINE('',#55672,#8819);
#6853=LINE('',#55674,#8820);
#6854=LINE('',#55675,#8821);
#6855=LINE('',#55678,#8822);
#6856=LINE('',#55680,#8823);
#6857=LINE('',#55681,#8824);
#6858=LINE('',#55684,#8825);
#6859=LINE('',#55686,#8826);
#6860=LINE('',#55687,#8827);
#6861=LINE('',#55690,#8828);
#6862=LINE('',#55691,#8829);
#6863=LINE('',#55692,#8830);
#6864=LINE('',#55697,#8831);
#6865=LINE('',#55698,#8832);
#6866=LINE('',#55702,#8833);
#6867=LINE('',#55703,#8834);
#6868=LINE('',#55704,#8835);
#6869=LINE('',#55709,#8836);
#6870=LINE('',#55710,#8837);
#6871=LINE('',#55715,#8838);
#6872=LINE('',#55716,#8839);
#6873=LINE('',#55720,#8840);
#6874=LINE('',#55721,#8841);
#6875=LINE('',#55722,#8842);
#6876=LINE('',#55724,#8843);
#6877=LINE('',#55729,#8844);
#6878=LINE('',#55730,#8845);
#6879=LINE('',#55733,#8846);
#6880=LINE('',#55735,#8847);
#6881=LINE('',#55736,#8848);
#6882=LINE('',#55739,#8849);
#6883=LINE('',#55741,#8850);
#6884=LINE('',#55742,#8851);
#6885=LINE('',#55744,#8852);
#6886=LINE('',#55746,#8853);
#6887=LINE('',#55747,#8854);
#6888=LINE('',#55750,#8855);
#6889=LINE('',#55753,#8856);
#6890=LINE('',#55755,#8857);
#6891=LINE('',#55759,#8858);
#6892=LINE('',#55763,#8859);
#6893=LINE('',#55771,#8860);
#6894=LINE('',#55775,#8861);
#6895=LINE('',#55779,#8862);
#6896=LINE('',#55787,#8863);
#6897=LINE('',#55789,#8864);
#6898=LINE('',#55791,#8865);
#6899=LINE('',#55799,#8866);
#6900=LINE('',#55803,#8867);
#6901=LINE('',#55807,#8868);
#6902=LINE('',#55815,#8869);
#6903=LINE('',#55819,#8870);
#6904=LINE('',#55823,#8871);
#6905=LINE('',#55824,#8872);
#6906=LINE('',#55827,#8873);
#6907=LINE('',#55829,#8874);
#6908=LINE('',#55831,#8875);
#6909=LINE('',#55833,#8876);
#6910=LINE('',#55835,#8877);
#6911=LINE('',#55837,#8878);
#6912=LINE('',#55839,#8879);
#6913=LINE('',#55841,#8880);
#6914=LINE('',#55843,#8881);
#6915=LINE('',#55845,#8882);
#6916=LINE('',#55847,#8883);
#6917=LINE('',#55849,#8884);
#6918=LINE('',#55850,#8885);
#6919=LINE('',#55854,#8886);
#6920=LINE('',#55855,#8887);
#6921=LINE('',#55856,#8888);
#6922=LINE('',#55860,#8889);
#6923=LINE('',#55861,#8890);
#6924=LINE('',#55862,#8891);
#6925=LINE('',#55865,#8892);
#6926=LINE('',#55866,#8893);
#6927=LINE('',#55869,#8894);
#6928=LINE('',#55870,#8895);
#6929=LINE('',#55873,#8896);
#6930=LINE('',#55874,#8897);
#6931=LINE('',#55877,#8898);
#6932=LINE('',#55880,#8899);
#6933=LINE('',#55883,#8900);
#6934=LINE('',#55886,#8901);
#6935=LINE('',#55888,#8902);
#6936=LINE('',#55891,#8903);
#6937=LINE('',#55892,#8904);
#6938=LINE('',#55894,#8905);
#6939=LINE('',#55899,#8906);
#6940=LINE('',#55900,#8907);
#6941=LINE('',#55905,#8908);
#6942=LINE('',#55906,#8909);
#6943=LINE('',#55913,#8910);
#6944=LINE('',#55914,#8911);
#6945=LINE('',#55919,#8912);
#6946=LINE('',#55920,#8913);
#6947=LINE('',#55922,#8914);
#6948=LINE('',#55924,#8915);
#6949=LINE('',#55929,#8916);
#6950=LINE('',#55930,#8917);
#6951=LINE('',#55935,#8918);
#6952=LINE('',#55936,#8919);
#6953=LINE('',#55941,#8920);
#6954=LINE('',#55943,#8921);
#6955=LINE('',#55944,#8922);
#6956=LINE('',#55946,#8923);
#6957=LINE('',#55951,#8924);
#6958=LINE('',#55952,#8925);
#6959=LINE('',#55957,#8926);
#6960=LINE('',#55958,#8927);
#6961=LINE('',#55965,#8928);
#6962=LINE('',#55966,#8929);
#6963=LINE('',#55971,#8930);
#6964=LINE('',#55972,#8931);
#6965=LINE('',#55974,#8932);
#6966=LINE('',#55976,#8933);
#6967=LINE('',#55978,#8934);
#6968=LINE('',#55983,#8935);
#6969=LINE('',#55984,#8936);
#6970=LINE('',#55989,#8937);
#6971=LINE('',#55990,#8938);
#6972=LINE('',#55995,#8939);
#6973=LINE('',#55998,#8940);
#6974=LINE('',#56001,#8941);
#6975=LINE('',#56004,#8942);
#6976=LINE('',#56008,#8943);
#6977=LINE('',#56009,#8944);
#6978=LINE('',#56010,#8945);
#6979=LINE('',#56013,#8946);
#6980=LINE('',#56014,#8947);
#6981=LINE('',#56017,#8948);
#6982=LINE('',#56018,#8949);
#6983=LINE('',#56020,#8950);
#6984=LINE('',#56023,#8951);
#6985=LINE('',#56024,#8952);
#6986=LINE('',#56026,#8953);
#6987=LINE('',#56028,#8954);
#6988=LINE('',#56030,#8955);
#6989=LINE('',#56032,#8956);
#6990=LINE('',#56034,#8957);
#6991=LINE('',#56036,#8958);
#6992=LINE('',#56039,#8959);
#6993=LINE('',#56040,#8960);
#6994=LINE('',#56042,#8961);
#6995=LINE('',#56046,#8962);
#6996=LINE('',#56047,#8963);
#6997=LINE('',#56051,#8964);
#6998=LINE('',#56053,#8965);
#6999=LINE('',#56098,#8966);
#7000=LINE('',#56141,#8967);
#7001=LINE('',#56160,#8968);
#7002=LINE('',#56197,#8969);
#7003=LINE('',#56198,#8970);
#7004=LINE('',#56201,#8971);
#7005=LINE('',#56202,#8972);
#7006=LINE('',#56205,#8973);
#7007=LINE('',#56206,#8974);
#7008=LINE('',#56209,#8975);
#7009=LINE('',#56210,#8976);
#7010=LINE('',#56213,#8977);
#7011=LINE('',#56214,#8978);
#7012=LINE('',#56217,#8979);
#7013=LINE('',#56218,#8980);
#7014=LINE('',#56222,#8981);
#7015=LINE('',#56223,#8982);
#7016=LINE('',#56224,#8983);
#7017=LINE('',#56227,#8984);
#7018=LINE('',#56228,#8985);
#7019=LINE('',#56231,#8986);
#7020=LINE('',#56232,#8987);
#7021=LINE('',#56235,#8988);
#7022=LINE('',#56236,#8989);
#7023=LINE('',#56239,#8990);
#7024=LINE('',#56240,#8991);
#7025=LINE('',#56242,#8992);
#7026=LINE('',#56325,#8993);
#7027=LINE('',#56326,#8994);
#7028=LINE('',#56328,#8995);
#7029=LINE('',#56330,#8996);
#7030=LINE('',#56332,#8997);
#7031=LINE('',#56334,#8998);
#7032=LINE('',#56352,#8999);
#7033=LINE('',#56356,#9000);
#7034=LINE('',#56361,#9001);
#7035=LINE('',#56365,#9002);
#7036=LINE('',#56370,#9003);
#7037=LINE('',#56374,#9004);
#7038=LINE('',#56379,#9005);
#7039=LINE('',#56383,#9006);
#7040=LINE('',#56388,#9007);
#7041=LINE('',#56392,#9008);
#7042=LINE('',#56397,#9009);
#7043=LINE('',#56401,#9010);
#7044=LINE('',#56406,#9011);
#7045=LINE('',#56410,#9012);
#7046=LINE('',#56415,#9013);
#7047=LINE('',#56419,#9014);
#7048=LINE('',#56423,#9015);
#7049=LINE('',#56425,#9016);
#7050=LINE('',#56427,#9017);
#7051=LINE('',#56428,#9018);
#7052=LINE('',#56431,#9019);
#7053=LINE('',#56435,#9020);
#7054=LINE('',#56439,#9021);
#7055=LINE('',#56441,#9022);
#7056=LINE('',#56443,#9023);
#7057=LINE('',#56445,#9024);
#7058=LINE('',#56446,#9025);
#7059=LINE('',#56449,#9026);
#7060=LINE('',#56451,#9027);
#7061=LINE('',#56452,#9028);
#7062=LINE('',#56456,#9029);
#7063=LINE('',#56460,#9030);
#7064=LINE('',#56463,#9031);
#7065=LINE('',#56464,#9032);
#7066=LINE('',#56466,#9033);
#7067=LINE('',#56467,#9034);
#7068=LINE('',#56469,#9035);
#7069=LINE('',#56470,#9036);
#7070=LINE('',#56474,#9037);
#7071=LINE('',#56476,#9038);
#7072=LINE('',#56477,#9039);
#7073=LINE('',#56479,#9040);
#7074=LINE('',#56489,#9041);
#7075=LINE('',#56494,#9042);
#7076=LINE('',#56510,#9043);
#7077=LINE('',#56516,#9044);
#7078=LINE('',#56522,#9045);
#7079=LINE('',#56527,#9046);
#7080=LINE('',#56529,#9047);
#7081=LINE('',#56531,#9048);
#7082=LINE('',#56533,#9049);
#7083=LINE('',#56535,#9050);
#7084=LINE('',#56536,#9051);
#7085=LINE('',#56542,#9052);
#7086=LINE('',#56543,#9053);
#7087=LINE('',#56545,#9054);
#7088=LINE('',#56546,#9055);
#7089=LINE('',#56549,#9056);
#7090=LINE('',#56550,#9057);
#7091=LINE('',#56551,#9058);
#7092=LINE('',#56554,#9059);
#7093=LINE('',#56555,#9060);
#7094=LINE('',#56556,#9061);
#7095=LINE('',#56559,#9062);
#7096=LINE('',#56560,#9063);
#7097=LINE('',#56561,#9064);
#7098=LINE('',#56564,#9065);
#7099=LINE('',#56565,#9066);
#7100=LINE('',#56566,#9067);
#7101=LINE('',#56568,#9068);
#7102=LINE('',#56569,#9069);
#7103=LINE('',#56580,#9070);
#7104=LINE('',#56586,#9071);
#7105=LINE('',#56595,#9072);
#7106=LINE('',#56598,#9073);
#7107=LINE('',#56604,#9074);
#7108=LINE('',#56607,#9075);
#7109=LINE('',#56609,#9076);
#7110=LINE('',#56610,#9077);
#7111=LINE('',#56612,#9078);
#7112=LINE('',#56613,#9079);
#7113=LINE('',#56621,#9080);
#7114=LINE('',#56625,#9081);
#7115=LINE('',#56632,#9082);
#7116=LINE('',#56637,#9083);
#7117=LINE('',#56643,#9084);
#7118=LINE('',#56645,#9085);
#7119=LINE('',#56647,#9086);
#7120=LINE('',#56649,#9087);
#7121=LINE('',#56651,#9088);
#7122=LINE('',#56652,#9089);
#7123=LINE('',#56656,#9090);
#7124=LINE('',#56658,#9091);
#7125=LINE('',#56659,#9092);
#7126=LINE('',#56662,#9093);
#7127=LINE('',#56663,#9094);
#7128=LINE('',#56666,#9095);
#7129=LINE('',#56667,#9096);
#7130=LINE('',#56670,#9097);
#7131=LINE('',#56671,#9098);
#7132=LINE('',#56674,#9099);
#7133=LINE('',#56675,#9100);
#7134=LINE('',#56677,#9101);
#7135=LINE('',#56686,#9102);
#7136=LINE('',#56691,#9103);
#7137=LINE('',#56707,#9104);
#7138=LINE('',#56713,#9105);
#7139=LINE('',#56719,#9106);
#7140=LINE('',#56724,#9107);
#7141=LINE('',#56726,#9108);
#7142=LINE('',#56728,#9109);
#7143=LINE('',#56730,#9110);
#7144=LINE('',#56732,#9111);
#7145=LINE('',#56733,#9112);
#7146=LINE('',#56739,#9113);
#7147=LINE('',#56740,#9114);
#7148=LINE('',#56742,#9115);
#7149=LINE('',#56743,#9116);
#7150=LINE('',#56746,#9117);
#7151=LINE('',#56747,#9118);
#7152=LINE('',#56748,#9119);
#7153=LINE('',#56751,#9120);
#7154=LINE('',#56752,#9121);
#7155=LINE('',#56753,#9122);
#7156=LINE('',#56756,#9123);
#7157=LINE('',#56757,#9124);
#7158=LINE('',#56758,#9125);
#7159=LINE('',#56761,#9126);
#7160=LINE('',#56762,#9127);
#7161=LINE('',#56763,#9128);
#7162=LINE('',#56765,#9129);
#7163=LINE('',#56766,#9130);
#7164=LINE('',#56777,#9131);
#7165=LINE('',#56783,#9132);
#7166=LINE('',#56792,#9133);
#7167=LINE('',#56795,#9134);
#7168=LINE('',#56801,#9135);
#7169=LINE('',#56804,#9136);
#7170=LINE('',#56806,#9137);
#7171=LINE('',#56807,#9138);
#7172=LINE('',#56809,#9139);
#7173=LINE('',#56810,#9140);
#7174=LINE('',#56818,#9141);
#7175=LINE('',#56822,#9142);
#7176=LINE('',#56829,#9143);
#7177=LINE('',#56834,#9144);
#7178=LINE('',#56840,#9145);
#7179=LINE('',#56842,#9146);
#7180=LINE('',#56844,#9147);
#7181=LINE('',#56846,#9148);
#7182=LINE('',#56848,#9149);
#7183=LINE('',#56849,#9150);
#7184=LINE('',#56853,#9151);
#7185=LINE('',#56855,#9152);
#7186=LINE('',#56856,#9153);
#7187=LINE('',#56859,#9154);
#7188=LINE('',#56860,#9155);
#7189=LINE('',#56863,#9156);
#7190=LINE('',#56864,#9157);
#7191=LINE('',#56867,#9158);
#7192=LINE('',#56868,#9159);
#7193=LINE('',#56871,#9160);
#7194=LINE('',#56872,#9161);
#7195=LINE('',#56874,#9162);
#7196=LINE('',#56881,#9163);
#7197=LINE('',#56885,#9164);
#7198=LINE('',#56892,#9165);
#7199=LINE('',#56897,#9166);
#7200=LINE('',#56903,#9167);
#7201=LINE('',#56905,#9168);
#7202=LINE('',#56907,#9169);
#7203=LINE('',#56909,#9170);
#7204=LINE('',#56911,#9171);
#7205=LINE('',#56912,#9172);
#7206=LINE('',#56916,#9173);
#7207=LINE('',#56918,#9174);
#7208=LINE('',#56919,#9175);
#7209=LINE('',#56922,#9176);
#7210=LINE('',#56923,#9177);
#7211=LINE('',#56926,#9178);
#7212=LINE('',#56927,#9179);
#7213=LINE('',#56930,#9180);
#7214=LINE('',#56931,#9181);
#7215=LINE('',#56934,#9182);
#7216=LINE('',#56935,#9183);
#7217=LINE('',#56937,#9184);
#7218=VECTOR('',#27485,3.);
#7219=VECTOR('',#27492,3.);
#7220=VECTOR('',#27499,3.);
#7221=VECTOR('',#27506,3.);
#7222=VECTOR('',#27513,3.4);
#7223=VECTOR('',#27520,3.4);
#7224=VECTOR('',#27527,3.4);
#7225=VECTOR('',#27534,3.4);
#7226=VECTOR('',#27541,3.);
#7227=VECTOR('',#27546,3.);
#7228=VECTOR('',#27551,3.);
#7229=VECTOR('',#27556,3.);
#7230=VECTOR('',#27561,2.49999999999999);
#7231=VECTOR('',#27566,2.49999999999999);
#7232=VECTOR('',#27571,2.49999999999999);
#7233=VECTOR('',#27576,2.49999999999999);
#7234=VECTOR('',#27579,1000.);
#7235=VECTOR('',#27580,1000.);
#7236=VECTOR('',#27581,1000.);
#7237=VECTOR('',#27582,1000.);
#7238=VECTOR('',#27585,1000.);
#7239=VECTOR('',#27586,1000.);
#7240=VECTOR('',#27587,1000.);
#7241=VECTOR('',#27588,1000.);
#7242=VECTOR('',#27591,1000.);
#7243=VECTOR('',#27592,1000.);
#7244=VECTOR('',#27593,1000.);
#7245=VECTOR('',#27596,1000.);
#7246=VECTOR('',#27597,1000.);
#7247=VECTOR('',#27600,1000.);
#7248=VECTOR('',#27601,1000.);
#7249=VECTOR('',#27602,1000.);
#7250=VECTOR('',#27605,1000.);
#7251=VECTOR('',#27606,1000.);
#7252=VECTOR('',#27607,1000.);
#7253=VECTOR('',#27610,1000.);
#7254=VECTOR('',#27611,1000.);
#7255=VECTOR('',#27612,1000.);
#7256=VECTOR('',#27615,1000.);
#7257=VECTOR('',#27618,1000.);
#7258=VECTOR('',#27631,5.00000000000009);
#7259=VECTOR('',#27634,1000.);
#7260=VECTOR('',#27635,1000.);
#7261=VECTOR('',#27648,5.50000000000001);
#7262=VECTOR('',#27655,6.00000000000005);
#7263=VECTOR('',#27666,7.00000000000006);
#7264=VECTOR('',#27675,7.50000000000004);
#7265=VECTOR('',#27678,7.49999999999999);
#7266=VECTOR('',#27693,5.);
#7267=VECTOR('',#27698,4.8);
#7268=VECTOR('',#27707,5.);
#7269=VECTOR('',#27712,5.);
#7270=VECTOR('',#27731,1000.);
#7271=VECTOR('',#27732,1000.);
#7272=VECTOR('',#27733,1000.);
#7273=VECTOR('',#27738,1000.);
#7274=VECTOR('',#27739,1000.);
#7275=VECTOR('',#27742,1000.);
#7276=VECTOR('',#27743,1000.);
#7277=VECTOR('',#27754,2.45849999999999);
#7278=VECTOR('',#27759,2.74999999999999);
#7279=VECTOR('',#27766,2.74999999999999);
#7280=VECTOR('',#27773,2.74999999999999);
#7281=VECTOR('',#27780,2.74999999999999);
#7282=VECTOR('',#27787,2.74999999999999);
#7283=VECTOR('',#27794,2.74999999999999);
#7284=VECTOR('',#27801,14.);
#7285=VECTOR('',#27808,11.);
#7286=VECTOR('',#27815,10.75);
#7287=VECTOR('',#27822,7.5);
#7288=VECTOR('',#27829,10.75);
#7289=VECTOR('',#27836,11.);
#7290=VECTOR('',#27847,1000.);
#7291=VECTOR('',#27850,1000.);
#7292=VECTOR('',#27863,1000.);
#7293=VECTOR('',#27866,1000.);
#7294=VECTOR('',#27869,1000.);
#7295=VECTOR('',#27870,1000.);
#7296=VECTOR('',#27883,1000.);
#7297=VECTOR('',#27884,1000.);
#7298=VECTOR('',#27911,4.49999999999999);
#7299=VECTOR('',#27918,4.49999999999999);
#7300=VECTOR('',#27925,12.);
#7301=VECTOR('',#27932,7.75);
#7302=VECTOR('',#27939,6.);
#7303=VECTOR('',#27946,7.74999999999999);
#7304=VECTOR('',#27953,12.);
#7305=VECTOR('',#27958,1.5);
#7306=VECTOR('',#27973,1.5);
#7307=VECTOR('',#27988,1.5);
#7308=VECTOR('',#28003,1.5);
#7309=VECTOR('',#28020,3.1);
#7310=VECTOR('',#28027,3.1);
#7311=VECTOR('',#28034,3.1);
#7312=VECTOR('',#28041,3.1);
#7313=VECTOR('',#28048,3.5);
#7314=VECTOR('',#28055,3.5);
#7315=VECTOR('',#28062,3.50000000000001);
#7316=VECTOR('',#28069,3.50000000000001);
#7317=VECTOR('',#28082,1000.);
#7318=VECTOR('',#28083,1000.);
#7319=VECTOR('',#28084,1000.);
#7320=VECTOR('',#28085,1000.);
#7321=VECTOR('',#28086,1000.);
#7322=VECTOR('',#28087,1000.);
#7323=VECTOR('',#28088,1000.);
#7324=VECTOR('',#28089,1000.);
#7325=VECTOR('',#28090,1000.);
#7326=VECTOR('',#28091,1000.);
#7327=VECTOR('',#28092,1000.);
#7328=VECTOR('',#28093,1000.);
#7329=VECTOR('',#28094,1000.);
#7330=VECTOR('',#28095,1000.);
#7331=VECTOR('',#28096,1000.);
#7332=VECTOR('',#28097,1000.);
#7333=VECTOR('',#28098,1000.);
#7334=VECTOR('',#28099,1000.);
#7335=VECTOR('',#28100,1000.);
#7336=VECTOR('',#28101,1000.);
#7337=VECTOR('',#28104,1000.);
#7338=VECTOR('',#28105,1000.);
#7339=VECTOR('',#28106,1000.);
#7340=VECTOR('',#28109,1000.);
#7341=VECTOR('',#28110,1000.);
#7342=VECTOR('',#28113,1000.);
#7343=VECTOR('',#28114,1000.);
#7344=VECTOR('',#28117,1000.);
#7345=VECTOR('',#28118,1000.);
#7346=VECTOR('',#28121,1000.);
#7347=VECTOR('',#28122,1000.);
#7348=VECTOR('',#28125,1000.);
#7349=VECTOR('',#28126,1000.);
#7350=VECTOR('',#28129,1000.);
#7351=VECTOR('',#28130,1000.);
#7352=VECTOR('',#28133,1000.);
#7353=VECTOR('',#28134,1000.);
#7354=VECTOR('',#28137,1000.);
#7355=VECTOR('',#28138,1000.);
#7356=VECTOR('',#28141,1000.);
#7357=VECTOR('',#28142,1000.);
#7358=VECTOR('',#28145,1000.);
#7359=VECTOR('',#28146,1000.);
#7360=VECTOR('',#28149,1000.);
#7361=VECTOR('',#28154,1000.);
#7362=VECTOR('',#28155,1000.);
#7363=VECTOR('',#28156,1000.);
#7364=VECTOR('',#28157,1000.);
#7365=VECTOR('',#28158,1000.);
#7366=VECTOR('',#28159,1000.);
#7367=VECTOR('',#28160,1000.);
#7368=VECTOR('',#28161,1000.);
#7369=VECTOR('',#28164,1000.);
#7370=VECTOR('',#28165,1000.);
#7371=VECTOR('',#28168,1000.);
#7372=VECTOR('',#28171,1000.);
#7373=VECTOR('',#28174,1000.);
#7374=VECTOR('',#28177,1000.);
#7375=VECTOR('',#28180,1000.);
#7376=VECTOR('',#28183,1000.);
#7377=VECTOR('',#28188,1000.);
#7378=VECTOR('',#28189,1000.);
#7379=VECTOR('',#28190,1000.);
#7380=VECTOR('',#28191,1000.);
#7381=VECTOR('',#28192,1000.);
#7382=VECTOR('',#28193,1000.);
#7383=VECTOR('',#28196,1000.);
#7384=VECTOR('',#28197,1000.);
#7385=VECTOR('',#28198,1000.);
#7386=VECTOR('',#28199,1000.);
#7387=VECTOR('',#28200,1000.);
#7388=VECTOR('',#28201,1000.);
#7389=VECTOR('',#28204,1000.);
#7390=VECTOR('',#28205,1000.);
#7391=VECTOR('',#28206,1000.);
#7392=VECTOR('',#28207,1000.);
#7393=VECTOR('',#28208,1000.);
#7394=VECTOR('',#28209,1000.);
#7395=VECTOR('',#28212,1000.);
#7396=VECTOR('',#28213,1000.);
#7397=VECTOR('',#28214,1000.);
#7398=VECTOR('',#28215,1000.);
#7399=VECTOR('',#28216,1000.);
#7400=VECTOR('',#28217,1000.);
#7401=VECTOR('',#28220,1000.);
#7402=VECTOR('',#28221,1000.);
#7403=VECTOR('',#28222,1000.);
#7404=VECTOR('',#28223,1000.);
#7405=VECTOR('',#28226,1000.);
#7406=VECTOR('',#28227,1000.);
#7407=VECTOR('',#28228,1000.);
#7408=VECTOR('',#28231,1000.);
#7409=VECTOR('',#28232,1000.);
#7410=VECTOR('',#28233,1000.);
#7411=VECTOR('',#28236,1000.);
#7412=VECTOR('',#28237,1000.);
#7413=VECTOR('',#28238,1000.);
#7414=VECTOR('',#28241,1000.);
#7415=VECTOR('',#28242,1000.);
#7416=VECTOR('',#28243,1000.);
#7417=VECTOR('',#28246,1000.);
#7418=VECTOR('',#28247,1000.);
#7419=VECTOR('',#28262,1000.);
#7420=VECTOR('',#28263,1000.);
#7421=VECTOR('',#28264,1000.);
#7422=VECTOR('',#28265,1000.);
#7423=VECTOR('',#28268,1000.);
#7424=VECTOR('',#28269,1000.);
#7425=VECTOR('',#28270,1000.);
#7426=VECTOR('',#28273,1000.);
#7427=VECTOR('',#28274,1000.);
#7428=VECTOR('',#28275,1000.);
#7429=VECTOR('',#28278,1000.);
#7430=VECTOR('',#28279,1000.);
#7431=VECTOR('',#28280,1000.);
#7432=VECTOR('',#28283,1000.);
#7433=VECTOR('',#28284,1000.);
#7434=VECTOR('',#28285,1000.);
#7435=VECTOR('',#28288,1000.);
#7436=VECTOR('',#28289,1000.);
#7437=VECTOR('',#28304,1000.);
#7438=VECTOR('',#28305,1000.);
#7439=VECTOR('',#28306,1000.);
#7440=VECTOR('',#28307,1000.);
#7441=VECTOR('',#28310,1000.);
#7442=VECTOR('',#28311,1000.);
#7443=VECTOR('',#28312,1000.);
#7444=VECTOR('',#28315,1000.);
#7445=VECTOR('',#28316,1000.);
#7446=VECTOR('',#28317,1000.);
#7447=VECTOR('',#28320,1000.);
#7448=VECTOR('',#28321,1000.);
#7449=VECTOR('',#28322,1000.);
#7450=VECTOR('',#28325,1000.);
#7451=VECTOR('',#28326,1000.);
#7452=VECTOR('',#28327,1000.);
#7453=VECTOR('',#28330,1000.);
#7454=VECTOR('',#28331,1000.);
#7455=VECTOR('',#28346,1000.);
#7456=VECTOR('',#28347,1000.);
#7457=VECTOR('',#28348,1000.);
#7458=VECTOR('',#28349,1000.);
#7459=VECTOR('',#28352,1000.);
#7460=VECTOR('',#28353,1000.);
#7461=VECTOR('',#28354,1000.);
#7462=VECTOR('',#28357,1000.);
#7463=VECTOR('',#28358,1000.);
#7464=VECTOR('',#28359,1000.);
#7465=VECTOR('',#28362,1000.);
#7466=VECTOR('',#28363,1000.);
#7467=VECTOR('',#28364,1000.);
#7468=VECTOR('',#28367,1000.);
#7469=VECTOR('',#28368,1000.);
#7470=VECTOR('',#28369,1000.);
#7471=VECTOR('',#28372,1000.);
#7472=VECTOR('',#28373,1000.);
#7473=VECTOR('',#28398,1.621);
#7474=VECTOR('',#28403,5.4585);
#7475=VECTOR('',#28412,6.);
#7476=VECTOR('',#28417,5.4585);
#7477=VECTOR('',#28422,1000.);
#7478=VECTOR('',#28425,1000.);
#7479=VECTOR('',#28430,8.5);
#7480=VECTOR('',#28437,1000.);
#7481=VECTOR('',#28440,1000.);
#7482=VECTOR('',#28445,1000.);
#7483=VECTOR('',#28448,1000.);
#7484=VECTOR('',#28453,1000.);
#7485=VECTOR('',#28456,1000.);
#7486=VECTOR('',#28461,1000.);
#7487=VECTOR('',#28462,1000.);
#7488=VECTOR('',#28463,1000.);
#7489=VECTOR('',#28464,1000.);
#7490=VECTOR('',#28467,1000.);
#7491=VECTOR('',#28468,1000.);
#7492=VECTOR('',#28469,1000.);
#7493=VECTOR('',#28470,1000.);
#7494=VECTOR('',#28483,2.);
#7495=VECTOR('',#28490,1.25);
#7496=VECTOR('',#28497,2.);
#7497=VECTOR('',#28502,1000.);
#7498=VECTOR('',#28503,1000.);
#7499=VECTOR('',#28504,1000.);
#7500=VECTOR('',#28505,1000.);
#7501=VECTOR('',#28506,1000.);
#7502=VECTOR('',#28507,1000.);
#7503=VECTOR('',#28510,1000.);
#7504=VECTOR('',#28511,1000.);
#7505=VECTOR('',#28512,1000.);
#7506=VECTOR('',#28515,1000.);
#7507=VECTOR('',#28516,1000.);
#7508=VECTOR('',#28519,1000.);
#7509=VECTOR('',#28520,1000.);
#7510=VECTOR('',#28523,1000.);
#7511=VECTOR('',#28524,1000.);
#7512=VECTOR('',#28527,1000.);
#7513=VECTOR('',#28528,1000.);
#7514=VECTOR('',#28531,1000.);
#7515=VECTOR('',#28540,7.75);
#7516=VECTOR('',#28547,6.);
#7517=VECTOR('',#28570,4.49999999999999);
#7518=VECTOR('',#28577,4.49999999999999);
#7519=VECTOR('',#28584,13.);
#7520=VECTOR('',#28589,1000.);
#7521=VECTOR('',#28590,1000.);
#7522=VECTOR('',#28591,1000.);
#7523=VECTOR('',#28592,1000.);
#7524=VECTOR('',#28593,1000.);
#7525=VECTOR('',#28594,1000.);
#7526=VECTOR('',#28595,1000.);
#7527=VECTOR('',#28596,1000.);
#7528=VECTOR('',#28597,1000.);
#7529=VECTOR('',#28598,1000.);
#7530=VECTOR('',#28599,1000.);
#7531=VECTOR('',#28600,1000.);
#7532=VECTOR('',#28603,1000.);
#7533=VECTOR('',#28604,1000.);
#7534=VECTOR('',#28605,1000.);
#7535=VECTOR('',#28606,1000.);
#7536=VECTOR('',#28607,1000.);
#7537=VECTOR('',#28608,1000.);
#7538=VECTOR('',#28609,1000.);
#7539=VECTOR('',#28610,1000.);
#7540=VECTOR('',#28611,1000.);
#7541=VECTOR('',#28612,1000.);
#7542=VECTOR('',#28613,1000.);
#7543=VECTOR('',#28614,1000.);
#7544=VECTOR('',#28617,1000.);
#7545=VECTOR('',#28618,1000.);
#7546=VECTOR('',#28621,1000.);
#7547=VECTOR('',#28624,1000.);
#7548=VECTOR('',#28627,1000.);
#7549=VECTOR('',#28630,1000.);
#7550=VECTOR('',#28633,1000.);
#7551=VECTOR('',#28636,1000.);
#7552=VECTOR('',#28639,1000.);
#7553=VECTOR('',#28642,1000.);
#7554=VECTOR('',#28645,1000.);
#7555=VECTOR('',#28648,1000.);
#7556=VECTOR('',#28661,5.);
#7557=VECTOR('',#28674,6.7);
#7558=VECTOR('',#28681,9.8);
#7559=VECTOR('',#28694,13.);
#7560=VECTOR('',#28707,9.8);
#7561=VECTOR('',#28714,6.69999999999999);
#7562=VECTOR('',#28735,0.6);
#7563=VECTOR('',#28742,0.6);
#7564=VECTOR('',#28749,1000.);
#7565=VECTOR('',#28752,1000.);
#7566=VECTOR('',#28757,1000.);
#7567=VECTOR('',#28760,1000.);
#7568=VECTOR('',#28763,1000.);
#7569=VECTOR('',#28766,1000.);
#7570=VECTOR('',#28771,1000.);
#7571=VECTOR('',#28774,1000.);
#7572=VECTOR('',#28775,1000.);
#7573=VECTOR('',#28776,1000.);
#7574=VECTOR('',#28779,1000.);
#7575=VECTOR('',#28780,1000.);
#7576=VECTOR('',#28781,1000.);
#7577=VECTOR('',#28782,1000.);
#7578=VECTOR('',#28785,1000.);
#7579=VECTOR('',#28790,1000.);
#7580=VECTOR('',#28795,1000.);
#7581=VECTOR('',#28796,1000.);
#7582=VECTOR('',#28799,1000.);
#7583=VECTOR('',#28802,1000.);
#7584=VECTOR('',#28807,1000.);
#7585=VECTOR('',#28810,1000.);
#7586=VECTOR('',#28813,1000.);
#7587=VECTOR('',#28816,1000.);
#7588=VECTOR('',#28831,3.);
#7589=VECTOR('',#28838,3.);
#7590=VECTOR('',#28845,4.25000000000001);
#7591=VECTOR('',#28852,4.25000000000001);
#7592=VECTOR('',#28857,1000.);
#7593=VECTOR('',#28858,1000.);
#7594=VECTOR('',#28859,1000.);
#7595=VECTOR('',#28860,1000.);
#7596=VECTOR('',#28863,1000.);
#7597=VECTOR('',#28864,1000.);
#7598=VECTOR('',#28865,1000.);
#7599=VECTOR('',#28866,1000.);
#7600=VECTOR('',#28867,1000.);
#7601=VECTOR('',#28870,1000.);
#7602=VECTOR('',#28871,1000.);
#7603=VECTOR('',#28872,1000.);
#7604=VECTOR('',#28873,1000.);
#7605=VECTOR('',#28876,1000.);
#7606=VECTOR('',#28877,1000.);
#7607=VECTOR('',#28878,1000.);
#7608=VECTOR('',#28879,1000.);
#7609=VECTOR('',#28880,1000.);
#7610=VECTOR('',#28883,1000.);
#7611=VECTOR('',#28884,1000.);
#7612=VECTOR('',#28885,1000.);
#7613=VECTOR('',#28886,1000.);
#7614=VECTOR('',#28889,1000.);
#7615=VECTOR('',#28890,1000.);
#7616=VECTOR('',#28895,1000.);
#7617=VECTOR('',#28896,1000.);
#7618=VECTOR('',#28899,1000.);
#7619=VECTOR('',#28902,1000.);
#7620=VECTOR('',#28903,1000.);
#7621=VECTOR('',#28906,1000.);
#7622=VECTOR('',#28915,3.);
#7623=VECTOR('',#28922,3.);
#7624=VECTOR('',#28929,4.25000000000001);
#7625=VECTOR('',#28936,4.25000000000001);
#7626=VECTOR('',#28941,1000.);
#7627=VECTOR('',#28942,1000.);
#7628=VECTOR('',#28943,1000.);
#7629=VECTOR('',#28944,1000.);
#7630=VECTOR('',#28947,1000.);
#7631=VECTOR('',#28948,1000.);
#7632=VECTOR('',#28949,1000.);
#7633=VECTOR('',#28950,1000.);
#7634=VECTOR('',#28951,1000.);
#7635=VECTOR('',#28954,1000.);
#7636=VECTOR('',#28955,1000.);
#7637=VECTOR('',#28956,1000.);
#7638=VECTOR('',#28957,1000.);
#7639=VECTOR('',#28960,1000.);
#7640=VECTOR('',#28961,1000.);
#7641=VECTOR('',#28962,1000.);
#7642=VECTOR('',#28963,1000.);
#7643=VECTOR('',#28964,1000.);
#7644=VECTOR('',#28967,1000.);
#7645=VECTOR('',#28968,1000.);
#7646=VECTOR('',#28969,1000.);
#7647=VECTOR('',#28970,1000.);
#7648=VECTOR('',#28973,1000.);
#7649=VECTOR('',#28974,1000.);
#7650=VECTOR('',#28979,1000.);
#7651=VECTOR('',#28980,1000.);
#7652=VECTOR('',#28983,1000.);
#7653=VECTOR('',#28986,1000.);
#7654=VECTOR('',#28987,1000.);
#7655=VECTOR('',#28990,1000.);
#7656=VECTOR('',#28999,1.65);
#7657=VECTOR('',#29006,1.65);
#7658=VECTOR('',#29013,1.65);
#7659=VECTOR('',#29020,1.65);
#7660=VECTOR('',#29027,3.);
#7661=VECTOR('',#29034,3.);
#7662=VECTOR('',#29041,5.5);
#7663=VECTOR('',#29048,3.3);
#7664=VECTOR('',#29055,5.5);
#7665=VECTOR('',#29062,3.3);
#7666=VECTOR('',#29069,10.);
#7667=VECTOR('',#29076,25.);
#7668=VECTOR('',#29081,1000.);
#7669=VECTOR('',#29082,1000.);
#7670=VECTOR('',#29083,1000.);
#7671=VECTOR('',#29084,1000.);
#7672=VECTOR('',#29087,1000.);
#7673=VECTOR('',#29088,1000.);
#7674=VECTOR('',#29089,1000.);
#7675=VECTOR('',#29092,1000.);
#7676=VECTOR('',#29093,1000.);
#7677=VECTOR('',#29096,1000.);
#7678=VECTOR('',#29097,1000.);
#7679=VECTOR('',#29100,1000.);
#7680=VECTOR('',#29121,1.5);
#7681=VECTOR('',#29128,9.);
#7682=VECTOR('',#29139,1.5);
#7683=VECTOR('',#29432,1.5);
#7684=VECTOR('',#29441,1.5);
#7685=VECTOR('',#29454,1.5);
#7686=VECTOR('',#29463,1.5);
#7687=VECTOR('',#29474,1000.);
#7688=VECTOR('',#29475,1000.);
#7689=VECTOR('',#29476,1000.);
#7690=VECTOR('',#29477,1000.);
#7691=VECTOR('',#29478,1000.);
#7692=VECTOR('',#29479,1000.);
#7693=VECTOR('',#29486,2.5);
#7694=VECTOR('',#29489,1000.);
#7695=VECTOR('',#29490,1000.);
#7696=VECTOR('',#29491,1000.);
#7697=VECTOR('',#29492,1000.);
#7698=VECTOR('',#29493,1000.);
#7699=VECTOR('',#29494,1000.);
#7700=VECTOR('',#29497,1000.);
#7701=VECTOR('',#29498,1000.);
#7702=VECTOR('',#29501,1000.);
#7703=VECTOR('',#29504,1000.);
#7704=VECTOR('',#29507,1000.);
#7705=VECTOR('',#29510,1000.);
#7706=VECTOR('',#29529,1000.);
#7707=VECTOR('',#29532,1000.);
#7708=VECTOR('',#29533,1000.);
#7709=VECTOR('',#29538,19.5);
#7710=VECTOR('',#29541,1000.);
#7711=VECTOR('',#29542,1000.);
#7712=VECTOR('',#29569,1000.);
#7713=VECTOR('',#29570,1000.);
#7714=VECTOR('',#29573,1000.);
#7715=VECTOR('',#29576,1000.);
#7716=VECTOR('',#29579,1000.);
#7717=VECTOR('',#29582,1000.);
#7718=VECTOR('',#29585,1000.);
#7719=VECTOR('',#29590,1000.);
#7720=VECTOR('',#29597,1000.);
#7721=VECTOR('',#29614,1000.);
#7722=VECTOR('',#29615,1000.);
#7723=VECTOR('',#29616,1000.);
#7724=VECTOR('',#29621,1000.);
#7725=VECTOR('',#29624,1000.);
#7726=VECTOR('',#29627,1000.);
#7727=VECTOR('',#29630,1000.);
#7728=VECTOR('',#29631,1000.);
#7729=VECTOR('',#29634,1000.);
#7730=VECTOR('',#29635,1000.);
#7731=VECTOR('',#29644,2.1);
#7732=VECTOR('',#29647,20.);
#7733=VECTOR('',#29648,20.);
#7734=VECTOR('',#29651,1000.);
#7735=VECTOR('',#29654,1000.);
#7736=VECTOR('',#29657,1000.);
#7737=VECTOR('',#29660,1000.);
#7738=VECTOR('',#29663,1000.);
#7739=VECTOR('',#29666,1000.);
#7740=VECTOR('',#29669,1000.);
#7741=VECTOR('',#29672,1000.);
#7742=VECTOR('',#29673,1000.);
#7743=VECTOR('',#29678,1000.);
#7744=VECTOR('',#29685,1000.);
#7745=VECTOR('',#29690,1000.);
#7746=VECTOR('',#29693,1000.);
#7747=VECTOR('',#29698,1000.);
#7748=VECTOR('',#29703,1000.);
#7749=VECTOR('',#29708,1000.);
#7750=VECTOR('',#29715,1000.);
#7751=VECTOR('',#29718,1000.);
#7752=VECTOR('',#29721,1000.);
#7753=VECTOR('',#29724,1000.);
#7754=VECTOR('',#29727,1000.);
#7755=VECTOR('',#29728,1000.);
#7756=VECTOR('',#29731,1000.);
#7757=VECTOR('',#29734,1000.);
#7758=VECTOR('',#29737,1000.);
#7759=VECTOR('',#29740,1000.);
#7760=VECTOR('',#29743,1000.);
#7761=VECTOR('',#29746,1000.);
#7762=VECTOR('',#29751,1000.);
#7763=VECTOR('',#29754,1000.);
#7764=VECTOR('',#29757,1000.);
#7765=VECTOR('',#29758,1000.);
#7766=VECTOR('',#29761,1000.);
#7767=VECTOR('',#29766,1000.);
#7768=VECTOR('',#29767,1000.);
#7769=VECTOR('',#29768,1000.);
#7770=VECTOR('',#29771,1000.);
#7771=VECTOR('',#29776,1000.);
#7772=VECTOR('',#29781,1000.);
#7773=VECTOR('',#29782,1000.);
#7774=VECTOR('',#29785,1000.);
#7775=VECTOR('',#29790,1000.);
#7776=VECTOR('',#29791,1000.);
#7777=VECTOR('',#29806,1000.);
#7778=VECTOR('',#29811,1000.);
#7779=VECTOR('',#29816,1000.);
#7780=VECTOR('',#29817,1000.);
#7781=VECTOR('',#29820,1000.);
#7782=VECTOR('',#29823,1000.);
#7783=VECTOR('',#29826,1000.);
#7784=VECTOR('',#29829,1000.);
#7785=VECTOR('',#29834,1000.);
#7786=VECTOR('',#29835,1000.);
#7787=VECTOR('',#29836,1000.);
#7788=VECTOR('',#29839,1000.);
#7789=VECTOR('',#29844,1000.);
#7790=VECTOR('',#29849,1000.);
#7791=VECTOR('',#29850,1000.);
#7792=VECTOR('',#29855,1000.);
#7793=VECTOR('',#29864,1000.);
#7794=VECTOR('',#29867,1000.);
#7795=VECTOR('',#29870,1000.);
#7796=VECTOR('',#29871,1000.);
#7797=VECTOR('',#29874,1000.);
#7798=VECTOR('',#29879,1000.);
#7799=VECTOR('',#29882,1000.);
#7800=VECTOR('',#29883,1000.);
#7801=VECTOR('',#29886,1000.);
#7802=VECTOR('',#29889,1000.);
#7803=VECTOR('',#29892,1000.);
#7804=VECTOR('',#29893,1000.);
#7805=VECTOR('',#29896,1000.);
#7806=VECTOR('',#29901,1000.);
#7807=VECTOR('',#29902,1000.);
#7808=VECTOR('',#29905,1000.);
#7809=VECTOR('',#29910,1000.);
#7810=VECTOR('',#29913,1000.);
#7811=VECTOR('',#29916,1000.);
#7812=VECTOR('',#29925,1000.);
#7813=VECTOR('',#29926,1000.);
#7814=VECTOR('',#29927,1000.);
#7815=VECTOR('',#29928,1000.);
#7816=VECTOR('',#29929,1000.);
#7817=VECTOR('',#29930,1000.);
#7818=VECTOR('',#29937,2.5);
#7819=VECTOR('',#29940,1000.);
#7820=VECTOR('',#29941,1000.);
#7821=VECTOR('',#29942,1000.);
#7822=VECTOR('',#29943,1000.);
#7823=VECTOR('',#29944,1000.);
#7824=VECTOR('',#29945,1000.);
#7825=VECTOR('',#29948,1000.);
#7826=VECTOR('',#29949,1000.);
#7827=VECTOR('',#29952,1000.);
#7828=VECTOR('',#29955,1000.);
#7829=VECTOR('',#29958,1000.);
#7830=VECTOR('',#29961,1000.);
#7831=VECTOR('',#29980,1000.);
#7832=VECTOR('',#29981,1000.);
#7833=VECTOR('',#29982,1000.);
#7834=VECTOR('',#29989,19.5);
#7835=VECTOR('',#29992,1000.);
#7836=VECTOR('',#29993,1000.);
#7837=VECTOR('',#30020,1000.);
#7838=VECTOR('',#30021,1000.);
#7839=VECTOR('',#30024,1000.);
#7840=VECTOR('',#30027,1000.);
#7841=VECTOR('',#30030,1000.);
#7842=VECTOR('',#30033,1000.);
#7843=VECTOR('',#30036,1000.);
#7844=VECTOR('',#30041,1000.);
#7845=VECTOR('',#30048,1000.);
#7846=VECTOR('',#30065,1000.);
#7847=VECTOR('',#30068,1000.);
#7848=VECTOR('',#30069,1000.);
#7849=VECTOR('',#30072,1000.);
#7850=VECTOR('',#30075,1000.);
#7851=VECTOR('',#30078,1000.);
#7852=VECTOR('',#30081,1000.);
#7853=VECTOR('',#30082,1000.);
#7854=VECTOR('',#30083,1000.);
#7855=VECTOR('',#30084,1000.);
#7856=VECTOR('',#30087,1000.);
#7857=VECTOR('',#30088,1000.);
#7858=VECTOR('',#30091,1000.);
#7859=VECTOR('',#30092,1000.);
#7860=VECTOR('',#30097,1000.);
#7861=VECTOR('',#30102,1000.);
#7862=VECTOR('',#30107,1000.);
#7863=VECTOR('',#30110,1000.);
#7864=VECTOR('',#30113,2.1);
#7865=VECTOR('',#30116,20.);
#7866=VECTOR('',#30117,20.);
#7867=VECTOR('',#30120,1000.);
#7868=VECTOR('',#30123,1000.);
#7869=VECTOR('',#30126,1000.);
#7870=VECTOR('',#30129,1000.);
#7871=VECTOR('',#30132,1000.);
#7872=VECTOR('',#30135,1000.);
#7873=VECTOR('',#30138,1000.);
#7874=VECTOR('',#30141,1000.);
#7875=VECTOR('',#30142,1000.);
#7876=VECTOR('',#30147,1000.);
#7877=VECTOR('',#30154,1000.);
#7878=VECTOR('',#30159,1000.);
#7879=VECTOR('',#30162,1000.);
#7880=VECTOR('',#30167,1000.);
#7881=VECTOR('',#30172,1000.);
#7882=VECTOR('',#30177,1000.);
#7883=VECTOR('',#30184,1000.);
#7884=VECTOR('',#30187,1000.);
#7885=VECTOR('',#30190,1000.);
#7886=VECTOR('',#30193,1000.);
#7887=VECTOR('',#30196,1000.);
#7888=VECTOR('',#30197,1000.);
#7889=VECTOR('',#30200,1000.);
#7890=VECTOR('',#30203,1000.);
#7891=VECTOR('',#30206,1000.);
#7892=VECTOR('',#30209,1000.);
#7893=VECTOR('',#30212,1000.);
#7894=VECTOR('',#30215,1000.);
#7895=VECTOR('',#30220,1000.);
#7896=VECTOR('',#30223,1000.);
#7897=VECTOR('',#30226,1000.);
#7898=VECTOR('',#30227,1000.);
#7899=VECTOR('',#30230,1000.);
#7900=VECTOR('',#30235,1000.);
#7901=VECTOR('',#30236,1000.);
#7902=VECTOR('',#30237,1000.);
#7903=VECTOR('',#30240,1000.);
#7904=VECTOR('',#30245,1000.);
#7905=VECTOR('',#30250,1000.);
#7906=VECTOR('',#30251,1000.);
#7907=VECTOR('',#30254,1000.);
#7908=VECTOR('',#30259,1000.);
#7909=VECTOR('',#30260,1000.);
#7910=VECTOR('',#30275,1000.);
#7911=VECTOR('',#30280,1000.);
#7912=VECTOR('',#30285,1000.);
#7913=VECTOR('',#30286,1000.);
#7914=VECTOR('',#30289,1000.);
#7915=VECTOR('',#30292,1000.);
#7916=VECTOR('',#30295,1000.);
#7917=VECTOR('',#30298,1000.);
#7918=VECTOR('',#30303,1000.);
#7919=VECTOR('',#30304,1000.);
#7920=VECTOR('',#30305,1000.);
#7921=VECTOR('',#30308,1000.);
#7922=VECTOR('',#30313,1000.);
#7923=VECTOR('',#30318,1000.);
#7924=VECTOR('',#30319,1000.);
#7925=VECTOR('',#30324,1000.);
#7926=VECTOR('',#30333,1000.);
#7927=VECTOR('',#30336,1000.);
#7928=VECTOR('',#30339,1000.);
#7929=VECTOR('',#30340,1000.);
#7930=VECTOR('',#30343,1000.);
#7931=VECTOR('',#30348,1000.);
#7932=VECTOR('',#30351,1000.);
#7933=VECTOR('',#30352,1000.);
#7934=VECTOR('',#30355,1000.);
#7935=VECTOR('',#30358,1000.);
#7936=VECTOR('',#30361,1000.);
#7937=VECTOR('',#30362,1000.);
#7938=VECTOR('',#30365,1000.);
#7939=VECTOR('',#30370,1000.);
#7940=VECTOR('',#30371,1000.);
#7941=VECTOR('',#30374,1000.);
#7942=VECTOR('',#30379,1000.);
#7943=VECTOR('',#30382,1000.);
#7944=VECTOR('',#30385,1000.);
#7945=VECTOR('',#30408,2.1);
#7946=VECTOR('',#30415,2.1);
#7947=VECTOR('',#30422,2.1);
#7948=VECTOR('',#30429,2.1);
#7949=VECTOR('',#30436,2.1);
#7950=VECTOR('',#30443,2.1);
#7951=VECTOR('',#30450,14.);
#7952=VECTOR('',#30455,1000.);
#7953=VECTOR('',#30458,1000.);
#7954=VECTOR('',#30459,1000.);
#7955=VECTOR('',#30460,1000.);
#7956=VECTOR('',#30465,1000.);
#7957=VECTOR('',#30466,1000.);
#7958=VECTOR('',#30467,1000.);
#7959=VECTOR('',#30470,1000.);
#7960=VECTOR('',#30475,1000.);
#7961=VECTOR('',#30476,1000.);
#7962=VECTOR('',#30479,1000.);
#7963=VECTOR('',#30480,1000.);
#7964=VECTOR('',#30483,1000.);
#7965=VECTOR('',#30486,1000.);
#7966=VECTOR('',#30497,2.99999999999999);
#7967=VECTOR('',#30504,2.99999999999999);
#7968=VECTOR('',#30511,3.3);
#7969=VECTOR('',#30518,3.3);
#7970=VECTOR('',#30525,3.3);
#7971=VECTOR('',#30532,3.3);
#7972=VECTOR('',#30537,1000.);
#7973=VECTOR('',#30538,1000.);
#7974=VECTOR('',#30539,1000.);
#7975=VECTOR('',#30540,1000.);
#7976=VECTOR('',#30543,1000.);
#7977=VECTOR('',#30544,1000.);
#7978=VECTOR('',#30545,1000.);
#7979=VECTOR('',#30548,1000.);
#7980=VECTOR('',#30549,1000.);
#7981=VECTOR('',#30550,1000.);
#7982=VECTOR('',#30553,1000.);
#7983=VECTOR('',#30554,1000.);
#7984=VECTOR('',#30569,3.3);
#7985=VECTOR('',#30576,3.3);
#7986=VECTOR('',#30583,3.3);
#7987=VECTOR('',#30590,3.3);
#7988=VECTOR('',#30597,3.3);
#7989=VECTOR('',#30604,3.3);
#7990=VECTOR('',#30609,1000.);
#7991=VECTOR('',#30610,1000.);
#7992=VECTOR('',#30611,1000.);
#7993=VECTOR('',#30612,1000.);
#7994=VECTOR('',#30615,1000.);
#7995=VECTOR('',#30616,1000.);
#7996=VECTOR('',#30617,1000.);
#7997=VECTOR('',#30620,1000.);
#7998=VECTOR('',#30621,1000.);
#7999=VECTOR('',#30622,1000.);
#8000=VECTOR('',#30625,1000.);
#8001=VECTOR('',#30626,1000.);
#8002=VECTOR('',#30635,1000.);
#8003=VECTOR('',#30636,1000.);
#8004=VECTOR('',#30637,1000.);
#8005=VECTOR('',#30638,1000.);
#8006=VECTOR('',#30641,1000.);
#8007=VECTOR('',#30642,1000.);
#8008=VECTOR('',#30643,1000.);
#8009=VECTOR('',#30646,1000.);
#8010=VECTOR('',#30647,1000.);
#8011=VECTOR('',#30648,1000.);
#8012=VECTOR('',#30651,1000.);
#8013=VECTOR('',#30652,1000.);
#8014=VECTOR('',#30653,1000.);
#8015=VECTOR('',#30656,1000.);
#8016=VECTOR('',#30657,1000.);
#8017=VECTOR('',#30664,1000.);
#8018=VECTOR('',#30665,1000.);
#8019=VECTOR('',#30666,1000.);
#8020=VECTOR('',#30667,1000.);
#8021=VECTOR('',#30670,1000.);
#8022=VECTOR('',#30671,1000.);
#8023=VECTOR('',#30672,1000.);
#8024=VECTOR('',#30675,1000.);
#8025=VECTOR('',#30676,1000.);
#8026=VECTOR('',#30677,1000.);
#8027=VECTOR('',#30680,1000.);
#8028=VECTOR('',#30681,1000.);
#8029=VECTOR('',#30682,1000.);
#8030=VECTOR('',#30685,1000.);
#8031=VECTOR('',#30686,1000.);
#8032=VECTOR('',#30695,1000.);
#8033=VECTOR('',#30698,1000.);
#8034=VECTOR('',#30703,3.39999999999999);
#8035=VECTOR('',#30710,3.4);
#8036=VECTOR('',#30717,3.4);
#8037=VECTOR('',#30724,3.39999999999999);
#8038=VECTOR('',#30731,4.24999999999998);
#8039=VECTOR('',#30738,4.24999999999998);
#8040=VECTOR('',#30745,4.24999999999998);
#8041=VECTOR('',#30752,4.24999999999998);
#8042=VECTOR('',#30759,45.);
#8043=VECTOR('',#30766,65.);
#8044=VECTOR('',#30773,2.99999999999999);
#8045=VECTOR('',#30780,2.99999999999999);
#8046=VECTOR('',#30787,2.5);
#8047=VECTOR('',#30794,2.5);
#8048=VECTOR('',#30801,2.5);
#8049=VECTOR('',#30808,2.5);
#8050=VECTOR('',#30815,5.50000000000001);
#8051=VECTOR('',#30822,3.30000000000004);
#8052=VECTOR('',#30829,5.50000000000001);
#8053=VECTOR('',#30836,3.30000000000004);
#8054=VECTOR('',#30843,5.50000000000001);
#8055=VECTOR('',#30850,3.30000000000004);
#8056=VECTOR('',#30857,5.50000000000001);
#8057=VECTOR('',#30864,3.30000000000004);
#8058=VECTOR('',#30871,5.50000000000001);
#8059=VECTOR('',#30878,3.30000000000004);
#8060=VECTOR('',#30885,5.50000000000001);
#8061=VECTOR('',#30892,3.30000000000004);
#8062=VECTOR('',#30899,5.49999999999999);
#8063=VECTOR('',#30906,3.30000000000004);
#8064=VECTOR('',#30913,5.50000000000001);
#8065=VECTOR('',#30920,3.30000000000004);
#8066=VECTOR('',#30927,5.50000000000001);
#8067=VECTOR('',#30934,3.30000000000004);
#8068=VECTOR('',#30941,5.50000000000001);
#8069=VECTOR('',#30948,3.30000000000004);
#8070=VECTOR('',#30955,5.50000000000001);
#8071=VECTOR('',#30962,3.30000000000004);
#8072=VECTOR('',#30969,5.50000000000001);
#8073=VECTOR('',#30976,3.30000000000004);
#8074=VECTOR('',#30983,5.50000000000001);
#8075=VECTOR('',#30990,3.30000000000004);
#8076=VECTOR('',#30997,5.50000000000001);
#8077=VECTOR('',#31004,3.30000000000004);
#8078=VECTOR('',#31011,5.49999999999999);
#8079=VECTOR('',#31018,3.30000000000004);
#8080=VECTOR('',#31025,5.50000000000001);
#8081=VECTOR('',#31032,3.30000000000004);
#8082=VECTOR('',#31037,1000.);
#8083=VECTOR('',#31038,1000.);
#8084=VECTOR('',#31039,1000.);
#8085=VECTOR('',#31040,1000.);
#8086=VECTOR('',#31041,1000.);
#8087=VECTOR('',#31042,1000.);
#8088=VECTOR('',#31043,1000.);
#8089=VECTOR('',#31044,1000.);
#8090=VECTOR('',#31047,1000.);
#8091=VECTOR('',#31048,1000.);
#8092=VECTOR('',#31049,1000.);
#8093=VECTOR('',#31050,1000.);
#8094=VECTOR('',#31053,1000.);
#8095=VECTOR('',#31054,1000.);
#8096=VECTOR('',#31055,1000.);
#8097=VECTOR('',#31056,1000.);
#8098=VECTOR('',#31059,1000.);
#8099=VECTOR('',#31060,1000.);
#8100=VECTOR('',#31061,1000.);
#8101=VECTOR('',#31062,1000.);
#8102=VECTOR('',#31065,1000.);
#8103=VECTOR('',#31066,1000.);
#8104=VECTOR('',#31067,1000.);
#8105=VECTOR('',#31068,1000.);
#8106=VECTOR('',#31069,1000.);
#8107=VECTOR('',#31074,1000.);
#8108=VECTOR('',#31075,1000.);
#8109=VECTOR('',#31076,1000.);
#8110=VECTOR('',#31077,1000.);
#8111=VECTOR('',#31080,1000.);
#8112=VECTOR('',#31083,1000.);
#8113=VECTOR('',#31084,1000.);
#8114=VECTOR('',#31085,1000.);
#8115=VECTOR('',#31086,1000.);
#8116=VECTOR('',#31087,1000.);
#8117=VECTOR('',#31088,1000.);
#8118=VECTOR('',#31089,1000.);
#8119=VECTOR('',#31090,1000.);
#8120=VECTOR('',#31093,1000.);
#8121=VECTOR('',#31094,1000.);
#8122=VECTOR('',#31097,1000.);
#8123=VECTOR('',#31098,1000.);
#8124=VECTOR('',#31101,1000.);
#8125=VECTOR('',#31102,1000.);
#8126=VECTOR('',#31105,1000.);
#8127=VECTOR('',#31106,1000.);
#8128=VECTOR('',#31147,1000.);
#8129=VECTOR('',#31150,1000.);
#8130=VECTOR('',#31169,5.50000000000001);
#8131=VECTOR('',#31184,3.5);
#8132=VECTOR('',#31199,5.50000000000001);
#8133=VECTOR('',#31214,3.5);
#8134=VECTOR('',#31229,5.50000000000001);
#8135=VECTOR('',#31244,3.5);
#8136=VECTOR('',#31259,5.50000000000001);
#8137=VECTOR('',#31274,3.5);
#8138=VECTOR('',#31289,5.50000000000001);
#8139=VECTOR('',#31304,3.5);
#8140=VECTOR('',#31319,5.50000000000001);
#8141=VECTOR('',#31334,3.5);
#8142=VECTOR('',#31349,5.5);
#8143=VECTOR('',#31364,3.5);
#8144=VECTOR('',#31379,5.5);
#8145=VECTOR('',#31394,3.5);
#8146=VECTOR('',#31407,1000.);
#8147=VECTOR('',#31408,1000.);
#8148=VECTOR('',#31409,1000.);
#8149=VECTOR('',#31412,1000.);
#8150=VECTOR('',#31413,1000.);
#8151=VECTOR('',#31416,1000.);
#8152=VECTOR('',#31419,1000.);
#8153=VECTOR('',#31420,1000.);
#8154=VECTOR('',#31421,1000.);
#8155=VECTOR('',#31422,1000.);
#8156=VECTOR('',#31423,1000.);
#8157=VECTOR('',#31424,1000.);
#8158=VECTOR('',#31425,1000.);
#8159=VECTOR('',#31426,1000.);
#8160=VECTOR('',#31427,1000.);
#8161=VECTOR('',#31428,1000.);
#8162=VECTOR('',#31429,1000.);
#8163=VECTOR('',#31432,1000.);
#8164=VECTOR('',#31433,1000.);
#8165=VECTOR('',#31434,1000.);
#8166=VECTOR('',#31435,1000.);
#8167=VECTOR('',#31436,1000.);
#8168=VECTOR('',#31437,1000.);
#8169=VECTOR('',#31438,1000.);
#8170=VECTOR('',#31439,1000.);
#8171=VECTOR('',#31440,1000.);
#8172=VECTOR('',#31441,1000.);
#8173=VECTOR('',#31442,1000.);
#8174=VECTOR('',#31447,1000.);
#8175=VECTOR('',#31448,1000.);
#8176=VECTOR('',#31455,1000.);
#8177=VECTOR('',#31456,1000.);
#8178=VECTOR('',#31463,1000.);
#8179=VECTOR('',#31466,1000.);
#8180=VECTOR('',#31471,1000.);
#8181=VECTOR('',#31472,1000.);
#8182=VECTOR('',#31479,1000.);
#8183=VECTOR('',#31480,1000.);
#8184=VECTOR('',#31487,1000.);
#8185=VECTOR('',#31488,1000.);
#8186=VECTOR('',#31495,1000.);
#8187=VECTOR('',#31496,1000.);
#8188=VECTOR('',#31497,1000.);
#8189=VECTOR('',#31500,1000.);
#8190=VECTOR('',#31503,1000.);
#8191=VECTOR('',#31504,1000.);
#8192=VECTOR('',#31507,1000.);
#8193=VECTOR('',#31510,1000.);
#8194=VECTOR('',#31513,1000.);
#8195=VECTOR('',#31520,1000.);
#8196=VECTOR('',#31523,1000.);
#8197=VECTOR('',#31526,1000.);
#8198=VECTOR('',#31533,1000.);
#8199=VECTOR('',#31534,1000.);
#8200=VECTOR('',#31535,1000.);
#8201=VECTOR('',#31542,1000.);
#8202=VECTOR('',#31545,1000.);
#8203=VECTOR('',#31548,1000.);
#8204=VECTOR('',#31555,1000.);
#8205=VECTOR('',#31558,1000.);
#8206=VECTOR('',#31561,1000.);
#8207=VECTOR('',#31564,1000.);
#8208=VECTOR('',#31565,1000.);
#8209=VECTOR('',#31566,1000.);
#8210=VECTOR('',#31567,1000.);
#8211=VECTOR('',#31570,1000.);
#8212=VECTOR('',#31571,1000.);
#8213=VECTOR('',#31572,1000.);
#8214=VECTOR('',#31575,1000.);
#8215=VECTOR('',#31578,1000.);
#8216=VECTOR('',#31581,1000.);
#8217=VECTOR('',#31588,1000.);
#8218=VECTOR('',#31591,1000.);
#8219=VECTOR('',#31594,1000.);
#8220=VECTOR('',#31601,1000.);
#8221=VECTOR('',#31602,1000.);
#8222=VECTOR('',#31603,1000.);
#8223=VECTOR('',#31610,1000.);
#8224=VECTOR('',#31613,1000.);
#8225=VECTOR('',#31616,1000.);
#8226=VECTOR('',#31623,1000.);
#8227=VECTOR('',#31626,1000.);
#8228=VECTOR('',#31629,1000.);
#8229=VECTOR('',#31632,1000.);
#8230=VECTOR('',#31633,1000.);
#8231=VECTOR('',#31636,1000.);
#8232=VECTOR('',#31637,1000.);
#8233=VECTOR('',#31640,1000.);
#8234=VECTOR('',#31641,1000.);
#8235=VECTOR('',#31644,1000.);
#8236=VECTOR('',#31645,1000.);
#8237=VECTOR('',#31648,1000.);
#8238=VECTOR('',#31649,1000.);
#8239=VECTOR('',#31652,1000.);
#8240=VECTOR('',#31653,1000.);
#8241=VECTOR('',#31656,1000.);
#8242=VECTOR('',#31657,1000.);
#8243=VECTOR('',#31660,1000.);
#8244=VECTOR('',#31663,1000.);
#8245=VECTOR('',#31666,1000.);
#8246=VECTOR('',#31669,1000.);
#8247=VECTOR('',#31670,1000.);
#8248=VECTOR('',#31673,1000.);
#8249=VECTOR('',#31674,1000.);
#8250=VECTOR('',#31677,1000.);
#8251=VECTOR('',#31678,1000.);
#8252=VECTOR('',#31681,1000.);
#8253=VECTOR('',#31682,1000.);
#8254=VECTOR('',#31685,1000.);
#8255=VECTOR('',#31688,1000.);
#8256=VECTOR('',#31689,1000.);
#8257=VECTOR('',#31692,1000.);
#8258=VECTOR('',#31693,1000.);
#8259=VECTOR('',#31714,1000.);
#8260=VECTOR('',#31715,1000.);
#8261=VECTOR('',#31718,1000.);
#8262=VECTOR('',#31719,1000.);
#8263=VECTOR('',#31722,1000.);
#8264=VECTOR('',#31723,1000.);
#8265=VECTOR('',#31726,1000.);
#8266=VECTOR('',#31727,1000.);
#8267=VECTOR('',#31732,1000.);
#8268=VECTOR('',#31733,1000.);
#8269=VECTOR('',#31736,1000.);
#8270=VECTOR('',#31737,1000.);
#8271=VECTOR('',#31760,1000.);
#8272=VECTOR('',#31785,2.5);
#8273=VECTOR('',#31792,2.5);
#8274=VECTOR('',#31799,3.65);
#8275=VECTOR('',#31804,2.5);
#8276=VECTOR('',#31807,2.5);
#8277=VECTOR('',#31812,3.32349999999999);
#8278=VECTOR('',#31819,3.3235);
#8279=VECTOR('',#31826,3.32349999999999);
#8280=VECTOR('',#31833,3.3235);
#8281=VECTOR('',#31840,2.5);
#8282=VECTOR('',#31847,2.5);
#8283=VECTOR('',#31854,3.65);
#8284=VECTOR('',#31861,0.500000000000006);
#8285=VECTOR('',#31864,1000.);
#8286=VECTOR('',#31867,1000.);
#8287=VECTOR('',#31870,2.5);
#8288=VECTOR('',#31873,2.5);
#8289=VECTOR('',#31878,0.5);
#8290=VECTOR('',#31879,1000.);
#8291=VECTOR('',#31882,1000.);
#8292=VECTOR('',#31893,4.);
#8293=VECTOR('',#31898,4.99995);
#8294=VECTOR('',#31905,1000.);
#8295=VECTOR('',#31906,1000.);
#8296=VECTOR('',#31907,1000.);
#8297=VECTOR('',#31912,1000.);
#8298=VECTOR('',#31915,1000.);
#8299=VECTOR('',#31920,1000.);
#8300=VECTOR('',#31923,1000.);
#8301=VECTOR('',#31928,1000.);
#8302=VECTOR('',#31929,1000.);
#8303=VECTOR('',#31930,1000.);
#8304=VECTOR('',#31933,1000.);
#8305=VECTOR('',#31934,1000.);
#8306=VECTOR('',#31935,1000.);
#8307=VECTOR('',#31936,1000.);
#8308=VECTOR('',#31939,1000.);
#8309=VECTOR('',#31940,1000.);
#8310=VECTOR('',#31941,1000.);
#8311=VECTOR('',#31942,1000.);
#8312=VECTOR('',#31945,1000.);
#8313=VECTOR('',#31946,1000.);
#8314=VECTOR('',#31947,1000.);
#8315=VECTOR('',#31948,1000.);
#8316=VECTOR('',#31951,1000.);
#8317=VECTOR('',#31952,1000.);
#8318=VECTOR('',#31953,1000.);
#8319=VECTOR('',#31954,1000.);
#8320=VECTOR('',#31957,1000.);
#8321=VECTOR('',#31958,1000.);
#8322=VECTOR('',#31959,1000.);
#8323=VECTOR('',#31960,1000.);
#8324=VECTOR('',#31963,1000.);
#8325=VECTOR('',#31964,1000.);
#8326=VECTOR('',#31965,1000.);
#8327=VECTOR('',#31966,1000.);
#8328=VECTOR('',#31969,1000.);
#8329=VECTOR('',#31970,1000.);
#8330=VECTOR('',#31971,1000.);
#8331=VECTOR('',#31972,1000.);
#8332=VECTOR('',#31975,1000.);
#8333=VECTOR('',#31976,1000.);
#8334=VECTOR('',#31977,1000.);
#8335=VECTOR('',#31978,1000.);
#8336=VECTOR('',#31981,1000.);
#8337=VECTOR('',#31982,1000.);
#8338=VECTOR('',#31983,1000.);
#8339=VECTOR('',#31984,1000.);
#8340=VECTOR('',#31987,1000.);
#8341=VECTOR('',#31988,1000.);
#8342=VECTOR('',#31989,1000.);
#8343=VECTOR('',#31992,1000.);
#8344=VECTOR('',#31993,1000.);
#8345=VECTOR('',#31994,1000.);
#8346=VECTOR('',#31995,1000.);
#8347=VECTOR('',#31998,1000.);
#8348=VECTOR('',#31999,1000.);
#8349=VECTOR('',#32000,1000.);
#8350=VECTOR('',#32003,1000.);
#8351=VECTOR('',#32004,1000.);
#8352=VECTOR('',#32005,1000.);
#8353=VECTOR('',#32006,1000.);
#8354=VECTOR('',#32009,1000.);
#8355=VECTOR('',#32010,1000.);
#8356=VECTOR('',#32011,1000.);
#8357=VECTOR('',#32012,1000.);
#8358=VECTOR('',#32015,1000.);
#8359=VECTOR('',#32016,1000.);
#8360=VECTOR('',#32017,1000.);
#8361=VECTOR('',#32018,1000.);
#8362=VECTOR('',#32021,1000.);
#8363=VECTOR('',#32022,1000.);
#8364=VECTOR('',#32023,1000.);
#8365=VECTOR('',#32024,1000.);
#8366=VECTOR('',#32027,1000.);
#8367=VECTOR('',#32028,1000.);
#8368=VECTOR('',#32033,1000.);
#8369=VECTOR('',#32036,1000.);
#8370=VECTOR('',#32041,1000.);
#8371=VECTOR('',#32044,1000.);
#8372=VECTOR('',#32049,1000.);
#8373=VECTOR('',#32052,1000.);
#8374=VECTOR('',#32057,1000.);
#8375=VECTOR('',#32060,1000.);
#8376=VECTOR('',#32161,1000.);
#8377=VECTOR('',#32162,1000.);
#8378=VECTOR('',#32163,1000.);
#8379=VECTOR('',#32164,1000.);
#8380=VECTOR('',#32167,1000.);
#8381=VECTOR('',#32168,1000.);
#8382=VECTOR('',#32169,1000.);
#8383=VECTOR('',#32170,1000.);
#8384=VECTOR('',#32171,1000.);
#8385=VECTOR('',#32172,1000.);
#8386=VECTOR('',#32175,1000.);
#8387=VECTOR('',#32176,1000.);
#8388=VECTOR('',#32179,1000.);
#8389=VECTOR('',#32180,1000.);
#8390=VECTOR('',#32183,1000.);
#8391=VECTOR('',#32186,1000.);
#8392=VECTOR('',#32187,1000.);
#8393=VECTOR('',#32190,1000.);
#8394=VECTOR('',#32191,1000.);
#8395=VECTOR('',#32194,1000.);
#8396=VECTOR('',#32197,1000.);
#8397=VECTOR('',#32198,1000.);
#8398=VECTOR('',#32199,1000.);
#8399=VECTOR('',#32202,1000.);
#8400=VECTOR('',#32203,1000.);
#8401=VECTOR('',#32206,1000.);
#8402=VECTOR('',#32207,1000.);
#8403=VECTOR('',#32210,1000.);
#8404=VECTOR('',#32211,1000.);
#8405=VECTOR('',#32214,1000.);
#8406=VECTOR('',#32215,1000.);
#8407=VECTOR('',#32218,1000.);
#8408=VECTOR('',#32223,1000.);
#8409=VECTOR('',#32226,1000.);
#8410=VECTOR('',#32229,1000.);
#8411=VECTOR('',#32236,1000.);
#8412=VECTOR('',#32239,1000.);
#8413=VECTOR('',#32242,1000.);
#8414=VECTOR('',#32249,1000.);
#8415=VECTOR('',#32250,1000.);
#8416=VECTOR('',#32251,1000.);
#8417=VECTOR('',#32258,1000.);
#8418=VECTOR('',#32261,1000.);
#8419=VECTOR('',#32264,1000.);
#8420=VECTOR('',#32271,1000.);
#8421=VECTOR('',#32274,1000.);
#8422=VECTOR('',#32277,1000.);
#8423=VECTOR('',#32278,1000.);
#8424=VECTOR('',#32279,1000.);
#8425=VECTOR('',#32280,1000.);
#8426=VECTOR('',#32281,1000.);
#8427=VECTOR('',#32282,1000.);
#8428=VECTOR('',#32283,1000.);
#8429=VECTOR('',#32284,1000.);
#8430=VECTOR('',#32285,1000.);
#8431=VECTOR('',#32286,1000.);
#8432=VECTOR('',#32289,1000.);
#8433=VECTOR('',#32290,1000.);
#8434=VECTOR('',#32291,1000.);
#8435=VECTOR('',#32296,1000.);
#8436=VECTOR('',#32299,1000.);
#8437=VECTOR('',#32300,1000.);
#8438=VECTOR('',#32305,1000.);
#8439=VECTOR('',#32308,1000.);
#8440=VECTOR('',#32309,1000.);
#8441=VECTOR('',#32314,1000.);
#8442=VECTOR('',#32319,1000.);
#8443=VECTOR('',#32324,1000.);
#8444=VECTOR('',#32327,1000.);
#8445=VECTOR('',#32328,1000.);
#8446=VECTOR('',#32333,1000.);
#8447=VECTOR('',#32336,1000.);
#8448=VECTOR('',#32337,1000.);
#8449=VECTOR('',#32342,1000.);
#8450=VECTOR('',#32345,1000.);
#8451=VECTOR('',#32346,1000.);
#8452=VECTOR('',#32351,1000.);
#8453=VECTOR('',#32356,1000.);
#8454=VECTOR('',#32361,1000.);
#8455=VECTOR('',#32364,1000.);
#8456=VECTOR('',#32365,1000.);
#8457=VECTOR('',#32368,1000.);
#8458=VECTOR('',#32369,1000.);
#8459=VECTOR('',#32372,1000.);
#8460=VECTOR('',#32373,1000.);
#8461=VECTOR('',#32378,1000.);
#8462=VECTOR('',#32383,1000.);
#8463=VECTOR('',#32388,1000.);
#8464=VECTOR('',#32391,1000.);
#8465=VECTOR('',#32392,1000.);
#8466=VECTOR('',#32397,1000.);
#8467=VECTOR('',#32400,1000.);
#8468=VECTOR('',#32401,1000.);
#8469=VECTOR('',#32406,1000.);
#8470=VECTOR('',#32409,1000.);
#8471=VECTOR('',#32410,1000.);
#8472=VECTOR('',#32415,1000.);
#8473=VECTOR('',#32420,1000.);
#8474=VECTOR('',#32425,1000.);
#8475=VECTOR('',#32428,1000.);
#8476=VECTOR('',#32429,1000.);
#8477=VECTOR('',#32434,1000.);
#8478=VECTOR('',#32437,1000.);
#8479=VECTOR('',#32438,1000.);
#8480=VECTOR('',#32443,1000.);
#8481=VECTOR('',#32446,1000.);
#8482=VECTOR('',#32447,1000.);
#8483=VECTOR('',#32450,1000.);
#8484=VECTOR('',#32451,1000.);
#8485=VECTOR('',#32454,1000.);
#8486=VECTOR('',#32455,1000.);
#8487=VECTOR('',#32458,1000.);
#8488=VECTOR('',#32459,1000.);
#8489=VECTOR('',#32462,1000.);
#8490=VECTOR('',#32463,1000.);
#8491=VECTOR('',#32466,1000.);
#8492=VECTOR('',#32467,1000.);
#8493=VECTOR('',#32470,1000.);
#8494=VECTOR('',#32471,1000.);
#8495=VECTOR('',#32474,1000.);
#8496=VECTOR('',#32475,1000.);
#8497=VECTOR('',#32478,1000.);
#8498=VECTOR('',#32479,1000.);
#8499=VECTOR('',#32482,1000.);
#8500=VECTOR('',#32487,1000.);
#8501=VECTOR('',#32490,1000.);
#8502=VECTOR('',#32493,1000.);
#8503=VECTOR('',#32494,1000.);
#8504=VECTOR('',#32497,1000.);
#8505=VECTOR('',#32498,1000.);
#8506=VECTOR('',#32499,1000.);
#8507=VECTOR('',#32500,1000.);
#8508=VECTOR('',#32501,1000.);
#8509=VECTOR('',#32502,1000.);
#8510=VECTOR('',#32503,1000.);
#8511=VECTOR('',#32506,1000.);
#8512=VECTOR('',#32509,1000.);
#8513=VECTOR('',#32516,1000.);
#8514=VECTOR('',#32519,1000.);
#8515=VECTOR('',#32522,1000.);
#8516=VECTOR('',#32529,1000.);
#8517=VECTOR('',#32530,1000.);
#8518=VECTOR('',#32531,1000.);
#8519=VECTOR('',#32538,1000.);
#8520=VECTOR('',#32541,1000.);
#8521=VECTOR('',#32544,1000.);
#8522=VECTOR('',#32551,1000.);
#8523=VECTOR('',#32554,1000.);
#8524=VECTOR('',#32557,1000.);
#8525=VECTOR('',#32558,1000.);
#8526=VECTOR('',#32559,1000.);
#8527=VECTOR('',#32560,1000.);
#8528=VECTOR('',#32561,1000.);
#8529=VECTOR('',#32564,1000.);
#8530=VECTOR('',#32565,1000.);
#8531=VECTOR('',#32568,1000.);
#8532=VECTOR('',#32569,1000.);
#8533=VECTOR('',#32578,1000.);
#8534=VECTOR('',#32581,1000.);
#8535=VECTOR('',#32584,1000.);
#8536=VECTOR('',#32585,1000.);
#8537=VECTOR('',#32586,1000.);
#8538=VECTOR('',#32589,1000.);
#8539=VECTOR('',#32590,1000.);
#8540=VECTOR('',#32593,1000.);
#8541=VECTOR('',#32594,1000.);
#8542=VECTOR('',#32597,1000.);
#8543=VECTOR('',#32598,1000.);
#8544=VECTOR('',#32601,1000.);
#8545=VECTOR('',#32602,1000.);
#8546=VECTOR('',#32603,1000.);
#8547=VECTOR('',#32604,1000.);
#8548=VECTOR('',#32605,1000.);
#8549=VECTOR('',#32608,1000.);
#8550=VECTOR('',#32609,1000.);
#8551=VECTOR('',#32612,1000.);
#8552=VECTOR('',#32613,1000.);
#8553=VECTOR('',#32616,1000.);
#8554=VECTOR('',#32617,1000.);
#8555=VECTOR('',#32620,1000.);
#8556=VECTOR('',#32621,1000.);
#8557=VECTOR('',#32624,1000.);
#8558=VECTOR('',#32625,1000.);
#8559=VECTOR('',#32630,1000.);
#8560=VECTOR('',#32633,1000.);
#8561=VECTOR('',#32634,1000.);
#8562=VECTOR('',#32639,1000.);
#8563=VECTOR('',#32642,1000.);
#8564=VECTOR('',#32643,1000.);
#8565=VECTOR('',#32648,1000.);
#8566=VECTOR('',#32653,1000.);
#8567=VECTOR('',#32658,1000.);
#8568=VECTOR('',#32661,1000.);
#8569=VECTOR('',#32662,1000.);
#8570=VECTOR('',#32667,1000.);
#8571=VECTOR('',#32670,1000.);
#8572=VECTOR('',#32671,1000.);
#8573=VECTOR('',#32676,1000.);
#8574=VECTOR('',#32679,1000.);
#8575=VECTOR('',#32680,1000.);
#8576=VECTOR('',#32685,1000.);
#8577=VECTOR('',#32690,1000.);
#8578=VECTOR('',#32695,1000.);
#8579=VECTOR('',#32698,1000.);
#8580=VECTOR('',#32699,1000.);
#8581=VECTOR('',#32702,1000.);
#8582=VECTOR('',#32703,1000.);
#8583=VECTOR('',#32706,1000.);
#8584=VECTOR('',#32707,1000.);
#8585=VECTOR('',#32712,1000.);
#8586=VECTOR('',#32717,1000.);
#8587=VECTOR('',#32722,1000.);
#8588=VECTOR('',#32725,1000.);
#8589=VECTOR('',#32726,1000.);
#8590=VECTOR('',#32731,1000.);
#8591=VECTOR('',#32734,1000.);
#8592=VECTOR('',#32735,1000.);
#8593=VECTOR('',#32740,1000.);
#8594=VECTOR('',#32743,1000.);
#8595=VECTOR('',#32744,1000.);
#8596=VECTOR('',#32749,1000.);
#8597=VECTOR('',#32754,1000.);
#8598=VECTOR('',#32759,1000.);
#8599=VECTOR('',#32762,1000.);
#8600=VECTOR('',#32763,1000.);
#8601=VECTOR('',#32768,1000.);
#8602=VECTOR('',#32771,1000.);
#8603=VECTOR('',#32772,1000.);
#8604=VECTOR('',#32777,1000.);
#8605=VECTOR('',#32780,1000.);
#8606=VECTOR('',#32785,1000.);
#8607=VECTOR('',#32786,1000.);
#8608=VECTOR('',#32787,1000.);
#8609=VECTOR('',#32788,1000.);
#8610=VECTOR('',#32791,1000.);
#8611=VECTOR('',#32792,1000.);
#8612=VECTOR('',#32793,1000.);
#8613=VECTOR('',#32794,1000.);
#8614=VECTOR('',#32797,1000.);
#8615=VECTOR('',#32798,1000.);
#8616=VECTOR('',#32801,1000.);
#8617=VECTOR('',#32802,1000.);
#8618=VECTOR('',#32813,1000.);
#8619=VECTOR('',#32816,1000.);
#8620=VECTOR('',#32817,1000.);
#8621=VECTOR('',#32818,1000.);
#8622=VECTOR('',#32819,1000.);
#8623=VECTOR('',#32822,1000.);
#8624=VECTOR('',#32823,1000.);
#8625=VECTOR('',#32824,1000.);
#8626=VECTOR('',#32827,1000.);
#8627=VECTOR('',#32828,1000.);
#8628=VECTOR('',#32829,1000.);
#8629=VECTOR('',#32830,1000.);
#8630=VECTOR('',#32833,1000.);
#8631=VECTOR('',#32836,1000.);
#8632=VECTOR('',#32837,1000.);
#8633=VECTOR('',#32840,1000.);
#8634=VECTOR('',#32845,1000.);
#8635=VECTOR('',#32846,1000.);
#8636=VECTOR('',#32847,1000.);
#8637=VECTOR('',#32848,1000.);
#8638=VECTOR('',#32849,1000.);
#8639=VECTOR('',#32850,1000.);
#8640=VECTOR('',#32851,1000.);
#8641=VECTOR('',#32852,1000.);
#8642=VECTOR('',#32853,1000.);
#8643=VECTOR('',#32854,1000.);
#8644=VECTOR('',#32857,1000.);
#8645=VECTOR('',#32860,1000.);
#8646=VECTOR('',#32867,1000.);
#8647=VECTOR('',#32870,1000.);
#8648=VECTOR('',#32873,1000.);
#8649=VECTOR('',#32880,1000.);
#8650=VECTOR('',#32881,1000.);
#8651=VECTOR('',#32882,1000.);
#8652=VECTOR('',#32889,1000.);
#8653=VECTOR('',#32892,1000.);
#8654=VECTOR('',#32895,1000.);
#8655=VECTOR('',#32902,1000.);
#8656=VECTOR('',#32905,1000.);
#8657=VECTOR('',#32908,1000.);
#8658=VECTOR('',#32911,1000.);
#8659=VECTOR('',#32912,1000.);
#8660=VECTOR('',#32915,1000.);
#8661=VECTOR('',#32916,1000.);
#8662=VECTOR('',#32919,1000.);
#8663=VECTOR('',#32920,1000.);
#8664=VECTOR('',#32921,1000.);
#8665=VECTOR('',#32924,1000.);
#8666=VECTOR('',#32925,1000.);
#8667=VECTOR('',#32926,1000.);
#8668=VECTOR('',#32929,1000.);
#8669=VECTOR('',#32930,1000.);
#8670=VECTOR('',#32931,1000.);
#8671=VECTOR('',#32934,1000.);
#8672=VECTOR('',#32935,1000.);
#8673=VECTOR('',#32936,1000.);
#8674=VECTOR('',#32949,1000.);
#8675=VECTOR('',#32950,1000.);
#8676=VECTOR('',#32951,1000.);
#8677=VECTOR('',#32954,1000.);
#8678=VECTOR('',#32955,1000.);
#8679=VECTOR('',#32956,1000.);
#8680=VECTOR('',#32961,1000.);
#8681=VECTOR('',#32962,1000.);
#8682=VECTOR('',#32965,1000.);
#8683=VECTOR('',#32966,1000.);
#8684=VECTOR('',#32967,1000.);
#8685=VECTOR('',#32970,1000.);
#8686=VECTOR('',#32971,1000.);
#8687=VECTOR('',#32978,1000.);
#8688=VECTOR('',#32979,1000.);
#8689=VECTOR('',#32988,1000.);
#8690=VECTOR('',#32989,1000.);
#8691=VECTOR('',#32990,1000.);
#8692=VECTOR('',#32993,1000.);
#8693=VECTOR('',#32994,1000.);
#8694=VECTOR('',#32997,1000.);
#8695=VECTOR('',#32998,1000.);
#8696=VECTOR('',#33001,1000.);
#8697=VECTOR('',#33002,1000.);
#8698=VECTOR('',#33005,1000.);
#8699=VECTOR('',#33006,1000.);
#8700=VECTOR('',#33009,1000.);
#8701=VECTOR('',#33010,1000.);
#8702=VECTOR('',#33013,1000.);
#8703=VECTOR('',#33014,1000.);
#8704=VECTOR('',#33017,1000.);
#8705=VECTOR('',#33018,1000.);
#8706=VECTOR('',#33021,1000.);
#8707=VECTOR('',#33022,1000.);
#8708=VECTOR('',#33025,1000.);
#8709=VECTOR('',#33026,1000.);
#8710=VECTOR('',#33031,1000.);
#8711=VECTOR('',#33034,1000.);
#8712=VECTOR('',#33035,1000.);
#8713=VECTOR('',#33040,1000.);
#8714=VECTOR('',#33043,1000.);
#8715=VECTOR('',#33044,1000.);
#8716=VECTOR('',#33049,1000.);
#8717=VECTOR('',#33054,1000.);
#8718=VECTOR('',#33059,1000.);
#8719=VECTOR('',#33062,1000.);
#8720=VECTOR('',#33063,1000.);
#8721=VECTOR('',#33068,1000.);
#8722=VECTOR('',#33071,1000.);
#8723=VECTOR('',#33072,1000.);
#8724=VECTOR('',#33077,1000.);
#8725=VECTOR('',#33080,1000.);
#8726=VECTOR('',#33081,1000.);
#8727=VECTOR('',#33086,1000.);
#8728=VECTOR('',#33091,1000.);
#8729=VECTOR('',#33096,1000.);
#8730=VECTOR('',#33099,1000.);
#8731=VECTOR('',#33100,1000.);
#8732=VECTOR('',#33103,1000.);
#8733=VECTOR('',#33104,1000.);
#8734=VECTOR('',#33107,1000.);
#8735=VECTOR('',#33108,1000.);
#8736=VECTOR('',#33113,1000.);
#8737=VECTOR('',#33118,1000.);
#8738=VECTOR('',#33123,1000.);
#8739=VECTOR('',#33126,1000.);
#8740=VECTOR('',#33127,1000.);
#8741=VECTOR('',#33132,1000.);
#8742=VECTOR('',#33135,1000.);
#8743=VECTOR('',#33136,1000.);
#8744=VECTOR('',#33141,1000.);
#8745=VECTOR('',#33144,1000.);
#8746=VECTOR('',#33145,1000.);
#8747=VECTOR('',#33150,1000.);
#8748=VECTOR('',#33155,1000.);
#8749=VECTOR('',#33160,1000.);
#8750=VECTOR('',#33163,1000.);
#8751=VECTOR('',#33164,1000.);
#8752=VECTOR('',#33169,1000.);
#8753=VECTOR('',#33172,1000.);
#8754=VECTOR('',#33173,1000.);
#8755=VECTOR('',#33178,1000.);
#8756=VECTOR('',#33181,1000.);
#8757=VECTOR('',#33184,1000.);
#8758=VECTOR('',#33185,1000.);
#8759=VECTOR('',#33186,1000.);
#8760=VECTOR('',#33187,1000.);
#8761=VECTOR('',#33190,1000.);
#8762=VECTOR('',#33191,1000.);
#8763=VECTOR('',#33192,1000.);
#8764=VECTOR('',#33195,1000.);
#8765=VECTOR('',#33196,1000.);
#8766=VECTOR('',#33197,1000.);
#8767=VECTOR('',#33200,1000.);
#8768=VECTOR('',#33201,1000.);
#8769=VECTOR('',#33202,1000.);
#8770=VECTOR('',#33205,1000.);
#8771=VECTOR('',#33206,1000.);
#8772=VECTOR('',#33207,1000.);
#8773=VECTOR('',#33210,1000.);
#8774=VECTOR('',#33211,1000.);
#8775=VECTOR('',#33212,1000.);
#8776=VECTOR('',#33213,1000.);
#8777=VECTOR('',#33216,1000.);
#8778=VECTOR('',#33217,1000.);
#8779=VECTOR('',#33218,1000.);
#8780=VECTOR('',#33221,1000.);
#8781=VECTOR('',#33222,1000.);
#8782=VECTOR('',#33223,1000.);
#8783=VECTOR('',#33226,1000.);
#8784=VECTOR('',#33227,1000.);
#8785=VECTOR('',#33230,1000.);
#8786=VECTOR('',#33231,1000.);
#8787=VECTOR('',#33232,1000.);
#8788=VECTOR('',#33233,1000.);
#8789=VECTOR('',#33236,1000.);
#8790=VECTOR('',#33237,1000.);
#8791=VECTOR('',#33238,1000.);
#8792=VECTOR('',#33241,1000.);
#8793=VECTOR('',#33242,1000.);
#8794=VECTOR('',#33243,1000.);
#8795=VECTOR('',#33246,1000.);
#8796=VECTOR('',#33247,1000.);
#8797=VECTOR('',#33248,1000.);
#8798=VECTOR('',#33251,1000.);
#8799=VECTOR('',#33252,1000.);
#8800=VECTOR('',#33253,1000.);
#8801=VECTOR('',#33256,1000.);
#8802=VECTOR('',#33257,1000.);
#8803=VECTOR('',#33258,1000.);
#8804=VECTOR('',#33261,1000.);
#8805=VECTOR('',#33262,1000.);
#8806=VECTOR('',#33263,1000.);
#8807=VECTOR('',#33266,1000.);
#8808=VECTOR('',#33267,1000.);
#8809=VECTOR('',#33268,1000.);
#8810=VECTOR('',#33271,1000.);
#8811=VECTOR('',#33272,1000.);
#8812=VECTOR('',#33273,1000.);
#8813=VECTOR('',#33276,1000.);
#8814=VECTOR('',#33277,1000.);
#8815=VECTOR('',#33278,1000.);
#8816=VECTOR('',#33281,1000.);
#8817=VECTOR('',#33282,1000.);
#8818=VECTOR('',#33283,1000.);
#8819=VECTOR('',#33286,1000.);
#8820=VECTOR('',#33287,1000.);
#8821=VECTOR('',#33288,1000.);
#8822=VECTOR('',#33291,1000.);
#8823=VECTOR('',#33292,1000.);
#8824=VECTOR('',#33293,1000.);
#8825=VECTOR('',#33296,1000.);
#8826=VECTOR('',#33297,1000.);
#8827=VECTOR('',#33298,1000.);
#8828=VECTOR('',#33301,1000.);
#8829=VECTOR('',#33302,1000.);
#8830=VECTOR('',#33303,1000.);
#8831=VECTOR('',#33308,1000.);
#8832=VECTOR('',#33309,1000.);
#8833=VECTOR('',#33312,1000.);
#8834=VECTOR('',#33313,1000.);
#8835=VECTOR('',#33314,1000.);
#8836=VECTOR('',#33319,1000.);
#8837=VECTOR('',#33320,1000.);
#8838=VECTOR('',#33325,1000.);
#8839=VECTOR('',#33326,1000.);
#8840=VECTOR('',#33329,1000.);
#8841=VECTOR('',#33330,1000.);
#8842=VECTOR('',#33331,1000.);
#8843=VECTOR('',#33334,1000.);
#8844=VECTOR('',#33341,1000.);
#8845=VECTOR('',#33342,1000.);
#8846=VECTOR('',#33345,1000.);
#8847=VECTOR('',#33346,1000.);
#8848=VECTOR('',#33347,1000.);
#8849=VECTOR('',#33350,1000.);
#8850=VECTOR('',#33351,1000.);
#8851=VECTOR('',#33352,1000.);
#8852=VECTOR('',#33355,1000.);
#8853=VECTOR('',#33356,1000.);
#8854=VECTOR('',#33357,1000.);
#8855=VECTOR('',#33362,1000.);
#8856=VECTOR('',#33365,1000.);
#8857=VECTOR('',#33366,1000.);
#8858=VECTOR('',#33369,1000.);
#8859=VECTOR('',#33372,1000.);
#8860=VECTOR('',#33379,1000.);
#8861=VECTOR('',#33382,1000.);
#8862=VECTOR('',#33385,1000.);
#8863=VECTOR('',#33392,1000.);
#8864=VECTOR('',#33393,1000.);
#8865=VECTOR('',#33394,1000.);
#8866=VECTOR('',#33401,1000.);
#8867=VECTOR('',#33404,1000.);
#8868=VECTOR('',#33407,1000.);
#8869=VECTOR('',#33414,1000.);
#8870=VECTOR('',#33417,1000.);
#8871=VECTOR('',#33420,1000.);
#8872=VECTOR('',#33421,1000.);
#8873=VECTOR('',#33424,1000.);
#8874=VECTOR('',#33425,1000.);
#8875=VECTOR('',#33426,1000.);
#8876=VECTOR('',#33427,1000.);
#8877=VECTOR('',#33428,1000.);
#8878=VECTOR('',#33429,1000.);
#8879=VECTOR('',#33430,1000.);
#8880=VECTOR('',#33431,1000.);
#8881=VECTOR('',#33432,1000.);
#8882=VECTOR('',#33433,1000.);
#8883=VECTOR('',#33434,1000.);
#8884=VECTOR('',#33435,1000.);
#8885=VECTOR('',#33436,1000.);
#8886=VECTOR('',#33439,1000.);
#8887=VECTOR('',#33440,1000.);
#8888=VECTOR('',#33441,1000.);
#8889=VECTOR('',#33444,1000.);
#8890=VECTOR('',#33445,1000.);
#8891=VECTOR('',#33446,1000.);
#8892=VECTOR('',#33449,1000.);
#8893=VECTOR('',#33450,1000.);
#8894=VECTOR('',#33453,1000.);
#8895=VECTOR('',#33454,1000.);
#8896=VECTOR('',#33457,1000.);
#8897=VECTOR('',#33458,1000.);
#8898=VECTOR('',#33461,1000.);
#8899=VECTOR('',#33464,1000.);
#8900=VECTOR('',#33467,1000.);
#8901=VECTOR('',#33470,1000.);
#8902=VECTOR('',#33473,1000.);
#8903=VECTOR('',#33476,1000.);
#8904=VECTOR('',#33477,1000.);
#8905=VECTOR('',#33480,1000.);
#8906=VECTOR('',#33485,1000.);
#8907=VECTOR('',#33486,1000.);
#8908=VECTOR('',#33491,1000.);
#8909=VECTOR('',#33492,1000.);
#8910=VECTOR('',#33501,1000.);
#8911=VECTOR('',#33502,1000.);
#8912=VECTOR('',#33507,1000.);
#8913=VECTOR('',#33508,1000.);
#8914=VECTOR('',#33511,1000.);
#8915=VECTOR('',#33514,1000.);
#8916=VECTOR('',#33519,1000.);
#8917=VECTOR('',#33520,1000.);
#8918=VECTOR('',#33525,1000.);
#8919=VECTOR('',#33526,1000.);
#8920=VECTOR('',#33533,1000.);
#8921=VECTOR('',#33534,1000.);
#8922=VECTOR('',#33535,1000.);
#8923=VECTOR('',#33538,1000.);
#8924=VECTOR('',#33543,1000.);
#8925=VECTOR('',#33544,1000.);
#8926=VECTOR('',#33549,1000.);
#8927=VECTOR('',#33550,1000.);
#8928=VECTOR('',#33559,1000.);
#8929=VECTOR('',#33560,1000.);
#8930=VECTOR('',#33565,1000.);
#8931=VECTOR('',#33566,1000.);
#8932=VECTOR('',#33569,1000.);
#8933=VECTOR('',#33572,1000.);
#8934=VECTOR('',#33575,1000.);
#8935=VECTOR('',#33580,1000.);
#8936=VECTOR('',#33581,1000.);
#8937=VECTOR('',#33586,1000.);
#8938=VECTOR('',#33587,1000.);
#8939=VECTOR('',#33594,1000.);
#8940=VECTOR('',#33597,1000.);
#8941=VECTOR('',#33600,1000.);
#8942=VECTOR('',#33603,1000.);
#8943=VECTOR('',#33606,1000.);
#8944=VECTOR('',#33607,1000.);
#8945=VECTOR('',#33608,1000.);
#8946=VECTOR('',#33611,1000.);
#8947=VECTOR('',#33612,1000.);
#8948=VECTOR('',#33615,1000.);
#8949=VECTOR('',#33616,1000.);
#8950=VECTOR('',#33619,1000.);
#8951=VECTOR('',#33622,1000.);
#8952=VECTOR('',#33623,1000.);
#8953=VECTOR('',#33626,1000.);
#8954=VECTOR('',#33629,1000.);
#8955=VECTOR('',#33632,1000.);
#8956=VECTOR('',#33635,1000.);
#8957=VECTOR('',#33638,1000.);
#8958=VECTOR('',#33641,1000.);
#8959=VECTOR('',#33644,1000.);
#8960=VECTOR('',#33645,1000.);
#8961=VECTOR('',#33648,1000.);
#8962=VECTOR('',#33653,1000.);
#8963=VECTOR('',#33654,1000.);
#8964=VECTOR('',#33659,1000.);
#8965=VECTOR('',#33662,1000.);
#8966=VECTOR('',#33689,2.5);
#8967=VECTOR('',#33708,3.);
#8968=VECTOR('',#33719,4.);
#8969=VECTOR('',#33762,1000.);
#8970=VECTOR('',#33763,1000.);
#8971=VECTOR('',#33766,1000.);
#8972=VECTOR('',#33767,1000.);
#8973=VECTOR('',#33770,1000.);
#8974=VECTOR('',#33771,1000.);
#8975=VECTOR('',#33774,1000.);
#8976=VECTOR('',#33775,1000.);
#8977=VECTOR('',#33778,1000.);
#8978=VECTOR('',#33779,1000.);
#8979=VECTOR('',#33782,1000.);
#8980=VECTOR('',#33783,1000.);
#8981=VECTOR('',#33786,1000.);
#8982=VECTOR('',#33787,1000.);
#8983=VECTOR('',#33788,1000.);
#8984=VECTOR('',#33791,1000.);
#8985=VECTOR('',#33792,1000.);
#8986=VECTOR('',#33795,1000.);
#8987=VECTOR('',#33796,1000.);
#8988=VECTOR('',#33799,1000.);
#8989=VECTOR('',#33800,1000.);
#8990=VECTOR('',#33803,1000.);
#8991=VECTOR('',#33804,1000.);
#8992=VECTOR('',#33807,1000.);
#8993=VECTOR('',#33832,1000.);
#8994=VECTOR('',#33833,1000.);
#8995=VECTOR('',#33836,1000.);
#8996=VECTOR('',#33839,1000.);
#8997=VECTOR('',#33842,1000.);
#8998=VECTOR('',#33845,1000.);
#8999=VECTOR('',#33876,2.5);
#9000=VECTOR('',#33881,2.5);
#9001=VECTOR('',#33886,2.5);
#9002=VECTOR('',#33891,2.5);
#9003=VECTOR('',#33896,2.5);
#9004=VECTOR('',#33901,2.5);
#9005=VECTOR('',#33906,2.5);
#9006=VECTOR('',#33911,2.5);
#9007=VECTOR('',#33916,2.5);
#9008=VECTOR('',#33921,2.5);
#9009=VECTOR('',#33926,2.5);
#9010=VECTOR('',#33931,2.5);
#9011=VECTOR('',#33936,2.5);
#9012=VECTOR('',#33941,2.5);
#9013=VECTOR('',#33946,2.5);
#9014=VECTOR('',#33951,2.5);
#9015=VECTOR('',#33954,1000.);
#9016=VECTOR('',#33955,1000.);
#9017=VECTOR('',#33956,1000.);
#9018=VECTOR('',#33957,1000.);
#9019=VECTOR('',#33960,1000.);
#9020=VECTOR('',#33963,1000.);
#9021=VECTOR('',#33966,1000.);
#9022=VECTOR('',#33967,1000.);
#9023=VECTOR('',#33968,1000.);
#9024=VECTOR('',#33969,1000.);
#9025=VECTOR('',#33970,1000.);
#9026=VECTOR('',#33973,1000.);
#9027=VECTOR('',#33974,1000.);
#9028=VECTOR('',#33975,1000.);
#9029=VECTOR('',#33978,1000.);
#9030=VECTOR('',#33981,1000.);
#9031=VECTOR('',#33984,1000.);
#9032=VECTOR('',#33985,1000.);
#9033=VECTOR('',#33986,1000.);
#9034=VECTOR('',#33987,1000.);
#9035=VECTOR('',#33990,1000.);
#9036=VECTOR('',#33991,1000.);
#9037=VECTOR('',#33998,1000.);
#9038=VECTOR('',#34001,1000.);
#9039=VECTOR('',#34002,1000.);
#9040=VECTOR('',#34005,1000.);
#9041=VECTOR('',#34018,3.75);
#9042=VECTOR('',#34023,1664.2794823505);
#9043=VECTOR('',#34040,4.25);
#9044=VECTOR('',#34047,2.065);
#9045=VECTOR('',#34054,2.5);
#9046=VECTOR('',#34059,1000.);
#9047=VECTOR('',#34060,1000.);
#9048=VECTOR('',#34061,1000.);
#9049=VECTOR('',#34062,1000.);
#9050=VECTOR('',#34063,1000.);
#9051=VECTOR('',#34064,1000.);
#9052=VECTOR('',#34073,1000.);
#9053=VECTOR('',#34074,1000.);
#9054=VECTOR('',#34075,1000.);
#9055=VECTOR('',#34076,1000.);
#9056=VECTOR('',#34079,1000.);
#9057=VECTOR('',#34080,1000.);
#9058=VECTOR('',#34081,1000.);
#9059=VECTOR('',#34084,1000.);
#9060=VECTOR('',#34085,1000.);
#9061=VECTOR('',#34086,1000.);
#9062=VECTOR('',#34089,1000.);
#9063=VECTOR('',#34090,1000.);
#9064=VECTOR('',#34091,1000.);
#9065=VECTOR('',#34094,1000.);
#9066=VECTOR('',#34095,1000.);
#9067=VECTOR('',#34096,1000.);
#9068=VECTOR('',#34099,1000.);
#9069=VECTOR('',#34100,1000.);
#9070=VECTOR('',#34117,5.);
#9071=VECTOR('',#34124,2.5);
#9072=VECTOR('',#34135,1000.);
#9073=VECTOR('',#34138,1000.);
#9074=VECTOR('',#34143,1000.);
#9075=VECTOR('',#34146,1000.);
#9076=VECTOR('',#34149,1000.);
#9077=VECTOR('',#34150,1000.);
#9078=VECTOR('',#34153,1000.);
#9079=VECTOR('',#34154,1000.);
#9080=VECTOR('',#34165,5.);
#9081=VECTOR('',#34170,5.);
#9082=VECTOR('',#34177,2.4585);
#9083=VECTOR('',#34184,3.);
#9084=VECTOR('',#34191,1000.);
#9085=VECTOR('',#34192,1000.);
#9086=VECTOR('',#34193,1000.);
#9087=VECTOR('',#34194,1000.);
#9088=VECTOR('',#34195,1000.);
#9089=VECTOR('',#34196,1000.);
#9090=VECTOR('',#34201,1000.);
#9091=VECTOR('',#34202,1000.);
#9092=VECTOR('',#34203,1000.);
#9093=VECTOR('',#34206,1000.);
#9094=VECTOR('',#34207,1000.);
#9095=VECTOR('',#34210,1000.);
#9096=VECTOR('',#34211,1000.);
#9097=VECTOR('',#34214,1000.);
#9098=VECTOR('',#34215,1000.);
#9099=VECTOR('',#34218,1000.);
#9100=VECTOR('',#34219,1000.);
#9101=VECTOR('',#34222,1000.);
#9102=VECTOR('',#34233,5.7);
#9103=VECTOR('',#34238,1664.2794823505);
#9104=VECTOR('',#34255,6.5);
#9105=VECTOR('',#34262,3.3225);
#9106=VECTOR('',#34269,4.);
#9107=VECTOR('',#34274,1000.);
#9108=VECTOR('',#34275,1000.);
#9109=VECTOR('',#34276,1000.);
#9110=VECTOR('',#34277,1000.);
#9111=VECTOR('',#34278,1000.);
#9112=VECTOR('',#34279,1000.);
#9113=VECTOR('',#34288,1000.);
#9114=VECTOR('',#34289,1000.);
#9115=VECTOR('',#34290,1000.);
#9116=VECTOR('',#34291,1000.);
#9117=VECTOR('',#34294,1000.);
#9118=VECTOR('',#34295,1000.);
#9119=VECTOR('',#34296,1000.);
#9120=VECTOR('',#34299,1000.);
#9121=VECTOR('',#34300,1000.);
#9122=VECTOR('',#34301,1000.);
#9123=VECTOR('',#34304,1000.);
#9124=VECTOR('',#34305,1000.);
#9125=VECTOR('',#34306,1000.);
#9126=VECTOR('',#34309,1000.);
#9127=VECTOR('',#34310,1000.);
#9128=VECTOR('',#34311,1000.);
#9129=VECTOR('',#34314,1000.);
#9130=VECTOR('',#34315,1000.);
#9131=VECTOR('',#34332,8.);
#9132=VECTOR('',#34339,4.);
#9133=VECTOR('',#34350,1000.);
#9134=VECTOR('',#34353,1000.);
#9135=VECTOR('',#34358,1000.);
#9136=VECTOR('',#34361,1000.);
#9137=VECTOR('',#34364,1000.);
#9138=VECTOR('',#34365,1000.);
#9139=VECTOR('',#34368,1000.);
#9140=VECTOR('',#34369,1000.);
#9141=VECTOR('',#34380,5.);
#9142=VECTOR('',#34385,5.);
#9143=VECTOR('',#34392,2.4585);
#9144=VECTOR('',#34399,3.);
#9145=VECTOR('',#34406,1000.);
#9146=VECTOR('',#34407,1000.);
#9147=VECTOR('',#34408,1000.);
#9148=VECTOR('',#34409,1000.);
#9149=VECTOR('',#34410,1000.);
#9150=VECTOR('',#34411,1000.);
#9151=VECTOR('',#34416,1000.);
#9152=VECTOR('',#34417,1000.);
#9153=VECTOR('',#34418,1000.);
#9154=VECTOR('',#34421,1000.);
#9155=VECTOR('',#34422,1000.);
#9156=VECTOR('',#34425,1000.);
#9157=VECTOR('',#34426,1000.);
#9158=VECTOR('',#34429,1000.);
#9159=VECTOR('',#34430,1000.);
#9160=VECTOR('',#34433,1000.);
#9161=VECTOR('',#34434,1000.);
#9162=VECTOR('',#34437,1000.);
#9163=VECTOR('',#34446,3.5);
#9164=VECTOR('',#34451,3.5);
#9165=VECTOR('',#34458,1.621);
#9166=VECTOR('',#34465,2.);
#9167=VECTOR('',#34472,1000.);
#9168=VECTOR('',#34473,1000.);
#9169=VECTOR('',#34474,1000.);
#9170=VECTOR('',#34475,1000.);
#9171=VECTOR('',#34476,1000.);
#9172=VECTOR('',#34477,1000.);
#9173=VECTOR('',#34482,1000.);
#9174=VECTOR('',#34483,1000.);
#9175=VECTOR('',#34484,1000.);
#9176=VECTOR('',#34487,1000.);
#9177=VECTOR('',#34488,1000.);
#9178=VECTOR('',#34491,1000.);
#9179=VECTOR('',#34492,1000.);
#9180=VECTOR('',#34495,1000.);
#9181=VECTOR('',#34496,1000.);
#9182=VECTOR('',#34499,1000.);
#9183=VECTOR('',#34500,1000.);
#9184=VECTOR('',#34503,1000.);
#9185=CIRCLE('',#24886,3.);
#9186=CIRCLE('',#24887,3.);
#9187=CIRCLE('',#24889,3.);
#9188=CIRCLE('',#24890,3.);
#9189=CIRCLE('',#24892,3.);
#9190=CIRCLE('',#24893,3.);
#9191=CIRCLE('',#24895,3.);
#9192=CIRCLE('',#24896,3.);
#9193=CIRCLE('',#24898,3.4);
#9194=CIRCLE('',#24899,3.4);
#9195=CIRCLE('',#24901,3.4);
#9196=CIRCLE('',#24902,3.4);
#9197=CIRCLE('',#24904,3.4);
#9198=CIRCLE('',#24905,3.4);
#9199=CIRCLE('',#24907,3.4);
#9200=CIRCLE('',#24908,3.4);
#9201=CIRCLE('',#24910,3.);
#9202=CIRCLE('',#24911,3.);
#9203=CIRCLE('',#24914,3.);
#9204=CIRCLE('',#24915,3.);
#9205=CIRCLE('',#24918,2.49999999999999);
#9206=CIRCLE('',#24919,2.49999999999999);
#9207=CIRCLE('',#24922,2.49999999999999);
#9208=CIRCLE('',#24923,2.49999999999999);
#9209=CIRCLE('',#24939,5.0000000000001);
#9210=CIRCLE('',#24940,5.00000000000007);
#9211=CIRCLE('',#24941,5.00000000000007);
#9212=CIRCLE('',#24943,5.2000000000001);
#9213=CIRCLE('',#24944,0.199999999999989);
#9214=CIRCLE('',#24946,6.00000000000009);
#9215=CIRCLE('',#24947,5.50000000000001);
#9216=CIRCLE('',#24949,6.00000000000001);
#9217=CIRCLE('',#24951,6.30000000000001);
#9218=CIRCLE('',#24952,0.300000000000011);
#9219=CIRCLE('',#24954,7.50000000000009);
#9220=CIRCLE('',#24955,7.00000000000006);
#9221=CIRCLE('',#24957,7.49999999999999);
#9222=CIRCLE('',#24958,7.49999999999999);
#9223=CIRCLE('',#24960,7.00000000000002);
#9224=CIRCLE('',#24962,5.);
#9225=CIRCLE('',#24963,0.3);
#9226=CIRCLE('',#24964,5.3);
#9227=CIRCLE('',#24966,5.);
#9228=CIRCLE('',#24968,4.8);
#9229=CIRCLE('',#24969,4.8);
#9230=CIRCLE('',#24971,5.);
#9231=CIRCLE('',#24972,5.);
#9232=CIRCLE('',#24973,5.);
#9233=CIRCLE('',#24975,4.50000000000003);
#9234=CIRCLE('',#24982,4.50000000000006);
#9235=CIRCLE('',#24988,1.5);
#9236=CIRCLE('',#24993,2.74999999999999);
#9237=CIRCLE('',#24994,2.75);
#9238=CIRCLE('',#24996,2.74999999999999);
#9239=CIRCLE('',#24997,2.75);
#9240=CIRCLE('',#24999,2.74999999999999);
#9241=CIRCLE('',#25000,2.75);
#9242=CIRCLE('',#25002,2.74999999999999);
#9243=CIRCLE('',#25003,2.75);
#9244=CIRCLE('',#25005,2.74999999999999);
#9245=CIRCLE('',#25006,2.75);
#9246=CIRCLE('',#25008,2.74999999999999);
#9247=CIRCLE('',#25009,2.75);
#9248=CIRCLE('',#25011,14.);
#9249=CIRCLE('',#25012,14.);
#9250=CIRCLE('',#25014,11.);
#9251=CIRCLE('',#25015,11.);
#9252=CIRCLE('',#25017,10.75);
#9253=CIRCLE('',#25018,10.75);
#9254=CIRCLE('',#25020,7.5);
#9255=CIRCLE('',#25021,7.5);
#9256=CIRCLE('',#25023,10.75);
#9257=CIRCLE('',#25024,10.75);
#9258=CIRCLE('',#25026,11.);
#9259=CIRCLE('',#25027,11.);
#9260=CIRCLE('',#25029,13.5);
#9261=CIRCLE('',#25030,0.5);
#9262=CIRCLE('',#25032,23.);
#9263=CIRCLE('',#25033,23.);
#9264=CIRCLE('',#25035,24.);
#9265=CIRCLE('',#25037,24.);
#9266=CIRCLE('',#25039,24.);
#9267=CIRCLE('',#25041,24.);
#9268=CIRCLE('',#25043,23.);
#9269=CIRCLE('',#25045,23.);
#9270=CIRCLE('',#25059,4.5);
#9271=CIRCLE('',#25060,4.49999999999999);
#9272=CIRCLE('',#25062,4.5);
#9273=CIRCLE('',#25063,4.49999999999999);
#9274=CIRCLE('',#25065,12.);
#9275=CIRCLE('',#25066,12.);
#9276=CIRCLE('',#25068,7.75);
#9277=CIRCLE('',#25069,7.74999999999999);
#9278=CIRCLE('',#25071,6.00000000000001);
#9279=CIRCLE('',#25072,6.00000000000001);
#9280=CIRCLE('',#25074,7.74999999999999);
#9281=CIRCLE('',#25075,7.74999999999999);
#9282=CIRCLE('',#25077,12.);
#9283=CIRCLE('',#25078,12.);
#9284=CIRCLE('',#25080,1.5);
#9285=CIRCLE('',#25081,1.5);
#9286=CIRCLE('',#25082,1.5);
#9287=CIRCLE('',#25083,1.5);
#9288=CIRCLE('',#25084,1.5);
#9289=CIRCLE('',#25085,1.5);
#9290=CIRCLE('',#25087,1.5);
#9291=CIRCLE('',#25088,1.5);
#9292=CIRCLE('',#25089,1.5);
#9293=CIRCLE('',#25090,1.5);
#9294=CIRCLE('',#25091,1.5);
#9295=CIRCLE('',#25092,1.5);
#9296=CIRCLE('',#25094,1.5);
#9297=CIRCLE('',#25095,1.5);
#9298=CIRCLE('',#25096,1.5);
#9299=CIRCLE('',#25097,1.5);
#9300=CIRCLE('',#25098,1.5);
#9301=CIRCLE('',#25099,1.5);
#9302=CIRCLE('',#25101,1.5);
#9303=CIRCLE('',#25102,1.5);
#9304=CIRCLE('',#25103,1.5);
#9305=CIRCLE('',#25104,1.5);
#9306=CIRCLE('',#25105,1.5);
#9307=CIRCLE('',#25106,1.5);
#9308=CIRCLE('',#25108,3.1);
#9309=CIRCLE('',#25109,3.1);
#9310=CIRCLE('',#25111,3.1);
#9311=CIRCLE('',#25112,3.1);
#9312=CIRCLE('',#25114,3.1);
#9313=CIRCLE('',#25115,3.1);
#9314=CIRCLE('',#25117,3.1);
#9315=CIRCLE('',#25118,3.1);
#9316=CIRCLE('',#25120,3.5);
#9317=CIRCLE('',#25121,3.5);
#9318=CIRCLE('',#25123,3.5);
#9319=CIRCLE('',#25124,3.5);
#9320=CIRCLE('',#25126,3.50000000000001);
#9321=CIRCLE('',#25127,3.50000000000001);
#9322=CIRCLE('',#25129,3.50000000000001);
#9323=CIRCLE('',#25130,3.50000000000001);
#9324=CIRCLE('',#25217,5.4585);
#9325=CIRCLE('',#25218,6.);
#9326=CIRCLE('',#25219,5.4585);
#9327=CIRCLE('',#25221,5.4585);
#9328=CIRCLE('',#25222,6.);
#9329=CIRCLE('',#25225,11.);
#9330=CIRCLE('',#25226,11.);
#9331=CIRCLE('',#25228,8.5);
#9332=CIRCLE('',#25229,8.5);
#9333=CIRCLE('',#25231,11.);
#9334=CIRCLE('',#25232,11.);
#9335=CIRCLE('',#25234,11.);
#9336=CIRCLE('',#25235,11.);
#9337=CIRCLE('',#25237,11.);
#9338=CIRCLE('',#25238,11.);
#9339=CIRCLE('',#25247,2.);
#9340=CIRCLE('',#25248,1.8);
#9341=CIRCLE('',#25250,2.);
#9342=CIRCLE('',#25251,1.25);
#9343=CIRCLE('',#25252,2.);
#9344=CIRCLE('',#25265,7.75);
#9345=CIRCLE('',#25266,7.75);
#9346=CIRCLE('',#25268,6.);
#9347=CIRCLE('',#25269,6.);
#9348=CIRCLE('',#25279,4.5);
#9349=CIRCLE('',#25280,4.49999999999999);
#9350=CIRCLE('',#25282,4.5);
#9351=CIRCLE('',#25283,4.49999999999999);
#9352=CIRCLE('',#25285,13.);
#9353=CIRCLE('',#25286,13.);
#9354=CIRCLE('',#25302,5.3);
#9355=CIRCLE('',#25303,0.300000000000002);
#9356=CIRCLE('',#25304,4.99999999999999);
#9357=CIRCLE('',#25306,5.);
#9358=CIRCLE('',#25308,0.300000000000002);
#9359=CIRCLE('',#25309,5.3);
#9360=CIRCLE('',#25311,6.7);
#9361=CIRCLE('',#25312,6.7);
#9362=CIRCLE('',#25314,9.8);
#9363=CIRCLE('',#25315,9.8);
#9364=CIRCLE('',#25317,12.7);
#9365=CIRCLE('',#25318,0.300000000000001);
#9366=CIRCLE('',#25319,13.);
#9367=CIRCLE('',#25321,13.);
#9368=CIRCLE('',#25323,0.300000000000002);
#9369=CIRCLE('',#25324,12.7);
#9370=CIRCLE('',#25326,9.8);
#9371=CIRCLE('',#25327,9.8);
#9372=CIRCLE('',#25329,6.69999999999999);
#9373=CIRCLE('',#25330,6.69999999999999);
#9374=CIRCLE('',#25339,0.6);
#9375=CIRCLE('',#25340,0.6);
#9376=CIRCLE('',#25342,0.6);
#9377=CIRCLE('',#25343,0.6);
#9378=CIRCLE('',#25345,4.8);
#9379=CIRCLE('',#25346,4.8);
#9380=CIRCLE('',#25348,6.15);
#9381=CIRCLE('',#25349,6.15);
#9382=CIRCLE('',#25351,1.6);
#9383=CIRCLE('',#25352,1.6);
#9384=CIRCLE('',#25353,1.6);
#9385=CIRCLE('',#25354,1.6);
#9386=CIRCLE('',#25356,1.6);
#9387=CIRCLE('',#25357,1.6);
#9388=CIRCLE('',#25358,1.6);
#9389=CIRCLE('',#25359,1.6);
#9390=CIRCLE('',#25374,3.);
#9391=CIRCLE('',#25375,3.);
#9392=CIRCLE('',#25377,3.);
#9393=CIRCLE('',#25378,3.);
#9394=CIRCLE('',#25380,4.25000000000001);
#9395=CIRCLE('',#25381,4.25000000000001);
#9396=CIRCLE('',#25383,4.25000000000001);
#9397=CIRCLE('',#25384,4.25000000000001);
#9398=CIRCLE('',#25399,3.);
#9399=CIRCLE('',#25400,3.);
#9400=CIRCLE('',#25402,3.);
#9401=CIRCLE('',#25403,3.);
#9402=CIRCLE('',#25405,4.25000000000001);
#9403=CIRCLE('',#25406,4.25000000000001);
#9404=CIRCLE('',#25408,4.25000000000001);
#9405=CIRCLE('',#25409,4.25000000000001);
#9406=CIRCLE('',#25424,1.65);
#9407=CIRCLE('',#25425,1.65);
#9408=CIRCLE('',#25427,1.65);
#9409=CIRCLE('',#25428,1.65);
#9410=CIRCLE('',#25430,1.65);
#9411=CIRCLE('',#25431,1.65);
#9412=CIRCLE('',#25433,1.65);
#9413=CIRCLE('',#25434,1.65);
#9414=CIRCLE('',#25436,3.);
#9415=CIRCLE('',#25437,3.);
#9416=CIRCLE('',#25439,3.);
#9417=CIRCLE('',#25440,3.);
#9418=CIRCLE('',#25442,5.5);
#9419=CIRCLE('',#25443,5.5);
#9420=CIRCLE('',#25445,3.3);
#9421=CIRCLE('',#25446,3.3);
#9422=CIRCLE('',#25448,5.5);
#9423=CIRCLE('',#25449,5.5);
#9424=CIRCLE('',#25451,3.3);
#9425=CIRCLE('',#25452,3.3);
#9426=CIRCLE('',#25454,10.);
#9427=CIRCLE('',#25455,10.);
#9428=CIRCLE('',#25457,25.);
#9429=CIRCLE('',#25458,25.);
#9430=CIRCLE('',#25472,1.5);
#9431=CIRCLE('',#25474,1.5);
#9432=CIRCLE('',#25476,9.);
#9433=CIRCLE('',#25477,9.);
#9434=CIRCLE('',#25479,1.5);
#9435=CIRCLE('',#25481,1.5);
#9436=CIRCLE('',#25483,0.400000000003301);
#9437=CIRCLE('',#25484,0.400018246612719);
#9438=CIRCLE('',#25485,0.4000000000033);
#9439=CIRCLE('',#25486,0.499983844668534);
#9440=CIRCLE('',#25487,0.499989222937552);
#9441=CIRCLE('',#25488,0.4);
#9442=CIRCLE('',#25489,0.4000000000004);
#9443=CIRCLE('',#25491,0.399999999999999);
#9444=CIRCLE('',#25493,0.399999999950399);
#9445=CIRCLE('',#25494,0.400000000003299);
#9446=CIRCLE('',#25495,0.50000942462105);
#9447=CIRCLE('',#25496,0.400018241496959);
#9448=CIRCLE('',#25498,0.4000000000033);
#9449=CIRCLE('',#25499,0.499988527203264);
#9450=CIRCLE('',#25500,0.400018246602581);
#9451=CIRCLE('',#25502,0.4000000000033);
#9452=CIRCLE('',#25503,0.4000000000033);
#9453=CIRCLE('',#25505,0.4000000000004);
#9454=CIRCLE('',#25507,0.40002572214466);
#9455=CIRCLE('',#25508,0.500009686373483);
#9456=CIRCLE('',#25509,0.49998900112587);
#9457=CIRCLE('',#25510,0.4);
#9458=CIRCLE('',#25511,0.4000000000004);
#9459=CIRCLE('',#25513,0.4);
#9460=CIRCLE('',#25515,0.3999999999504);
#9461=CIRCLE('',#25516,0.4000000000033);
#9462=CIRCLE('',#25517,0.500010213165878);
#9463=CIRCLE('',#25518,0.400018241494099);
#9464=CIRCLE('',#25520,0.4000000000033);
#9465=CIRCLE('',#25521,0.499988839014698);
#9466=CIRCLE('',#25522,0.400018246604447);
#9467=CIRCLE('',#25524,0.400000000003301);
#9468=CIRCLE('',#25525,0.400000000003301);
#9469=CIRCLE('',#25527,0.400000000000399);
#9470=CIRCLE('',#25529,0.400025722143921);
#9471=CIRCLE('',#25530,0.500008606842085);
#9472=CIRCLE('',#25531,0.499984919866047);
#9473=CIRCLE('',#25532,0.4);
#9474=CIRCLE('',#25533,0.4000000000004);
#9475=CIRCLE('',#25535,0.4);
#9476=CIRCLE('',#25537,0.3999999999504);
#9477=CIRCLE('',#25538,0.400000000003302);
#9478=CIRCLE('',#25539,0.500022426641145);
#9479=CIRCLE('',#25540,0.400018241484847);
#9480=CIRCLE('',#25542,0.4000000000033);
#9481=CIRCLE('',#25543,0.499988763335309);
#9482=CIRCLE('',#25544,0.400018246619586);
#9483=CIRCLE('',#25546,0.400000000003301);
#9484=CIRCLE('',#25547,0.4000000000033);
#9485=CIRCLE('',#25549,0.400000000000401);
#9486=CIRCLE('',#25551,0.400025722154133);
#9487=CIRCLE('',#25552,0.500008887107232);
#9488=CIRCLE('',#25553,0.499989277844728);
#9489=CIRCLE('',#25554,0.4);
#9490=CIRCLE('',#25555,0.4000000000004);
#9491=CIRCLE('',#25557,0.399999999999999);
#9492=CIRCLE('',#25559,0.3999999999504);
#9493=CIRCLE('',#25560,0.400000000003299);
#9494=CIRCLE('',#25561,0.500008216044762);
#9495=CIRCLE('',#25562,0.400018241439198);
#9496=CIRCLE('',#25564,0.4000000000033);
#9497=CIRCLE('',#25565,0.499982708615474);
#9498=CIRCLE('',#25566,0.400018246543346);
#9499=CIRCLE('',#25568,0.4000000000033);
#9500=CIRCLE('',#25569,0.4000000000033);
#9501=CIRCLE('',#25571,0.400000000000399);
#9502=CIRCLE('',#25573,0.400025722215534);
#9503=CIRCLE('',#25574,0.500011264103594);
#9504=CIRCLE('',#25576,0.4000000000003);
#9505=CIRCLE('',#25577,0.400025722150869);
#9506=CIRCLE('',#25578,0.4000000000003);
#9507=CIRCLE('',#25580,0.4);
#9508=CIRCLE('',#25582,0.4);
#9509=CIRCLE('',#25583,0.399999999950402);
#9510=CIRCLE('',#25584,0.499989175301816);
#9511=CIRCLE('',#25585,0.500009622535219);
#9512=CIRCLE('',#25586,0.400000000003302);
#9513=CIRCLE('',#25588,0.4000000000033);
#9514=CIRCLE('',#25589,0.400018241481554);
#9515=CIRCLE('',#25590,0.499988814391298);
#9516=CIRCLE('',#25591,0.4);
#9517=CIRCLE('',#25592,0.4000000000004);
#9518=CIRCLE('',#25594,0.4);
#9519=CIRCLE('',#25596,0.3999999999504);
#9520=CIRCLE('',#25597,0.400000000003299);
#9521=CIRCLE('',#25598,0.500009986819179);
#9522=CIRCLE('',#25599,0.400018241441403);
#9523=CIRCLE('',#25601,0.4000000000033);
#9524=CIRCLE('',#25602,0.499988313792213);
#9525=CIRCLE('',#25603,0.400018246554086);
#9526=CIRCLE('',#25605,0.400000000003301);
#9527=CIRCLE('',#25606,0.400000000003301);
#9528=CIRCLE('',#25608,0.400000000000401);
#9529=CIRCLE('',#25610,0.400025722217637);
#9530=CIRCLE('',#25611,0.500009101578587);
#9531=CIRCLE('',#25612,9.832396974191);
#9532=CIRCLE('',#25613,9.832396974191);
#9533=CIRCLE('',#25614,9.83239697419101);
#9534=CIRCLE('',#25615,9.832396974191);
#9535=CIRCLE('',#25616,9.832396974191);
#9536=CIRCLE('',#25617,9.832396974191);
#9537=CIRCLE('',#25618,9.832396974191);
#9538=CIRCLE('',#25619,9.832396974191);
#9539=CIRCLE('',#25620,9.832396974191);
#9540=CIRCLE('',#25621,9.832396974191);
#9541=CIRCLE('',#25622,9.832396974191);
#9542=CIRCLE('',#25623,9.832396974191);
#9543=CIRCLE('',#25625,1.5);
#9544=CIRCLE('',#25627,1.5);
#9545=CIRCLE('',#25629,1.5);
#9546=CIRCLE('',#25631,1.5);
#9547=CIRCLE('',#25634,0.500022231909381);
#9548=CIRCLE('',#25636,1.5);
#9549=CIRCLE('',#25638,1.5);
#9550=CIRCLE('',#25640,1.5);
#9551=CIRCLE('',#25642,1.5);
#9552=CIRCLE('',#25646,2.5);
#9553=CIRCLE('',#25648,2.5);
#9554=CIRCLE('',#25659,11.5);
#9555=CIRCLE('',#25660,20.);
#9556=CIRCLE('',#25661,11.5);
#9557=CIRCLE('',#25662,12.);
#9558=CIRCLE('',#25664,19.);
#9559=CIRCLE('',#25665,7.);
#9560=CIRCLE('',#25667,20.);
#9561=CIRCLE('',#25669,20.);
#9562=CIRCLE('',#25671,11.5);
#9563=CIRCLE('',#25672,20.);
#9564=CIRCLE('',#25673,11.5);
#9565=CIRCLE('',#25674,12.);
#9566=CIRCLE('',#25676,11.5);
#9567=CIRCLE('',#25677,12.);
#9568=CIRCLE('',#25678,11.5);
#9569=CIRCLE('',#25679,20.);
#9570=CIRCLE('',#25681,11.5);
#9571=CIRCLE('',#25683,12.);
#9572=CIRCLE('',#25685,12.);
#9573=CIRCLE('',#25687,12.);
#9574=CIRCLE('',#25689,11.5);
#9575=CIRCLE('',#25691,11.5);
#9576=CIRCLE('',#25693,20.);
#9577=CIRCLE('',#25694,11.5);
#9578=CIRCLE('',#25695,20.);
#9579=CIRCLE('',#25696,20.);
#9580=CIRCLE('',#25697,11.5);
#9581=CIRCLE('',#25698,20.);
#9582=CIRCLE('',#25699,11.5);
#9583=CIRCLE('',#25700,7.);
#9584=CIRCLE('',#25706,2.1);
#9585=CIRCLE('',#25711,22.3311974134124);
#9586=CIRCLE('',#25712,22.32884051476);
#9587=CIRCLE('',#25713,20.);
#9588=CIRCLE('',#25714,20.);
#9589=CIRCLE('',#25715,20.);
#9590=CIRCLE('',#25716,20.);
#9591=CIRCLE('',#25717,20.);
#9592=CIRCLE('',#25718,20.);
#9593=CIRCLE('',#25725,20.);
#9594=CIRCLE('',#25726,20.);
#9595=CIRCLE('',#25727,20.);
#9596=CIRCLE('',#25735,19.5);
#9597=CIRCLE('',#25736,19.5);
#9598=CIRCLE('',#25737,19.5);
#9599=CIRCLE('',#25738,19.5);
#9600=CIRCLE('',#25756,19.5);
#9601=CIRCLE('',#25759,19.5);
#9602=CIRCLE('',#25762,19.5);
#9603=CIRCLE('',#25789,21.7696935948967);
#9604=CIRCLE('',#25792,21.7721107487055);
#9605=CIRCLE('',#25796,19.5);
#9606=CIRCLE('',#25799,19.5);
#9607=CIRCLE('',#25802,19.5);
#9608=CIRCLE('',#25809,2.5);
#9609=CIRCLE('',#25811,2.5);
#9610=CIRCLE('',#25822,11.5);
#9611=CIRCLE('',#25823,20.);
#9612=CIRCLE('',#25824,11.5);
#9613=CIRCLE('',#25825,12.);
#9614=CIRCLE('',#25827,19.);
#9615=CIRCLE('',#25828,5.);
#9616=CIRCLE('',#25830,20.);
#9617=CIRCLE('',#25832,20.);
#9618=CIRCLE('',#25834,11.5);
#9619=CIRCLE('',#25835,20.);
#9620=CIRCLE('',#25836,11.5);
#9621=CIRCLE('',#25837,12.);
#9622=CIRCLE('',#25839,11.5);
#9623=CIRCLE('',#25840,12.);
#9624=CIRCLE('',#25841,11.5);
#9625=CIRCLE('',#25842,20.);
#9626=CIRCLE('',#25844,11.5);
#9627=CIRCLE('',#25846,12.);
#9628=CIRCLE('',#25848,12.);
#9629=CIRCLE('',#25850,12.);
#9630=CIRCLE('',#25852,11.5);
#9631=CIRCLE('',#25854,11.5);
#9632=CIRCLE('',#25856,20.);
#9633=CIRCLE('',#25857,11.5);
#9634=CIRCLE('',#25858,20.);
#9635=CIRCLE('',#25859,20.);
#9636=CIRCLE('',#25860,11.5);
#9637=CIRCLE('',#25861,20.);
#9638=CIRCLE('',#25862,11.5);
#9639=CIRCLE('',#25863,5.);
#9640=CIRCLE('',#25871,2.1);
#9641=CIRCLE('',#25873,2.1);
#9642=CIRCLE('',#25874,2.1);
#9643=CIRCLE('',#25879,22.3311974134124);
#9644=CIRCLE('',#25880,22.32884051476);
#9645=CIRCLE('',#25881,20.);
#9646=CIRCLE('',#25882,20.);
#9647=CIRCLE('',#25883,20.);
#9648=CIRCLE('',#25884,20.);
#9649=CIRCLE('',#25885,20.);
#9650=CIRCLE('',#25886,20.);
#9651=CIRCLE('',#25893,20.);
#9652=CIRCLE('',#25894,20.);
#9653=CIRCLE('',#25895,20.);
#9654=CIRCLE('',#25903,19.5);
#9655=CIRCLE('',#25904,19.5);
#9656=CIRCLE('',#25905,19.5);
#9657=CIRCLE('',#25906,19.5);
#9658=CIRCLE('',#25924,19.5);
#9659=CIRCLE('',#25927,19.5);
#9660=CIRCLE('',#25930,19.5);
#9661=CIRCLE('',#25957,21.7696935948967);
#9662=CIRCLE('',#25960,21.7721107487055);
#9663=CIRCLE('',#25964,19.5);
#9664=CIRCLE('',#25967,19.5);
#9665=CIRCLE('',#25970,19.5);
#9666=CIRCLE('',#25984,2.1);
#9667=CIRCLE('',#25985,2.1);
#9668=CIRCLE('',#25987,2.1);
#9669=CIRCLE('',#25988,2.1);
#9670=CIRCLE('',#25990,2.1);
#9671=CIRCLE('',#25991,2.1);
#9672=CIRCLE('',#25993,2.1);
#9673=CIRCLE('',#25994,2.1);
#9674=CIRCLE('',#25996,2.1);
#9675=CIRCLE('',#25997,2.1);
#9676=CIRCLE('',#25999,2.1);
#9677=CIRCLE('',#26000,2.1);
#9678=CIRCLE('',#26002,14.);
#9679=CIRCLE('',#26003,14.);
#9680=CIRCLE('',#26005,10.);
#9681=CIRCLE('',#26006,10.);
#9682=CIRCLE('',#26009,10.);
#9683=CIRCLE('',#26010,10.);
#9684=CIRCLE('',#26018,2.99999999999999);
#9685=CIRCLE('',#26019,2.99999999999999);
#9686=CIRCLE('',#26021,2.99999999999999);
#9687=CIRCLE('',#26022,2.99999999999999);
#9688=CIRCLE('',#26024,3.3);
#9689=CIRCLE('',#26025,3.3);
#9690=CIRCLE('',#26027,3.3);
#9691=CIRCLE('',#26028,3.3);
#9692=CIRCLE('',#26030,3.3);
#9693=CIRCLE('',#26031,3.3);
#9694=CIRCLE('',#26033,3.3);
#9695=CIRCLE('',#26034,3.3);
#9696=CIRCLE('',#26045,3.3);
#9697=CIRCLE('',#26046,3.3);
#9698=CIRCLE('',#26048,3.3);
#9699=CIRCLE('',#26049,3.3);
#9700=CIRCLE('',#26051,3.3);
#9701=CIRCLE('',#26052,3.3);
#9702=CIRCLE('',#26054,3.3);
#9703=CIRCLE('',#26055,3.3);
#9704=CIRCLE('',#26057,3.3);
#9705=CIRCLE('',#26058,3.3);
#9706=CIRCLE('',#26060,3.3);
#9707=CIRCLE('',#26061,3.3);
#9708=CIRCLE('',#26084,55.);
#9709=CIRCLE('',#26085,55.);
#9710=CIRCLE('',#26087,3.39999999999999);
#9711=CIRCLE('',#26088,3.4);
#9712=CIRCLE('',#26090,3.4);
#9713=CIRCLE('',#26091,3.4);
#9714=CIRCLE('',#26093,3.4);
#9715=CIRCLE('',#26094,3.4);
#9716=CIRCLE('',#26096,3.39999999999999);
#9717=CIRCLE('',#26097,3.4);
#9718=CIRCLE('',#26099,4.24999999999998);
#9719=CIRCLE('',#26100,4.24999999999998);
#9720=CIRCLE('',#26102,4.24999999999998);
#9721=CIRCLE('',#26103,4.24999999999998);
#9722=CIRCLE('',#26105,4.24999999999998);
#9723=CIRCLE('',#26106,4.24999999999998);
#9724=CIRCLE('',#26108,4.24999999999998);
#9725=CIRCLE('',#26109,4.24999999999998);
#9726=CIRCLE('',#26111,45.);
#9727=CIRCLE('',#26112,45.);
#9728=CIRCLE('',#26114,65.);
#9729=CIRCLE('',#26115,65.);
#9730=CIRCLE('',#26117,2.99999999999999);
#9731=CIRCLE('',#26118,2.99999999999999);
#9732=CIRCLE('',#26120,2.99999999999999);
#9733=CIRCLE('',#26121,2.99999999999999);
#9734=CIRCLE('',#26123,2.5);
#9735=CIRCLE('',#26124,2.5);
#9736=CIRCLE('',#26126,2.5);
#9737=CIRCLE('',#26127,2.5);
#9738=CIRCLE('',#26129,2.5);
#9739=CIRCLE('',#26130,2.5);
#9740=CIRCLE('',#26132,2.5);
#9741=CIRCLE('',#26133,2.5);
#9742=CIRCLE('',#26135,5.50000000000001);
#9743=CIRCLE('',#26136,5.50000000000001);
#9744=CIRCLE('',#26138,3.30000000000008);
#9745=CIRCLE('',#26139,3.3);
#9746=CIRCLE('',#26141,5.50000000000001);
#9747=CIRCLE('',#26142,5.50000000000001);
#9748=CIRCLE('',#26144,3.30000000000008);
#9749=CIRCLE('',#26145,3.3);
#9750=CIRCLE('',#26147,5.50000000000001);
#9751=CIRCLE('',#26148,5.50000000000001);
#9752=CIRCLE('',#26150,3.30000000000008);
#9753=CIRCLE('',#26151,3.3);
#9754=CIRCLE('',#26153,5.50000000000001);
#9755=CIRCLE('',#26154,5.50000000000001);
#9756=CIRCLE('',#26156,3.30000000000008);
#9757=CIRCLE('',#26157,3.3);
#9758=CIRCLE('',#26159,5.50000000000001);
#9759=CIRCLE('',#26160,5.50000000000001);
#9760=CIRCLE('',#26162,3.30000000000008);
#9761=CIRCLE('',#26163,3.3);
#9762=CIRCLE('',#26165,5.50000000000001);
#9763=CIRCLE('',#26166,5.50000000000001);
#9764=CIRCLE('',#26168,3.30000000000008);
#9765=CIRCLE('',#26169,3.3);
#9766=CIRCLE('',#26171,5.49999999999999);
#9767=CIRCLE('',#26172,5.49999999999999);
#9768=CIRCLE('',#26174,3.30000000000008);
#9769=CIRCLE('',#26175,3.3);
#9770=CIRCLE('',#26177,5.50000000000001);
#9771=CIRCLE('',#26178,5.50000000000001);
#9772=CIRCLE('',#26180,3.30000000000008);
#9773=CIRCLE('',#26181,3.3);
#9774=CIRCLE('',#26183,5.50000000000001);
#9775=CIRCLE('',#26184,5.50000000000001);
#9776=CIRCLE('',#26186,3.30000000000008);
#9777=CIRCLE('',#26187,3.3);
#9778=CIRCLE('',#26189,5.50000000000001);
#9779=CIRCLE('',#26190,5.50000000000001);
#9780=CIRCLE('',#26192,3.30000000000008);
#9781=CIRCLE('',#26193,3.3);
#9782=CIRCLE('',#26195,5.50000000000001);
#9783=CIRCLE('',#26196,5.50000000000001);
#9784=CIRCLE('',#26198,3.30000000000008);
#9785=CIRCLE('',#26199,3.3);
#9786=CIRCLE('',#26201,5.50000000000001);
#9787=CIRCLE('',#26202,5.50000000000001);
#9788=CIRCLE('',#26204,3.30000000000008);
#9789=CIRCLE('',#26205,3.3);
#9790=CIRCLE('',#26207,5.50000000000001);
#9791=CIRCLE('',#26208,5.50000000000001);
#9792=CIRCLE('',#26210,3.30000000000008);
#9793=CIRCLE('',#26211,3.3);
#9794=CIRCLE('',#26213,5.50000000000001);
#9795=CIRCLE('',#26214,5.50000000000001);
#9796=CIRCLE('',#26216,3.30000000000008);
#9797=CIRCLE('',#26217,3.3);
#9798=CIRCLE('',#26219,5.49999999999999);
#9799=CIRCLE('',#26220,5.49999999999999);
#9800=CIRCLE('',#26222,3.30000000000008);
#9801=CIRCLE('',#26223,3.3);
#9802=CIRCLE('',#26225,5.50000000000001);
#9803=CIRCLE('',#26226,5.50000000000001);
#9804=CIRCLE('',#26228,3.30000000000008);
#9805=CIRCLE('',#26229,3.3);
#9806=CIRCLE('',#26235,55.);
#9807=CIRCLE('',#26237,55.);
#9808=CIRCLE('',#26272,5.50000000000001);
#9809=CIRCLE('',#26273,5.50000000000001);
#9810=CIRCLE('',#26275,3.5);
#9811=CIRCLE('',#26277,3.5);
#9812=CIRCLE('',#26279,3.5);
#9813=CIRCLE('',#26280,3.5);
#9814=CIRCLE('',#26281,3.5);
#9815=CIRCLE('',#26283,3.5);
#9816=CIRCLE('',#26286,5.50000000000001);
#9817=CIRCLE('',#26287,5.50000000000001);
#9818=CIRCLE('',#26289,3.5);
#9819=CIRCLE('',#26291,3.5);
#9820=CIRCLE('',#26293,3.5);
#9821=CIRCLE('',#26294,3.5);
#9822=CIRCLE('',#26295,3.5);
#9823=CIRCLE('',#26297,3.5);
#9824=CIRCLE('',#26300,5.50000000000001);
#9825=CIRCLE('',#26301,5.50000000000001);
#9826=CIRCLE('',#26303,3.5);
#9827=CIRCLE('',#26305,3.5);
#9828=CIRCLE('',#26307,3.5);
#9829=CIRCLE('',#26308,3.5);
#9830=CIRCLE('',#26309,3.5);
#9831=CIRCLE('',#26311,3.5);
#9832=CIRCLE('',#26314,5.50000000000001);
#9833=CIRCLE('',#26315,5.50000000000001);
#9834=CIRCLE('',#26317,3.5);
#9835=CIRCLE('',#26319,3.5);
#9836=CIRCLE('',#26321,3.5);
#9837=CIRCLE('',#26322,3.5);
#9838=CIRCLE('',#26323,3.5);
#9839=CIRCLE('',#26325,3.5);
#9840=CIRCLE('',#26328,5.50000000000001);
#9841=CIRCLE('',#26329,5.50000000000001);
#9842=CIRCLE('',#26331,3.5);
#9843=CIRCLE('',#26333,3.5);
#9844=CIRCLE('',#26335,3.5);
#9845=CIRCLE('',#26336,3.5);
#9846=CIRCLE('',#26337,3.5);
#9847=CIRCLE('',#26339,3.5);
#9848=CIRCLE('',#26342,5.50000000000001);
#9849=CIRCLE('',#26343,5.50000000000001);
#9850=CIRCLE('',#26345,3.5);
#9851=CIRCLE('',#26347,3.49999999999999);
#9852=CIRCLE('',#26349,3.5);
#9853=CIRCLE('',#26350,3.5);
#9854=CIRCLE('',#26351,3.5);
#9855=CIRCLE('',#26353,3.49999999999999);
#9856=CIRCLE('',#26356,5.5);
#9857=CIRCLE('',#26357,5.5);
#9858=CIRCLE('',#26359,3.5);
#9859=CIRCLE('',#26361,3.5);
#9860=CIRCLE('',#26363,3.5);
#9861=CIRCLE('',#26364,3.5);
#9862=CIRCLE('',#26365,3.5);
#9863=CIRCLE('',#26367,3.5);
#9864=CIRCLE('',#26370,5.5);
#9865=CIRCLE('',#26371,5.5);
#9866=CIRCLE('',#26373,3.5);
#9867=CIRCLE('',#26375,3.49999999999999);
#9868=CIRCLE('',#26377,3.5);
#9869=CIRCLE('',#26378,3.5);
#9870=CIRCLE('',#26379,3.5);
#9871=CIRCLE('',#26381,3.49999999999999);
#9872=CIRCLE('',#26410,0.999999999999999);
#9873=CIRCLE('',#26411,0.5);
#9874=CIRCLE('',#26412,0.5);
#9875=CIRCLE('',#26413,0.5);
#9876=CIRCLE('',#26414,2.3);
#9877=CIRCLE('',#26415,0.5);
#9878=CIRCLE('',#26416,0.5);
#9879=CIRCLE('',#26417,0.5);
#9880=CIRCLE('',#26418,0.5);
#9881=CIRCLE('',#26419,2.3);
#9882=CIRCLE('',#26420,0.5);
#9883=CIRCLE('',#26421,0.5);
#9884=CIRCLE('',#26422,2.3);
#9885=CIRCLE('',#26423,0.5);
#9886=CIRCLE('',#26424,0.5);
#9887=CIRCLE('',#26425,0.5);
#9888=CIRCLE('',#26426,0.5);
#9889=CIRCLE('',#26427,2.3);
#9890=CIRCLE('',#26428,0.5);
#9891=CIRCLE('',#26429,0.5);
#9892=CIRCLE('',#26430,0.5);
#9893=CIRCLE('',#26431,0.999999999999999);
#9894=CIRCLE('',#26433,0.999999999999999);
#9895=CIRCLE('',#26434,0.5);
#9896=CIRCLE('',#26435,0.5);
#9897=CIRCLE('',#26436,0.5);
#9898=CIRCLE('',#26437,2.3);
#9899=CIRCLE('',#26438,0.5);
#9900=CIRCLE('',#26439,0.5);
#9901=CIRCLE('',#26440,0.5);
#9902=CIRCLE('',#26441,0.5);
#9903=CIRCLE('',#26442,2.3);
#9904=CIRCLE('',#26443,0.5);
#9905=CIRCLE('',#26444,0.5);
#9906=CIRCLE('',#26445,2.3);
#9907=CIRCLE('',#26446,0.5);
#9908=CIRCLE('',#26447,0.5);
#9909=CIRCLE('',#26448,0.5);
#9910=CIRCLE('',#26449,0.5);
#9911=CIRCLE('',#26450,2.3);
#9912=CIRCLE('',#26451,0.5);
#9913=CIRCLE('',#26452,0.5);
#9914=CIRCLE('',#26453,0.5);
#9915=CIRCLE('',#26454,0.999999999999999);
#9916=CIRCLE('',#26509,2.5);
#9917=CIRCLE('',#26510,2.5);
#9918=CIRCLE('',#26512,2.5);
#9919=CIRCLE('',#26513,2.5);
#9920=CIRCLE('',#26515,3.65);
#9921=CIRCLE('',#26516,3.65);
#9922=CIRCLE('',#26520,3.3235);
#9923=CIRCLE('',#26521,3.3235);
#9924=CIRCLE('',#26523,3.3235);
#9925=CIRCLE('',#26524,3.3235);
#9926=CIRCLE('',#26526,3.3235);
#9927=CIRCLE('',#26527,3.32349999999999);
#9928=CIRCLE('',#26529,3.32349999999999);
#9929=CIRCLE('',#26530,3.3235);
#9930=CIRCLE('',#26532,2.5);
#9931=CIRCLE('',#26533,2.5);
#9932=CIRCLE('',#26535,2.5);
#9933=CIRCLE('',#26536,2.5);
#9934=CIRCLE('',#26538,3.65);
#9935=CIRCLE('',#26539,3.65);
#9936=CIRCLE('',#26541,0.500000000000004);
#9937=CIRCLE('',#26542,0.500000000000004);
#9938=CIRCLE('',#26543,0.500000000000006);
#9939=CIRCLE('',#26547,0.5);
#9940=CIRCLE('',#26548,0.5);
#9941=CIRCLE('',#26549,0.5);
#9942=CIRCLE('',#26550,4.);
#9943=CIRCLE('',#26551,4.);
#9944=CIRCLE('',#26553,4.);
#9945=CIRCLE('',#26555,4.99995);
#9946=CIRCLE('',#26556,4.99995);
#9947=CIRCLE('',#26585,2.3);
#9948=CIRCLE('',#26586,2.3);
#9949=CIRCLE('',#26588,2.3);
#9950=CIRCLE('',#26589,2.3);
#9951=CIRCLE('',#26591,2.3);
#9952=CIRCLE('',#26592,2.3);
#9953=CIRCLE('',#26594,2.3);
#9954=CIRCLE('',#26595,2.3);
#9955=CIRCLE('',#26597,0.5);
#9956=CIRCLE('',#26598,0.5);
#9957=CIRCLE('',#26600,0.5);
#9958=CIRCLE('',#26601,0.5);
#9959=CIRCLE('',#26603,0.5);
#9960=CIRCLE('',#26604,0.5);
#9961=CIRCLE('',#26606,0.5);
#9962=CIRCLE('',#26607,0.5);
#9963=CIRCLE('',#26609,0.5);
#9964=CIRCLE('',#26610,0.5);
#9965=CIRCLE('',#26612,0.5);
#9966=CIRCLE('',#26613,0.5);
#9967=CIRCLE('',#26615,0.5);
#9968=CIRCLE('',#26616,0.5);
#9969=CIRCLE('',#26618,0.5);
#9970=CIRCLE('',#26619,0.5);
#9971=CIRCLE('',#26621,0.5);
#9972=CIRCLE('',#26622,0.5);
#9973=CIRCLE('',#26624,0.5);
#9974=CIRCLE('',#26625,0.5);
#9975=CIRCLE('',#26627,0.5);
#9976=CIRCLE('',#26628,0.5);
#9977=CIRCLE('',#26630,0.499999999999999);
#9978=CIRCLE('',#26631,0.5);
#9979=CIRCLE('',#26633,0.5);
#9980=CIRCLE('',#26634,0.5);
#9981=CIRCLE('',#26636,0.5);
#9982=CIRCLE('',#26637,0.5);
#9983=CIRCLE('',#26639,0.5);
#9984=CIRCLE('',#26640,0.5);
#9985=CIRCLE('',#26642,0.500000000000001);
#9986=CIRCLE('',#26643,0.5);
#9987=CIRCLE('',#26661,0.450000000000001);
#9988=CIRCLE('',#26662,0.450000000000001);
#9989=CIRCLE('',#26663,0.55);
#9990=CIRCLE('',#26664,2.25);
#9991=CIRCLE('',#26665,0.549999999999998);
#9992=CIRCLE('',#26666,0.55);
#9993=CIRCLE('',#26667,0.55);
#9994=CIRCLE('',#26668,0.55);
#9995=CIRCLE('',#26669,2.25);
#9996=CIRCLE('',#26670,0.55);
#9997=CIRCLE('',#26671,0.550000000000001);
#9998=CIRCLE('',#26672,2.25);
#9999=CIRCLE('',#26673,0.550000000000002);
#10000=CIRCLE('',#26674,0.55);
#10001=CIRCLE('',#26675,0.55);
#10002=CIRCLE('',#26676,0.55);
#10003=CIRCLE('',#26677,2.25);
#10004=CIRCLE('',#26678,0.55);
#10005=CIRCLE('',#26679,0.450000000000001);
#10006=CIRCLE('',#26680,0.450000000000001);
#10007=CIRCLE('',#26683,0.450000000000001);
#10008=CIRCLE('',#26686,0.450000000000001);
#10009=CIRCLE('',#26689,0.55);
#10010=CIRCLE('',#26691,2.25);
#10011=CIRCLE('',#26693,0.549999999999998);
#10012=CIRCLE('',#26696,0.55);
#10013=CIRCLE('',#26699,0.55);
#10014=CIRCLE('',#26702,0.55);
#10015=CIRCLE('',#26704,2.25);
#10016=CIRCLE('',#26706,0.55);
#10017=CIRCLE('',#26711,0.550000000000001);
#10018=CIRCLE('',#26713,2.25);
#10019=CIRCLE('',#26715,0.550000000000002);
#10020=CIRCLE('',#26718,0.55);
#10021=CIRCLE('',#26721,0.55);
#10022=CIRCLE('',#26724,0.55);
#10023=CIRCLE('',#26726,2.25);
#10024=CIRCLE('',#26728,0.55);
#10025=CIRCLE('',#26731,0.450000000000001);
#10026=CIRCLE('',#26734,0.450000000000001);
#10027=CIRCLE('',#26747,0.5);
#10028=CIRCLE('',#26749,4.99995);
#10029=CIRCLE('',#26750,0.5);
#10030=CIRCLE('',#26751,0.5);
#10031=CIRCLE('',#26752,0.5);
#10032=CIRCLE('',#26753,2.3);
#10033=CIRCLE('',#26754,0.5);
#10034=CIRCLE('',#26755,0.5);
#10035=CIRCLE('',#26756,0.5);
#10036=CIRCLE('',#26757,0.5);
#10037=CIRCLE('',#26758,2.3);
#10038=CIRCLE('',#26759,0.5);
#10039=CIRCLE('',#26760,0.5);
#10040=CIRCLE('',#26761,2.3);
#10041=CIRCLE('',#26762,0.5);
#10042=CIRCLE('',#26763,0.5);
#10043=CIRCLE('',#26764,0.5);
#10044=CIRCLE('',#26765,0.5);
#10045=CIRCLE('',#26766,2.3);
#10046=CIRCLE('',#26767,0.5);
#10047=CIRCLE('',#26768,0.5);
#10048=CIRCLE('',#26769,0.5);
#10049=CIRCLE('',#26773,0.5);
#10050=CIRCLE('',#26776,0.500000000000006);
#10051=CIRCLE('',#26788,0.5);
#10052=CIRCLE('',#26791,0.5);
#10053=CIRCLE('',#26794,0.5);
#10054=CIRCLE('',#26796,2.3);
#10055=CIRCLE('',#26798,0.499999999999999);
#10056=CIRCLE('',#26801,0.5);
#10057=CIRCLE('',#26804,0.5);
#10058=CIRCLE('',#26807,0.5);
#10059=CIRCLE('',#26809,2.3);
#10060=CIRCLE('',#26811,0.500000000000001);
#10061=CIRCLE('',#26816,0.5);
#10062=CIRCLE('',#26818,2.3);
#10063=CIRCLE('',#26820,0.5);
#10064=CIRCLE('',#26823,0.5);
#10065=CIRCLE('',#26826,0.5);
#10066=CIRCLE('',#26829,0.5);
#10067=CIRCLE('',#26831,2.3);
#10068=CIRCLE('',#26833,0.5);
#10069=CIRCLE('',#26836,0.5);
#10070=CIRCLE('',#26839,0.5);
#10071=CIRCLE('',#26847,0.500000000000006);
#10072=CIRCLE('',#26849,2.);
#10073=CIRCLE('',#26850,2.);
#10074=CIRCLE('',#26855,2.);
#10075=CIRCLE('',#26857,2.);
#10076=CIRCLE('',#26859,0.450000000000001);
#10077=CIRCLE('',#26860,0.450000000000001);
#10078=CIRCLE('',#26861,0.55);
#10079=CIRCLE('',#26862,2.25);
#10080=CIRCLE('',#26863,0.55);
#10081=CIRCLE('',#26864,0.55);
#10082=CIRCLE('',#26865,0.55);
#10083=CIRCLE('',#26866,0.550000000000002);
#10084=CIRCLE('',#26867,2.25);
#10085=CIRCLE('',#26868,0.550000000000001);
#10086=CIRCLE('',#26869,0.55);
#10087=CIRCLE('',#26870,2.25);
#10088=CIRCLE('',#26871,0.55);
#10089=CIRCLE('',#26872,0.55);
#10090=CIRCLE('',#26873,0.55);
#10091=CIRCLE('',#26874,0.549999999999998);
#10092=CIRCLE('',#26875,2.25);
#10093=CIRCLE('',#26876,0.55);
#10094=CIRCLE('',#26877,0.450000000000001);
#10095=CIRCLE('',#26878,0.450000000000001);
#10096=CIRCLE('',#26890,5.5);
#10097=CIRCLE('',#26896,5.5);
#10098=CIRCLE('',#26913,0.450000000000001);
#10099=CIRCLE('',#26916,0.450000000000001);
#10100=CIRCLE('',#26919,0.55);
#10101=CIRCLE('',#26921,2.25);
#10102=CIRCLE('',#26923,0.55);
#10103=CIRCLE('',#26926,0.55);
#10104=CIRCLE('',#26929,0.55);
#10105=CIRCLE('',#26932,0.550000000000002);
#10106=CIRCLE('',#26934,2.25);
#10107=CIRCLE('',#26936,0.550000000000001);
#10108=CIRCLE('',#26941,0.55);
#10109=CIRCLE('',#26943,2.25);
#10110=CIRCLE('',#26945,0.55);
#10111=CIRCLE('',#26948,0.55);
#10112=CIRCLE('',#26951,0.55);
#10113=CIRCLE('',#26954,0.549999999999998);
#10114=CIRCLE('',#26956,2.25);
#10115=CIRCLE('',#26958,0.55);
#10116=CIRCLE('',#26961,0.450000000000001);
#10117=CIRCLE('',#26964,0.450000000000001);
#10118=CIRCLE('',#26991,5.50000000000001);
#10119=CIRCLE('',#26999,5.49999999999999);
#10120=CIRCLE('',#27008,0.5);
#10121=CIRCLE('',#27009,0.5);
#10122=CIRCLE('',#27010,0.5);
#10123=CIRCLE('',#27011,2.3);
#10124=CIRCLE('',#27012,0.499999999999999);
#10125=CIRCLE('',#27013,0.5);
#10126=CIRCLE('',#27014,0.5);
#10127=CIRCLE('',#27015,0.5);
#10128=CIRCLE('',#27016,2.3);
#10129=CIRCLE('',#27017,0.500000000000001);
#10130=CIRCLE('',#27018,0.5);
#10131=CIRCLE('',#27019,2.3);
#10132=CIRCLE('',#27020,0.5);
#10133=CIRCLE('',#27021,0.5);
#10134=CIRCLE('',#27022,0.5);
#10135=CIRCLE('',#27023,0.5);
#10136=CIRCLE('',#27024,2.3);
#10137=CIRCLE('',#27025,0.5);
#10138=CIRCLE('',#27026,0.5);
#10139=CIRCLE('',#27027,0.5);
#10140=CIRCLE('',#27035,0.5);
#10141=CIRCLE('',#27037,0.5);
#10142=CIRCLE('',#27042,0.5);
#10143=CIRCLE('',#27044,0.5);
#10144=CIRCLE('',#27046,2.3);
#10145=CIRCLE('',#27048,0.5);
#10146=CIRCLE('',#27050,0.5);
#10147=CIRCLE('',#27054,0.5);
#10148=CIRCLE('',#27056,0.5);
#10149=CIRCLE('',#27058,2.3);
#10150=CIRCLE('',#27062,0.500000000000001);
#10151=CIRCLE('',#27064,0.5);
#10152=CIRCLE('',#27066,2.3);
#10153=CIRCLE('',#27068,0.5);
#10154=CIRCLE('',#27070,0.5);
#10155=CIRCLE('',#27075,0.499999999999999);
#10156=CIRCLE('',#27077,0.5);
#10157=CIRCLE('',#27079,2.3);
#10158=CIRCLE('',#27081,0.5);
#10159=CIRCLE('',#27083,0.5);
#10160=CIRCLE('',#27100,4.99995);
#10161=CIRCLE('',#27109,3.44123551017618);
#10162=CIRCLE('',#27110,1.21);
#10163=CIRCLE('',#27111,3.21339563862929);
#10164=CIRCLE('',#27112,2.);
#10165=CIRCLE('',#27113,3.36374346224613);
#10166=CIRCLE('',#27115,2.5);
#10167=CIRCLE('',#27117,1.09087121146357);
#10168=CIRCLE('',#27119,3.46410161513777);
#10169=CIRCLE('',#27121,3.46410161513775);
#10170=CIRCLE('',#27123,3.);
#10171=CIRCLE('',#27124,3.);
#10172=CIRCLE('',#27126,4.);
#10173=CIRCLE('',#27127,4.);
#10174=CIRCLE('',#27128,4.);
#10175=CIRCLE('',#27129,4.);
#10176=CIRCLE('',#27130,4.);
#10177=CIRCLE('',#27131,4.);
#10178=CIRCLE('',#27132,4.);
#10179=CIRCLE('',#27133,4.);
#10180=CIRCLE('',#27134,4.);
#10181=CIRCLE('',#27136,4.);
#10182=CIRCLE('',#27138,3.46410161513776);
#10183=CIRCLE('',#27139,3.46410161513777);
#10184=CIRCLE('',#27140,3.46410161513777);
#10185=CIRCLE('',#27141,3.46410161513777);
#10186=CIRCLE('',#27142,3.46410161513777);
#10187=CIRCLE('',#27144,3.46410161513775);
#10188=CIRCLE('',#27145,3.46410161513775);
#10189=CIRCLE('',#27146,3.46410161513775);
#10190=CIRCLE('',#27147,3.46410161513775);
#10191=CIRCLE('',#27148,3.46410161513776);
#10192=CIRCLE('',#27191,2.5);
#10193=CIRCLE('',#27192,2.5);
#10194=CIRCLE('',#27195,2.5);
#10195=CIRCLE('',#27196,2.5);
#10196=CIRCLE('',#27199,2.5);
#10197=CIRCLE('',#27200,2.5);
#10198=CIRCLE('',#27203,2.5);
#10199=CIRCLE('',#27204,2.5);
#10200=CIRCLE('',#27207,2.5);
#10201=CIRCLE('',#27208,2.5);
#10202=CIRCLE('',#27211,2.5);
#10203=CIRCLE('',#27212,2.5);
#10204=CIRCLE('',#27215,2.5);
#10205=CIRCLE('',#27216,2.5);
#10206=CIRCLE('',#27219,2.5);
#10207=CIRCLE('',#27220,2.5);
#10208=CIRCLE('',#27224,0.200000000000001);
#10209=CIRCLE('',#27225,0.200000000000001);
#10210=CIRCLE('',#27228,0.200000000000001);
#10211=CIRCLE('',#27229,0.200000000000001);
#10212=CIRCLE('',#27240,4.25);
#10213=CIRCLE('',#27241,4.25);
#10214=CIRCLE('',#27242,3.75);
#10215=CIRCLE('',#27244,2.);
#10216=CIRCLE('',#27245,2.);
#10217=CIRCLE('',#27246,2.);
#10218=CIRCLE('',#27247,2.);
#10219=CIRCLE('',#27248,2.);
#10220=CIRCLE('',#27249,2.);
#10221=CIRCLE('',#27250,2.);
#10222=CIRCLE('',#27252,4.25);
#10223=CIRCLE('',#27254,2.065);
#10224=CIRCLE('',#27255,2.065);
#10225=CIRCLE('',#27257,2.5);
#10226=CIRCLE('',#27258,2.5);
#10227=CIRCLE('',#27276,5.);
#10228=CIRCLE('',#27277,5.);
#10229=CIRCLE('',#27279,2.5);
#10230=CIRCLE('',#27280,2.5);
#10231=CIRCLE('',#27284,4.25);
#10232=CIRCLE('',#27285,4.25);
#10233=CIRCLE('',#27287,2.5);
#10234=CIRCLE('',#27288,2.5);
#10235=CIRCLE('',#27295,5.);
#10236=CIRCLE('',#27296,5.);
#10237=CIRCLE('',#27298,4.4);
#10238=CIRCLE('',#27300,3.);
#10239=CIRCLE('',#27301,2.4585);
#10240=CIRCLE('',#27302,3.);
#10241=CIRCLE('',#27304,3.);
#10242=CIRCLE('',#27317,6.5);
#10243=CIRCLE('',#27318,6.5);
#10244=CIRCLE('',#27319,5.7);
#10245=CIRCLE('',#27321,3.);
#10246=CIRCLE('',#27322,3.);
#10247=CIRCLE('',#27323,3.);
#10248=CIRCLE('',#27324,3.);
#10249=CIRCLE('',#27325,3.);
#10250=CIRCLE('',#27326,3.);
#10251=CIRCLE('',#27327,3.);
#10252=CIRCLE('',#27329,6.5);
#10253=CIRCLE('',#27331,3.3225);
#10254=CIRCLE('',#27332,3.3225);
#10255=CIRCLE('',#27334,4.);
#10256=CIRCLE('',#27335,4.);
#10257=CIRCLE('',#27353,8.);
#10258=CIRCLE('',#27354,8.);
#10259=CIRCLE('',#27356,4.);
#10260=CIRCLE('',#27357,4.);
#10261=CIRCLE('',#27361,7.25);
#10262=CIRCLE('',#27362,7.25);
#10263=CIRCLE('',#27364,4.);
#10264=CIRCLE('',#27365,4.);
#10265=CIRCLE('',#27372,5.);
#10266=CIRCLE('',#27373,5.);
#10267=CIRCLE('',#27375,4.4);
#10268=CIRCLE('',#27377,3.);
#10269=CIRCLE('',#27378,2.4585);
#10270=CIRCLE('',#27379,3.);
#10271=CIRCLE('',#27381,3.);
#10272=CIRCLE('',#27394,3.5);
#10273=CIRCLE('',#27395,3.5);
#10274=CIRCLE('',#27397,3.1);
#10275=CIRCLE('',#27399,2.);
#10276=CIRCLE('',#27400,1.621);
#10277=CIRCLE('',#27401,2.);
#10278=CIRCLE('',#27403,2.);
#10279=VERTEX_POINT('',#34635);
#10280=VERTEX_POINT('',#34637);
#10281=VERTEX_POINT('',#34641);
#10282=VERTEX_POINT('',#34643);
#10283=VERTEX_POINT('',#34647);
#10284=VERTEX_POINT('',#34649);
#10285=VERTEX_POINT('',#34653);
#10286=VERTEX_POINT('',#34655);
#10287=VERTEX_POINT('',#34659);
#10288=VERTEX_POINT('',#34661);
#10289=VERTEX_POINT('',#34665);
#10290=VERTEX_POINT('',#34667);
#10291=VERTEX_POINT('',#34671);
#10292=VERTEX_POINT('',#34673);
#10293=VERTEX_POINT('',#34677);
#10294=VERTEX_POINT('',#34679);
#10295=VERTEX_POINT('',#34683);
#10296=VERTEX_POINT('',#34685);
#10297=VERTEX_POINT('',#34689);
#10298=VERTEX_POINT('',#34692);
#10299=VERTEX_POINT('',#34694);
#10300=VERTEX_POINT('',#34698);
#10301=VERTEX_POINT('',#34701);
#10302=VERTEX_POINT('',#34703);
#10303=VERTEX_POINT('',#34707);
#10304=VERTEX_POINT('',#34710);
#10305=VERTEX_POINT('',#34712);
#10306=VERTEX_POINT('',#34716);
#10307=VERTEX_POINT('',#34719);
#10308=VERTEX_POINT('',#34720);
#10309=VERTEX_POINT('',#34722);
#10310=VERTEX_POINT('',#34724);
#10311=VERTEX_POINT('',#34728);
#10312=VERTEX_POINT('',#34729);
#10313=VERTEX_POINT('',#34731);
#10314=VERTEX_POINT('',#34733);
#10315=VERTEX_POINT('',#34737);
#10316=VERTEX_POINT('',#34739);
#10317=VERTEX_POINT('',#34746);
#10318=VERTEX_POINT('',#34748);
#10319=VERTEX_POINT('',#34752);
#10320=VERTEX_POINT('',#34754);
#10321=VERTEX_POINT('',#34758);
#10322=VERTEX_POINT('',#34760);
#10323=VERTEX_POINT('',#34772);
#10324=VERTEX_POINT('',#34774);
#10325=VERTEX_POINT('',#34776);
#10326=VERTEX_POINT('',#34778);
#10327=VERTEX_POINT('',#34780);
#10328=VERTEX_POINT('',#34799);
#10329=VERTEX_POINT('',#34803);
#10330=VERTEX_POINT('',#34807);
#10331=VERTEX_POINT('',#34809);
#10332=VERTEX_POINT('',#34813);
#10333=VERTEX_POINT('',#34817);
#10334=VERTEX_POINT('',#34821);
#10335=VERTEX_POINT('',#34823);
#10336=VERTEX_POINT('',#34827);
#10337=VERTEX_POINT('',#34828);
#10338=VERTEX_POINT('',#34833);
#10339=VERTEX_POINT('',#34837);
#10340=VERTEX_POINT('',#34839);
#10341=VERTEX_POINT('',#34843);
#10342=VERTEX_POINT('',#34847);
#10343=VERTEX_POINT('',#34849);
#10344=VERTEX_POINT('',#34853);
#10345=VERTEX_POINT('',#34854);
#10346=VERTEX_POINT('',#34857);
#10347=VERTEX_POINT('',#34861);
#10348=VERTEX_POINT('',#34870);
#10349=VERTEX_POINT('',#34875);
#10350=VERTEX_POINT('',#34882);
#10351=VERTEX_POINT('',#34884);
#10352=VERTEX_POINT('',#34889);
#10353=VERTEX_POINT('',#34893);
#10354=VERTEX_POINT('',#34901);
#10355=VERTEX_POINT('',#34936);
#10356=VERTEX_POINT('',#34973);
#10357=VERTEX_POINT('',#34975);
#10358=VERTEX_POINT('',#34979);
#10359=VERTEX_POINT('',#34981);
#10360=VERTEX_POINT('',#34985);
#10361=VERTEX_POINT('',#34987);
#10362=VERTEX_POINT('',#34991);
#10363=VERTEX_POINT('',#34993);
#10364=VERTEX_POINT('',#34997);
#10365=VERTEX_POINT('',#34999);
#10366=VERTEX_POINT('',#35003);
#10367=VERTEX_POINT('',#35005);
#10368=VERTEX_POINT('',#35009);
#10369=VERTEX_POINT('',#35011);
#10370=VERTEX_POINT('',#35015);
#10371=VERTEX_POINT('',#35017);
#10372=VERTEX_POINT('',#35021);
#10373=VERTEX_POINT('',#35023);
#10374=VERTEX_POINT('',#35027);
#10375=VERTEX_POINT('',#35029);
#10376=VERTEX_POINT('',#35033);
#10377=VERTEX_POINT('',#35035);
#10378=VERTEX_POINT('',#35039);
#10379=VERTEX_POINT('',#35041);
#10380=VERTEX_POINT('',#35045);
#10381=VERTEX_POINT('',#35049);
#10382=VERTEX_POINT('',#35050);
#10383=VERTEX_POINT('',#35052);
#10384=VERTEX_POINT('',#35054);
#10385=VERTEX_POINT('',#35058);
#10386=VERTEX_POINT('',#35069);
#10387=VERTEX_POINT('',#35082);
#10388=VERTEX_POINT('',#35093);
#10389=VERTEX_POINT('',#35106);
#10390=VERTEX_POINT('',#35108);
#10391=VERTEX_POINT('',#35112);
#10392=VERTEX_POINT('',#35114);
#10393=VERTEX_POINT('',#35118);
#10394=VERTEX_POINT('',#35129);
#10395=VERTEX_POINT('',#35142);
#10396=VERTEX_POINT('',#35153);
#10397=VERTEX_POINT('',#35180);
#10398=VERTEX_POINT('',#35182);
#10399=VERTEX_POINT('',#35186);
#10400=VERTEX_POINT('',#35188);
#10401=VERTEX_POINT('',#35192);
#10402=VERTEX_POINT('',#35194);
#10403=VERTEX_POINT('',#35198);
#10404=VERTEX_POINT('',#35200);
#10405=VERTEX_POINT('',#35204);
#10406=VERTEX_POINT('',#35206);
#10407=VERTEX_POINT('',#35210);
#10408=VERTEX_POINT('',#35212);
#10409=VERTEX_POINT('',#35216);
#10410=VERTEX_POINT('',#35218);
#10411=VERTEX_POINT('',#35222);
#10412=VERTEX_POINT('',#35223);
#10413=VERTEX_POINT('',#35225);
#10414=VERTEX_POINT('',#35227);
#10415=VERTEX_POINT('',#35229);
#10416=VERTEX_POINT('',#35231);
#10417=VERTEX_POINT('',#35233);
#10418=VERTEX_POINT('',#35237);
#10419=VERTEX_POINT('',#35238);
#10420=VERTEX_POINT('',#35240);
#10421=VERTEX_POINT('',#35242);
#10422=VERTEX_POINT('',#35244);
#10423=VERTEX_POINT('',#35246);
#10424=VERTEX_POINT('',#35248);
#10425=VERTEX_POINT('',#35252);
#10426=VERTEX_POINT('',#35253);
#10427=VERTEX_POINT('',#35255);
#10428=VERTEX_POINT('',#35257);
#10429=VERTEX_POINT('',#35259);
#10430=VERTEX_POINT('',#35261);
#10431=VERTEX_POINT('',#35263);
#10432=VERTEX_POINT('',#35267);
#10433=VERTEX_POINT('',#35268);
#10434=VERTEX_POINT('',#35270);
#10435=VERTEX_POINT('',#35272);
#10436=VERTEX_POINT('',#35274);
#10437=VERTEX_POINT('',#35276);
#10438=VERTEX_POINT('',#35278);
#10439=VERTEX_POINT('',#35282);
#10440=VERTEX_POINT('',#35284);
#10441=VERTEX_POINT('',#35288);
#10442=VERTEX_POINT('',#35290);
#10443=VERTEX_POINT('',#35294);
#10444=VERTEX_POINT('',#35296);
#10445=VERTEX_POINT('',#35300);
#10446=VERTEX_POINT('',#35302);
#10447=VERTEX_POINT('',#35306);
#10448=VERTEX_POINT('',#35308);
#10449=VERTEX_POINT('',#35312);
#10450=VERTEX_POINT('',#35314);
#10451=VERTEX_POINT('',#35318);
#10452=VERTEX_POINT('',#35320);
#10453=VERTEX_POINT('',#35324);
#10454=VERTEX_POINT('',#35326);
#10455=VERTEX_POINT('',#35334);
#10456=VERTEX_POINT('',#35335);
#10457=VERTEX_POINT('',#35337);
#10458=VERTEX_POINT('',#35339);
#10459=VERTEX_POINT('',#35341);
#10460=VERTEX_POINT('',#35343);
#10461=VERTEX_POINT('',#35345);
#10462=VERTEX_POINT('',#35347);
#10463=VERTEX_POINT('',#35349);
#10464=VERTEX_POINT('',#35351);
#10465=VERTEX_POINT('',#35353);
#10466=VERTEX_POINT('',#35355);
#10467=VERTEX_POINT('',#35358);
#10468=VERTEX_POINT('',#35359);
#10469=VERTEX_POINT('',#35361);
#10470=VERTEX_POINT('',#35363);
#10471=VERTEX_POINT('',#35365);
#10472=VERTEX_POINT('',#35367);
#10473=VERTEX_POINT('',#35369);
#10474=VERTEX_POINT('',#35371);
#10475=VERTEX_POINT('',#35375);
#10476=VERTEX_POINT('',#35376);
#10477=VERTEX_POINT('',#35381);
#10478=VERTEX_POINT('',#35385);
#10479=VERTEX_POINT('',#35389);
#10480=VERTEX_POINT('',#35393);
#10481=VERTEX_POINT('',#35397);
#10482=VERTEX_POINT('',#35401);
#10483=VERTEX_POINT('',#35405);
#10484=VERTEX_POINT('',#35409);
#10485=VERTEX_POINT('',#35413);
#10486=VERTEX_POINT('',#35417);
#10487=VERTEX_POINT('',#35424);
#10488=VERTEX_POINT('',#35425);
#10489=VERTEX_POINT('',#35427);
#10490=VERTEX_POINT('',#35429);
#10491=VERTEX_POINT('',#35431);
#10492=VERTEX_POINT('',#35433);
#10493=VERTEX_POINT('',#35435);
#10494=VERTEX_POINT('',#35437);
#10495=VERTEX_POINT('',#35457);
#10496=VERTEX_POINT('',#35458);
#10497=VERTEX_POINT('',#35460);
#10498=VERTEX_POINT('',#35462);
#10499=VERTEX_POINT('',#35464);
#10500=VERTEX_POINT('',#35466);
#10501=VERTEX_POINT('',#35470);
#10502=VERTEX_POINT('',#35471);
#10503=VERTEX_POINT('',#35473);
#10504=VERTEX_POINT('',#35475);
#10505=VERTEX_POINT('',#35477);
#10506=VERTEX_POINT('',#35479);
#10507=VERTEX_POINT('',#35483);
#10508=VERTEX_POINT('',#35484);
#10509=VERTEX_POINT('',#35486);
#10510=VERTEX_POINT('',#35488);
#10511=VERTEX_POINT('',#35490);
#10512=VERTEX_POINT('',#35492);
#10513=VERTEX_POINT('',#35496);
#10514=VERTEX_POINT('',#35497);
#10515=VERTEX_POINT('',#35499);
#10516=VERTEX_POINT('',#35501);
#10517=VERTEX_POINT('',#35503);
#10518=VERTEX_POINT('',#35505);
#10519=VERTEX_POINT('',#35509);
#10520=VERTEX_POINT('',#35512);
#10521=VERTEX_POINT('',#35517);
#10522=VERTEX_POINT('',#35522);
#10523=VERTEX_POINT('',#35527);
#10524=VERTEX_POINT('',#35532);
#10525=VERTEX_POINT('',#35545);
#10526=VERTEX_POINT('',#35548);
#10527=VERTEX_POINT('',#35553);
#10528=VERTEX_POINT('',#35558);
#10529=VERTEX_POINT('',#35563);
#10530=VERTEX_POINT('',#35568);
#10531=VERTEX_POINT('',#35581);
#10532=VERTEX_POINT('',#35584);
#10533=VERTEX_POINT('',#35589);
#10534=VERTEX_POINT('',#35594);
#10535=VERTEX_POINT('',#35599);
#10536=VERTEX_POINT('',#35604);
#10537=VERTEX_POINT('',#35617);
#10538=VERTEX_POINT('',#35620);
#10539=VERTEX_POINT('',#35625);
#10540=VERTEX_POINT('',#35630);
#10541=VERTEX_POINT('',#35635);
#10542=VERTEX_POINT('',#35640);
#10543=VERTEX_POINT('',#35658);
#10544=VERTEX_POINT('',#35693);
#10545=VERTEX_POINT('',#35730);
#10546=VERTEX_POINT('',#35731);
#10547=VERTEX_POINT('',#35733);
#10548=VERTEX_POINT('',#35738);
#10549=VERTEX_POINT('',#35740);
#10550=VERTEX_POINT('',#35746);
#10551=VERTEX_POINT('',#35747);
#10552=VERTEX_POINT('',#35749);
#10553=VERTEX_POINT('',#35751);
#10554=VERTEX_POINT('',#35755);
#10555=VERTEX_POINT('',#35757);
#10556=VERTEX_POINT('',#35761);
#10557=VERTEX_POINT('',#35762);
#10558=VERTEX_POINT('',#35764);
#10559=VERTEX_POINT('',#35766);
#10560=VERTEX_POINT('',#35770);
#10561=VERTEX_POINT('',#35771);
#10562=VERTEX_POINT('',#35773);
#10563=VERTEX_POINT('',#35775);
#10564=VERTEX_POINT('',#35779);
#10565=VERTEX_POINT('',#35780);
#10566=VERTEX_POINT('',#35782);
#10567=VERTEX_POINT('',#35784);
#10568=VERTEX_POINT('',#35803);
#10569=VERTEX_POINT('',#35805);
#10570=VERTEX_POINT('',#35809);
#10571=VERTEX_POINT('',#35810);
#10572=VERTEX_POINT('',#35812);
#10573=VERTEX_POINT('',#35820);
#10574=VERTEX_POINT('',#35821);
#10575=VERTEX_POINT('',#35823);
#10576=VERTEX_POINT('',#35825);
#10577=VERTEX_POINT('',#35827);
#10578=VERTEX_POINT('',#35829);
#10579=VERTEX_POINT('',#35833);
#10580=VERTEX_POINT('',#35835);
#10581=VERTEX_POINT('',#35839);
#10582=VERTEX_POINT('',#35843);
#10583=VERTEX_POINT('',#35847);
#10584=VERTEX_POINT('',#35851);
#10585=VERTEX_POINT('',#35859);
#10586=VERTEX_POINT('',#35861);
#10587=VERTEX_POINT('',#35865);
#10588=VERTEX_POINT('',#35867);
#10589=VERTEX_POINT('',#35879);
#10590=VERTEX_POINT('',#35881);
#10591=VERTEX_POINT('',#35885);
#10592=VERTEX_POINT('',#35887);
#10593=VERTEX_POINT('',#35891);
#10594=VERTEX_POINT('',#35893);
#10595=VERTEX_POINT('',#35897);
#10596=VERTEX_POINT('',#35898);
#10597=VERTEX_POINT('',#35900);
#10598=VERTEX_POINT('',#35902);
#10599=VERTEX_POINT('',#35904);
#10600=VERTEX_POINT('',#35906);
#10601=VERTEX_POINT('',#35908);
#10602=VERTEX_POINT('',#35910);
#10603=VERTEX_POINT('',#35912);
#10604=VERTEX_POINT('',#35914);
#10605=VERTEX_POINT('',#35916);
#10606=VERTEX_POINT('',#35918);
#10607=VERTEX_POINT('',#35922);
#10608=VERTEX_POINT('',#35923);
#10609=VERTEX_POINT('',#35925);
#10610=VERTEX_POINT('',#35927);
#10611=VERTEX_POINT('',#35929);
#10612=VERTEX_POINT('',#35931);
#10613=VERTEX_POINT('',#35933);
#10614=VERTEX_POINT('',#35935);
#10615=VERTEX_POINT('',#35937);
#10616=VERTEX_POINT('',#35939);
#10617=VERTEX_POINT('',#35941);
#10618=VERTEX_POINT('',#35943);
#10619=VERTEX_POINT('',#35971);
#10620=VERTEX_POINT('',#35973);
#10621=VERTEX_POINT('',#35977);
#10622=VERTEX_POINT('',#35981);
#10623=VERTEX_POINT('',#35985);
#10624=VERTEX_POINT('',#35987);
#10625=VERTEX_POINT('',#35991);
#10626=VERTEX_POINT('',#35993);
#10627=VERTEX_POINT('',#35997);
#10628=VERTEX_POINT('',#35999);
#10629=VERTEX_POINT('',#36003);
#10630=VERTEX_POINT('',#36007);
#10631=VERTEX_POINT('',#36011);
#10632=VERTEX_POINT('',#36013);
#10633=VERTEX_POINT('',#36017);
#10634=VERTEX_POINT('',#36019);
#10635=VERTEX_POINT('',#36030);
#10636=VERTEX_POINT('',#36032);
#10637=VERTEX_POINT('',#36036);
#10638=VERTEX_POINT('',#36038);
#10639=VERTEX_POINT('',#36042);
#10640=VERTEX_POINT('',#36043);
#10641=VERTEX_POINT('',#36045);
#10642=VERTEX_POINT('',#36047);
#10643=VERTEX_POINT('',#36051);
#10644=VERTEX_POINT('',#36052);
#10645=VERTEX_POINT('',#36054);
#10646=VERTEX_POINT('',#36056);
#10647=VERTEX_POINT('',#36060);
#10648=VERTEX_POINT('',#36061);
#10649=VERTEX_POINT('',#36063);
#10650=VERTEX_POINT('',#36065);
#10651=VERTEX_POINT('',#36068);
#10652=VERTEX_POINT('',#36070);
#10653=VERTEX_POINT('',#36072);
#10654=VERTEX_POINT('',#36074);
#10655=VERTEX_POINT('',#36079);
#10656=VERTEX_POINT('',#36080);
#10657=VERTEX_POINT('',#36083);
#10658=VERTEX_POINT('',#36085);
#10659=VERTEX_POINT('',#36087);
#10660=VERTEX_POINT('',#36089);
#10661=VERTEX_POINT('',#36092);
#10662=VERTEX_POINT('',#36094);
#10663=VERTEX_POINT('',#36119);
#10664=VERTEX_POINT('',#36121);
#10665=VERTEX_POINT('',#36125);
#10666=VERTEX_POINT('',#36127);
#10667=VERTEX_POINT('',#36131);
#10668=VERTEX_POINT('',#36133);
#10669=VERTEX_POINT('',#36137);
#10670=VERTEX_POINT('',#36139);
#10671=VERTEX_POINT('',#36143);
#10672=VERTEX_POINT('',#36144);
#10673=VERTEX_POINT('',#36146);
#10674=VERTEX_POINT('',#36148);
#10675=VERTEX_POINT('',#36152);
#10676=VERTEX_POINT('',#36154);
#10677=VERTEX_POINT('',#36156);
#10678=VERTEX_POINT('',#36158);
#10679=VERTEX_POINT('',#36162);
#10680=VERTEX_POINT('',#36163);
#10681=VERTEX_POINT('',#36166);
#10682=VERTEX_POINT('',#36170);
#10683=VERTEX_POINT('',#36171);
#10684=VERTEX_POINT('',#36173);
#10685=VERTEX_POINT('',#36176);
#10686=VERTEX_POINT('',#36180);
#10687=VERTEX_POINT('',#36182);
#10688=VERTEX_POINT('',#36187);
#10689=VERTEX_POINT('',#36192);
#10690=VERTEX_POINT('',#36198);
#10691=VERTEX_POINT('',#36206);
#10692=VERTEX_POINT('',#36208);
#10693=VERTEX_POINT('',#36212);
#10694=VERTEX_POINT('',#36214);
#10695=VERTEX_POINT('',#36218);
#10696=VERTEX_POINT('',#36220);
#10697=VERTEX_POINT('',#36224);
#10698=VERTEX_POINT('',#36226);
#10699=VERTEX_POINT('',#36230);
#10700=VERTEX_POINT('',#36231);
#10701=VERTEX_POINT('',#36233);
#10702=VERTEX_POINT('',#36235);
#10703=VERTEX_POINT('',#36239);
#10704=VERTEX_POINT('',#36241);
#10705=VERTEX_POINT('',#36243);
#10706=VERTEX_POINT('',#36245);
#10707=VERTEX_POINT('',#36249);
#10708=VERTEX_POINT('',#36250);
#10709=VERTEX_POINT('',#36253);
#10710=VERTEX_POINT('',#36257);
#10711=VERTEX_POINT('',#36258);
#10712=VERTEX_POINT('',#36260);
#10713=VERTEX_POINT('',#36263);
#10714=VERTEX_POINT('',#36267);
#10715=VERTEX_POINT('',#36269);
#10716=VERTEX_POINT('',#36274);
#10717=VERTEX_POINT('',#36279);
#10718=VERTEX_POINT('',#36285);
#10719=VERTEX_POINT('',#36293);
#10720=VERTEX_POINT('',#36295);
#10721=VERTEX_POINT('',#36299);
#10722=VERTEX_POINT('',#36301);
#10723=VERTEX_POINT('',#36305);
#10724=VERTEX_POINT('',#36307);
#10725=VERTEX_POINT('',#36311);
#10726=VERTEX_POINT('',#36313);
#10727=VERTEX_POINT('',#36317);
#10728=VERTEX_POINT('',#36319);
#10729=VERTEX_POINT('',#36323);
#10730=VERTEX_POINT('',#36325);
#10731=VERTEX_POINT('',#36329);
#10732=VERTEX_POINT('',#36331);
#10733=VERTEX_POINT('',#36335);
#10734=VERTEX_POINT('',#36337);
#10735=VERTEX_POINT('',#36341);
#10736=VERTEX_POINT('',#36343);
#10737=VERTEX_POINT('',#36347);
#10738=VERTEX_POINT('',#36349);
#10739=VERTEX_POINT('',#36353);
#10740=VERTEX_POINT('',#36355);
#10741=VERTEX_POINT('',#36359);
#10742=VERTEX_POINT('',#36361);
#10743=VERTEX_POINT('',#36365);
#10744=VERTEX_POINT('',#36366);
#10745=VERTEX_POINT('',#36368);
#10746=VERTEX_POINT('',#36370);
#10747=VERTEX_POINT('',#36374);
#10748=VERTEX_POINT('',#36375);
#10749=VERTEX_POINT('',#36380);
#10750=VERTEX_POINT('',#36384);
#10751=VERTEX_POINT('',#36397);
#10752=VERTEX_POINT('',#36400);
#10753=VERTEX_POINT('',#36404);
#10754=VERTEX_POINT('',#36406);
#10755=VERTEX_POINT('',#36410);
#10756=VERTEX_POINT('',#36413);
#10757=VERTEX_POINT('',#36417);
#10758=VERTEX_POINT('',#36418);
#10759=VERTEX_POINT('',#36420);
#10760=VERTEX_POINT('',#36463);
#10761=VERTEX_POINT('',#36486);
#10762=VERTEX_POINT('',#36591);
#10763=VERTEX_POINT('',#36593);
#10764=VERTEX_POINT('',#36677);
#10765=VERTEX_POINT('',#36678);
#10766=VERTEX_POINT('',#36680);
#10767=VERTEX_POINT('',#36688);
#10768=VERTEX_POINT('',#36831);
#10769=VERTEX_POINT('',#36905);
#10770=VERTEX_POINT('',#36963);
#10771=VERTEX_POINT('',#36964);
#10772=VERTEX_POINT('',#36966);
#10773=VERTEX_POINT('',#37113);
#10774=VERTEX_POINT('',#37203);
#10775=VERTEX_POINT('',#37427);
#10776=VERTEX_POINT('',#37539);
#10777=VERTEX_POINT('',#37674);
#10778=VERTEX_POINT('',#37675);
#10779=VERTEX_POINT('',#37830);
#10780=VERTEX_POINT('',#37892);
#10781=VERTEX_POINT('',#37893);
#10782=VERTEX_POINT('',#37895);
#10783=VERTEX_POINT('',#37903);
#10784=VERTEX_POINT('',#38045);
#10785=VERTEX_POINT('',#38068);
#10786=VERTEX_POINT('',#38081);
#10787=VERTEX_POINT('',#38507);
#10788=VERTEX_POINT('',#38668);
#10789=VERTEX_POINT('',#38669);
#10790=VERTEX_POINT('',#38719);
#10791=VERTEX_POINT('',#38727);
#10792=VERTEX_POINT('',#39209);
#10793=VERTEX_POINT('',#39210);
#10794=VERTEX_POINT('',#39212);
#10795=VERTEX_POINT('',#39220);
#10796=VERTEX_POINT('',#39363);
#10797=VERTEX_POINT('',#39437);
#10798=VERTEX_POINT('',#39495);
#10799=VERTEX_POINT('',#39496);
#10800=VERTEX_POINT('',#39498);
#10801=VERTEX_POINT('',#39645);
#10802=VERTEX_POINT('',#39733);
#10803=VERTEX_POINT('',#39957);
#10804=VERTEX_POINT('',#40069);
#10805=VERTEX_POINT('',#40213);
#10806=VERTEX_POINT('',#40214);
#10807=VERTEX_POINT('',#40369);
#10808=VERTEX_POINT('',#40431);
#10809=VERTEX_POINT('',#40432);
#10810=VERTEX_POINT('',#40434);
#10811=VERTEX_POINT('',#40442);
#10812=VERTEX_POINT('',#40584);
#10813=VERTEX_POINT('',#40607);
#10814=VERTEX_POINT('',#40620);
#10815=VERTEX_POINT('',#41046);
#10816=VERTEX_POINT('',#41207);
#10817=VERTEX_POINT('',#41208);
#10818=VERTEX_POINT('',#41258);
#10819=VERTEX_POINT('',#41266);
#10820=VERTEX_POINT('',#41769);
#10821=VERTEX_POINT('',#41770);
#10822=VERTEX_POINT('',#41772);
#10823=VERTEX_POINT('',#41780);
#10824=VERTEX_POINT('',#41923);
#10825=VERTEX_POINT('',#41997);
#10826=VERTEX_POINT('',#42055);
#10827=VERTEX_POINT('',#42056);
#10828=VERTEX_POINT('',#42058);
#10829=VERTEX_POINT('',#42205);
#10830=VERTEX_POINT('',#42294);
#10831=VERTEX_POINT('',#42518);
#10832=VERTEX_POINT('',#42634);
#10833=VERTEX_POINT('',#42754);
#10834=VERTEX_POINT('',#42755);
#10835=VERTEX_POINT('',#42907);
#10836=VERTEX_POINT('',#42969);
#10837=VERTEX_POINT('',#42970);
#10838=VERTEX_POINT('',#42972);
#10839=VERTEX_POINT('',#42980);
#10840=VERTEX_POINT('',#43122);
#10841=VERTEX_POINT('',#43145);
#10842=VERTEX_POINT('',#43158);
#10843=VERTEX_POINT('',#43584);
#10844=VERTEX_POINT('',#43745);
#10845=VERTEX_POINT('',#43746);
#10846=VERTEX_POINT('',#43796);
#10847=VERTEX_POINT('',#43804);
#10848=VERTEX_POINT('',#44295);
#10849=VERTEX_POINT('',#44296);
#10850=VERTEX_POINT('',#44298);
#10851=VERTEX_POINT('',#44306);
#10852=VERTEX_POINT('',#44452);
#10853=VERTEX_POINT('',#44526);
#10854=VERTEX_POINT('',#44584);
#10855=VERTEX_POINT('',#44585);
#10856=VERTEX_POINT('',#44587);
#10857=VERTEX_POINT('',#44734);
#10858=VERTEX_POINT('',#44824);
#10859=VERTEX_POINT('',#45048);
#10860=VERTEX_POINT('',#45160);
#10861=VERTEX_POINT('',#45286);
#10862=VERTEX_POINT('',#45287);
#10863=VERTEX_POINT('',#45442);
#10864=VERTEX_POINT('',#45500);
#10865=VERTEX_POINT('',#45501);
#10866=VERTEX_POINT('',#45503);
#10867=VERTEX_POINT('',#45520);
#10868=VERTEX_POINT('',#45656);
#10869=VERTEX_POINT('',#45679);
#10870=VERTEX_POINT('',#45692);
#10871=VERTEX_POINT('',#46118);
#10872=VERTEX_POINT('',#46275);
#10873=VERTEX_POINT('',#46276);
#10874=VERTEX_POINT('',#46326);
#10875=VERTEX_POINT('',#46343);
#10876=VERTEX_POINT('',#46781);
#10877=VERTEX_POINT('',#46782);
#10878=VERTEX_POINT('',#46784);
#10879=VERTEX_POINT('',#46803);
#10880=VERTEX_POINT('',#46805);
#10881=VERTEX_POINT('',#46818);
#10882=VERTEX_POINT('',#46865);
#10883=VERTEX_POINT('',#46939);
#10884=VERTEX_POINT('',#47068);
#10885=VERTEX_POINT('',#47070);
#10886=VERTEX_POINT('',#47158);
#10887=VERTEX_POINT('',#47159);
#10888=VERTEX_POINT('',#47321);
#10889=VERTEX_POINT('',#47597);
#10890=VERTEX_POINT('',#47688);
#10891=VERTEX_POINT('',#47731);
#10892=VERTEX_POINT('',#47842);
#10893=VERTEX_POINT('',#47935);
#10894=VERTEX_POINT('',#47936);
#10895=VERTEX_POINT('',#47938);
#10896=VERTEX_POINT('',#47946);
#10897=VERTEX_POINT('',#48092);
#10898=VERTEX_POINT('',#48166);
#10899=VERTEX_POINT('',#48224);
#10900=VERTEX_POINT('',#48225);
#10901=VERTEX_POINT('',#48227);
#10902=VERTEX_POINT('',#48374);
#10903=VERTEX_POINT('',#48462);
#10904=VERTEX_POINT('',#48686);
#10905=VERTEX_POINT('',#48810);
#10906=VERTEX_POINT('',#48957);
#10907=VERTEX_POINT('',#48958);
#10908=VERTEX_POINT('',#49110);
#10909=VERTEX_POINT('',#49172);
#10910=VERTEX_POINT('',#49173);
#10911=VERTEX_POINT('',#49175);
#10912=VERTEX_POINT('',#49183);
#10913=VERTEX_POINT('',#49325);
#10914=VERTEX_POINT('',#49348);
#10915=VERTEX_POINT('',#49361);
#10916=VERTEX_POINT('',#49787);
#10917=VERTEX_POINT('',#49948);
#10918=VERTEX_POINT('',#49949);
#10919=VERTEX_POINT('',#49996);
#10920=VERTEX_POINT('',#50004);
#10921=VERTEX_POINT('',#50492);
#10922=VERTEX_POINT('',#50493);
#10923=VERTEX_POINT('',#50653);
#10924=VERTEX_POINT('',#50656);
#10925=VERTEX_POINT('',#50660);
#10926=VERTEX_POINT('',#50663);
#10927=VERTEX_POINT('',#51246);
#10928=VERTEX_POINT('',#51423);
#10929=VERTEX_POINT('',#51645);
#10930=VERTEX_POINT('',#51648);
#10931=VERTEX_POINT('',#51652);
#10932=VERTEX_POINT('',#51655);
#10933=VERTEX_POINT('',#51661);
#10934=VERTEX_POINT('',#51663);
#10935=VERTEX_POINT('',#51664);
#10936=VERTEX_POINT('',#51666);
#10937=VERTEX_POINT('',#51668);
#10938=VERTEX_POINT('',#51670);
#10939=VERTEX_POINT('',#51672);
#10940=VERTEX_POINT('',#51676);
#10941=VERTEX_POINT('',#51681);
#10942=VERTEX_POINT('',#51682);
#10943=VERTEX_POINT('',#51684);
#10944=VERTEX_POINT('',#51686);
#10945=VERTEX_POINT('',#51688);
#10946=VERTEX_POINT('',#51690);
#10947=VERTEX_POINT('',#51707);
#10948=VERTEX_POINT('',#51708);
#10949=VERTEX_POINT('',#51710);
#10950=VERTEX_POINT('',#51712);
#10951=VERTEX_POINT('',#51716);
#10952=VERTEX_POINT('',#51718);
#10953=VERTEX_POINT('',#51719);
#10954=VERTEX_POINT('',#51721);
#10955=VERTEX_POINT('',#51723);
#10956=VERTEX_POINT('',#51727);
#10957=VERTEX_POINT('',#51731);
#10958=VERTEX_POINT('',#51732);
#10959=VERTEX_POINT('',#51734);
#10960=VERTEX_POINT('',#51753);
#10961=VERTEX_POINT('',#51757);
#10962=VERTEX_POINT('',#51758);
#10963=VERTEX_POINT('',#51760);
#10964=VERTEX_POINT('',#51762);
#10965=VERTEX_POINT('',#51766);
#10966=VERTEX_POINT('',#51767);
#10967=VERTEX_POINT('',#51769);
#10968=VERTEX_POINT('',#51771);
#10969=VERTEX_POINT('',#51775);
#10970=VERTEX_POINT('',#51776);
#10971=VERTEX_POINT('',#51781);
#10972=VERTEX_POINT('',#51783);
#10973=VERTEX_POINT('',#51787);
#10974=VERTEX_POINT('',#51789);
#10975=VERTEX_POINT('',#51793);
#10976=VERTEX_POINT('',#51797);
#10977=VERTEX_POINT('',#51801);
#10978=VERTEX_POINT('',#51805);
#10979=VERTEX_POINT('',#51807);
#10980=VERTEX_POINT('',#51809);
#10981=VERTEX_POINT('',#51811);
#10982=VERTEX_POINT('',#51816);
#10983=VERTEX_POINT('',#51817);
#10984=VERTEX_POINT('',#51819);
#10985=VERTEX_POINT('',#51821);
#10986=VERTEX_POINT('',#51836);
#10987=VERTEX_POINT('',#51841);
#10988=VERTEX_POINT('',#51843);
#10989=VERTEX_POINT('',#51862);
#10990=VERTEX_POINT('',#51886);
#10991=VERTEX_POINT('',#51887);
#10992=VERTEX_POINT('',#51904);
#10993=VERTEX_POINT('',#51906);
#10994=VERTEX_POINT('',#51908);
#10995=VERTEX_POINT('',#51910);
#10996=VERTEX_POINT('',#51912);
#10997=VERTEX_POINT('',#51914);
#10998=VERTEX_POINT('',#51916);
#10999=VERTEX_POINT('',#51919);
#11000=VERTEX_POINT('',#51920);
#11001=VERTEX_POINT('',#51922);
#11002=VERTEX_POINT('',#51924);
#11003=VERTEX_POINT('',#51926);
#11004=VERTEX_POINT('',#51928);
#11005=VERTEX_POINT('',#51930);
#11006=VERTEX_POINT('',#51932);
#11007=VERTEX_POINT('',#51935);
#11008=VERTEX_POINT('',#51936);
#11009=VERTEX_POINT('',#51938);
#11010=VERTEX_POINT('',#51940);
#11011=VERTEX_POINT('',#51942);
#11012=VERTEX_POINT('',#51944);
#11013=VERTEX_POINT('',#51947);
#11014=VERTEX_POINT('',#51948);
#11015=VERTEX_POINT('',#51950);
#11016=VERTEX_POINT('',#51952);
#11017=VERTEX_POINT('',#51954);
#11018=VERTEX_POINT('',#51956);
#11019=VERTEX_POINT('',#51958);
#11020=VERTEX_POINT('',#51960);
#11021=VERTEX_POINT('',#51962);
#11022=VERTEX_POINT('',#51964);
#11023=VERTEX_POINT('',#51966);
#11024=VERTEX_POINT('',#51969);
#11025=VERTEX_POINT('',#51970);
#11026=VERTEX_POINT('',#51972);
#11027=VERTEX_POINT('',#51974);
#11028=VERTEX_POINT('',#51976);
#11029=VERTEX_POINT('',#51978);
#11030=VERTEX_POINT('',#51982);
#11031=VERTEX_POINT('',#51983);
#11032=VERTEX_POINT('',#51985);
#11033=VERTEX_POINT('',#51987);
#11034=VERTEX_POINT('',#51989);
#11035=VERTEX_POINT('',#51991);
#11036=VERTEX_POINT('',#51993);
#11037=VERTEX_POINT('',#51995);
#11038=VERTEX_POINT('',#52015);
#11039=VERTEX_POINT('',#52017);
#11040=VERTEX_POINT('',#52021);
#11041=VERTEX_POINT('',#52025);
#11042=VERTEX_POINT('',#52029);
#11043=VERTEX_POINT('',#52031);
#11044=VERTEX_POINT('',#52035);
#11045=VERTEX_POINT('',#52039);
#11046=VERTEX_POINT('',#52043);
#11047=VERTEX_POINT('',#52047);
#11048=VERTEX_POINT('',#52051);
#11049=VERTEX_POINT('',#52060);
#11050=VERTEX_POINT('',#52061);
#11051=VERTEX_POINT('',#52063);
#11052=VERTEX_POINT('',#52065);
#11053=VERTEX_POINT('',#52067);
#11054=VERTEX_POINT('',#52069);
#11055=VERTEX_POINT('',#52085);
#11056=VERTEX_POINT('',#52087);
#11057=VERTEX_POINT('',#52091);
#11058=VERTEX_POINT('',#52095);
#11059=VERTEX_POINT('',#52099);
#11060=VERTEX_POINT('',#52103);
#11061=VERTEX_POINT('',#52110);
#11062=VERTEX_POINT('',#52112);
#11063=VERTEX_POINT('',#52116);
#11064=VERTEX_POINT('',#52120);
#11065=VERTEX_POINT('',#52124);
#11066=VERTEX_POINT('',#52143);
#11067=VERTEX_POINT('',#52147);
#11068=VERTEX_POINT('',#52149);
#11069=VERTEX_POINT('',#52153);
#11070=VERTEX_POINT('',#52157);
#11071=VERTEX_POINT('',#52161);
#11072=VERTEX_POINT('',#52165);
#11073=VERTEX_POINT('',#52171);
#11074=VERTEX_POINT('',#52196);
#11075=VERTEX_POINT('',#52198);
#11076=VERTEX_POINT('',#52199);
#11077=VERTEX_POINT('',#52201);
#11078=VERTEX_POINT('',#52203);
#11079=VERTEX_POINT('',#52205);
#11080=VERTEX_POINT('',#52207);
#11081=VERTEX_POINT('',#52211);
#11082=VERTEX_POINT('',#52216);
#11083=VERTEX_POINT('',#52217);
#11084=VERTEX_POINT('',#52219);
#11085=VERTEX_POINT('',#52221);
#11086=VERTEX_POINT('',#52223);
#11087=VERTEX_POINT('',#52225);
#11088=VERTEX_POINT('',#52242);
#11089=VERTEX_POINT('',#52243);
#11090=VERTEX_POINT('',#52245);
#11091=VERTEX_POINT('',#52247);
#11092=VERTEX_POINT('',#52251);
#11093=VERTEX_POINT('',#52253);
#11094=VERTEX_POINT('',#52254);
#11095=VERTEX_POINT('',#52256);
#11096=VERTEX_POINT('',#52258);
#11097=VERTEX_POINT('',#52262);
#11098=VERTEX_POINT('',#52266);
#11099=VERTEX_POINT('',#52267);
#11100=VERTEX_POINT('',#52269);
#11101=VERTEX_POINT('',#52288);
#11102=VERTEX_POINT('',#52292);
#11103=VERTEX_POINT('',#52293);
#11104=VERTEX_POINT('',#52295);
#11105=VERTEX_POINT('',#52297);
#11106=VERTEX_POINT('',#52301);
#11107=VERTEX_POINT('',#52302);
#11108=VERTEX_POINT('',#52304);
#11109=VERTEX_POINT('',#52306);
#11110=VERTEX_POINT('',#52310);
#11111=VERTEX_POINT('',#52311);
#11112=VERTEX_POINT('',#52316);
#11113=VERTEX_POINT('',#52318);
#11114=VERTEX_POINT('',#52322);
#11115=VERTEX_POINT('',#52324);
#11116=VERTEX_POINT('',#52328);
#11117=VERTEX_POINT('',#52332);
#11118=VERTEX_POINT('',#52336);
#11119=VERTEX_POINT('',#52340);
#11120=VERTEX_POINT('',#52342);
#11121=VERTEX_POINT('',#52344);
#11122=VERTEX_POINT('',#52346);
#11123=VERTEX_POINT('',#52351);
#11124=VERTEX_POINT('',#52352);
#11125=VERTEX_POINT('',#52354);
#11126=VERTEX_POINT('',#52356);
#11127=VERTEX_POINT('',#52366);
#11128=VERTEX_POINT('',#52368);
#11129=VERTEX_POINT('',#52381);
#11130=VERTEX_POINT('',#52383);
#11131=VERTEX_POINT('',#52396);
#11132=VERTEX_POINT('',#52400);
#11133=VERTEX_POINT('',#52404);
#11134=VERTEX_POINT('',#52408);
#11135=VERTEX_POINT('',#52410);
#11136=VERTEX_POINT('',#52418);
#11137=VERTEX_POINT('',#52420);
#11138=VERTEX_POINT('',#52439);
#11139=VERTEX_POINT('',#52463);
#11140=VERTEX_POINT('',#52464);
#11141=VERTEX_POINT('',#52481);
#11142=VERTEX_POINT('',#52483);
#11143=VERTEX_POINT('',#52485);
#11144=VERTEX_POINT('',#52487);
#11145=VERTEX_POINT('',#52489);
#11146=VERTEX_POINT('',#52491);
#11147=VERTEX_POINT('',#52493);
#11148=VERTEX_POINT('',#52496);
#11149=VERTEX_POINT('',#52497);
#11150=VERTEX_POINT('',#52499);
#11151=VERTEX_POINT('',#52501);
#11152=VERTEX_POINT('',#52503);
#11153=VERTEX_POINT('',#52505);
#11154=VERTEX_POINT('',#52507);
#11155=VERTEX_POINT('',#52509);
#11156=VERTEX_POINT('',#52512);
#11157=VERTEX_POINT('',#52513);
#11158=VERTEX_POINT('',#52515);
#11159=VERTEX_POINT('',#52517);
#11160=VERTEX_POINT('',#52519);
#11161=VERTEX_POINT('',#52521);
#11162=VERTEX_POINT('',#52524);
#11163=VERTEX_POINT('',#52525);
#11164=VERTEX_POINT('',#52527);
#11165=VERTEX_POINT('',#52529);
#11166=VERTEX_POINT('',#52531);
#11167=VERTEX_POINT('',#52533);
#11168=VERTEX_POINT('',#52535);
#11169=VERTEX_POINT('',#52537);
#11170=VERTEX_POINT('',#52539);
#11171=VERTEX_POINT('',#52541);
#11172=VERTEX_POINT('',#52543);
#11173=VERTEX_POINT('',#52546);
#11174=VERTEX_POINT('',#52547);
#11175=VERTEX_POINT('',#52549);
#11176=VERTEX_POINT('',#52551);
#11177=VERTEX_POINT('',#52553);
#11178=VERTEX_POINT('',#52555);
#11179=VERTEX_POINT('',#52559);
#11180=VERTEX_POINT('',#52560);
#11181=VERTEX_POINT('',#52562);
#11182=VERTEX_POINT('',#52564);
#11183=VERTEX_POINT('',#52566);
#11184=VERTEX_POINT('',#52568);
#11185=VERTEX_POINT('',#52570);
#11186=VERTEX_POINT('',#52572);
#11187=VERTEX_POINT('',#52592);
#11188=VERTEX_POINT('',#52594);
#11189=VERTEX_POINT('',#52598);
#11190=VERTEX_POINT('',#52602);
#11191=VERTEX_POINT('',#52606);
#11192=VERTEX_POINT('',#52608);
#11193=VERTEX_POINT('',#52612);
#11194=VERTEX_POINT('',#52616);
#11195=VERTEX_POINT('',#52620);
#11196=VERTEX_POINT('',#52624);
#11197=VERTEX_POINT('',#52628);
#11198=VERTEX_POINT('',#52637);
#11199=VERTEX_POINT('',#52638);
#11200=VERTEX_POINT('',#52640);
#11201=VERTEX_POINT('',#52642);
#11202=VERTEX_POINT('',#52644);
#11203=VERTEX_POINT('',#52646);
#11204=VERTEX_POINT('',#52662);
#11205=VERTEX_POINT('',#52664);
#11206=VERTEX_POINT('',#52668);
#11207=VERTEX_POINT('',#52672);
#11208=VERTEX_POINT('',#52676);
#11209=VERTEX_POINT('',#52680);
#11210=VERTEX_POINT('',#52687);
#11211=VERTEX_POINT('',#52689);
#11212=VERTEX_POINT('',#52693);
#11213=VERTEX_POINT('',#52697);
#11214=VERTEX_POINT('',#52701);
#11215=VERTEX_POINT('',#52720);
#11216=VERTEX_POINT('',#52724);
#11217=VERTEX_POINT('',#52726);
#11218=VERTEX_POINT('',#52730);
#11219=VERTEX_POINT('',#52734);
#11220=VERTEX_POINT('',#52738);
#11221=VERTEX_POINT('',#52742);
#11222=VERTEX_POINT('',#52748);
#11223=VERTEX_POINT('',#52780);
#11224=VERTEX_POINT('',#52782);
#11225=VERTEX_POINT('',#52786);
#11226=VERTEX_POINT('',#52788);
#11227=VERTEX_POINT('',#52792);
#11228=VERTEX_POINT('',#52794);
#11229=VERTEX_POINT('',#52798);
#11230=VERTEX_POINT('',#52800);
#11231=VERTEX_POINT('',#52804);
#11232=VERTEX_POINT('',#52806);
#11233=VERTEX_POINT('',#52810);
#11234=VERTEX_POINT('',#52812);
#11235=VERTEX_POINT('',#52816);
#11236=VERTEX_POINT('',#52818);
#11237=VERTEX_POINT('',#52822);
#11238=VERTEX_POINT('',#52823);
#11239=VERTEX_POINT('',#52825);
#11240=VERTEX_POINT('',#52827);
#11241=VERTEX_POINT('',#52829);
#11242=VERTEX_POINT('',#52831);
#11243=VERTEX_POINT('',#52835);
#11244=VERTEX_POINT('',#52836);
#11245=VERTEX_POINT('',#52841);
#11246=VERTEX_POINT('',#52842);
#11247=VERTEX_POINT('',#52845);
#11248=VERTEX_POINT('',#52847);
#11249=VERTEX_POINT('',#52861);
#11250=VERTEX_POINT('',#52863);
#11251=VERTEX_POINT('',#52867);
#11252=VERTEX_POINT('',#52869);
#11253=VERTEX_POINT('',#52873);
#11254=VERTEX_POINT('',#52875);
#11255=VERTEX_POINT('',#52879);
#11256=VERTEX_POINT('',#52881);
#11257=VERTEX_POINT('',#52885);
#11258=VERTEX_POINT('',#52887);
#11259=VERTEX_POINT('',#52891);
#11260=VERTEX_POINT('',#52893);
#11261=VERTEX_POINT('',#52897);
#11262=VERTEX_POINT('',#52898);
#11263=VERTEX_POINT('',#52900);
#11264=VERTEX_POINT('',#52902);
#11265=VERTEX_POINT('',#52906);
#11266=VERTEX_POINT('',#52908);
#11267=VERTEX_POINT('',#52912);
#11268=VERTEX_POINT('',#52914);
#11269=VERTEX_POINT('',#52926);
#11270=VERTEX_POINT('',#52928);
#11271=VERTEX_POINT('',#52932);
#11272=VERTEX_POINT('',#52934);
#11273=VERTEX_POINT('',#52938);
#11274=VERTEX_POINT('',#52940);
#11275=VERTEX_POINT('',#52944);
#11276=VERTEX_POINT('',#52946);
#11277=VERTEX_POINT('',#52950);
#11278=VERTEX_POINT('',#52952);
#11279=VERTEX_POINT('',#52956);
#11280=VERTEX_POINT('',#52958);
#11281=VERTEX_POINT('',#52962);
#11282=VERTEX_POINT('',#52963);
#11283=VERTEX_POINT('',#52965);
#11284=VERTEX_POINT('',#52967);
#11285=VERTEX_POINT('',#52971);
#11286=VERTEX_POINT('',#52973);
#11287=VERTEX_POINT('',#52977);
#11288=VERTEX_POINT('',#52979);
#11289=VERTEX_POINT('',#52989);
#11290=VERTEX_POINT('',#52990);
#11291=VERTEX_POINT('',#52992);
#11292=VERTEX_POINT('',#52994);
#11293=VERTEX_POINT('',#52998);
#11294=VERTEX_POINT('',#53000);
#11295=VERTEX_POINT('',#53004);
#11296=VERTEX_POINT('',#53006);
#11297=VERTEX_POINT('',#53010);
#11298=VERTEX_POINT('',#53012);
#11299=VERTEX_POINT('',#53021);
#11300=VERTEX_POINT('',#53022);
#11301=VERTEX_POINT('',#53024);
#11302=VERTEX_POINT('',#53026);
#11303=VERTEX_POINT('',#53030);
#11304=VERTEX_POINT('',#53032);
#11305=VERTEX_POINT('',#53036);
#11306=VERTEX_POINT('',#53038);
#11307=VERTEX_POINT('',#53042);
#11308=VERTEX_POINT('',#53044);
#11309=VERTEX_POINT('',#53053);
#11310=VERTEX_POINT('',#53054);
#11311=VERTEX_POINT('',#53056);
#11312=VERTEX_POINT('',#53058);
#11313=VERTEX_POINT('',#53062);
#11314=VERTEX_POINT('',#53064);
#11315=VERTEX_POINT('',#53068);
#11316=VERTEX_POINT('',#53070);
#11317=VERTEX_POINT('',#53074);
#11318=VERTEX_POINT('',#53076);
#11319=VERTEX_POINT('',#53080);
#11320=VERTEX_POINT('',#53082);
#11321=VERTEX_POINT('',#53086);
#11322=VERTEX_POINT('',#53088);
#11323=VERTEX_POINT('',#53092);
#11324=VERTEX_POINT('',#53094);
#11325=VERTEX_POINT('',#53098);
#11326=VERTEX_POINT('',#53100);
#11327=VERTEX_POINT('',#53104);
#11328=VERTEX_POINT('',#53106);
#11329=VERTEX_POINT('',#53110);
#11330=VERTEX_POINT('',#53112);
#11331=VERTEX_POINT('',#53116);
#11332=VERTEX_POINT('',#53118);
#11333=VERTEX_POINT('',#53122);
#11334=VERTEX_POINT('',#53124);
#11335=VERTEX_POINT('',#53128);
#11336=VERTEX_POINT('',#53130);
#11337=VERTEX_POINT('',#53134);
#11338=VERTEX_POINT('',#53136);
#11339=VERTEX_POINT('',#53140);
#11340=VERTEX_POINT('',#53142);
#11341=VERTEX_POINT('',#53146);
#11342=VERTEX_POINT('',#53148);
#11343=VERTEX_POINT('',#53152);
#11344=VERTEX_POINT('',#53154);
#11345=VERTEX_POINT('',#53158);
#11346=VERTEX_POINT('',#53160);
#11347=VERTEX_POINT('',#53164);
#11348=VERTEX_POINT('',#53166);
#11349=VERTEX_POINT('',#53170);
#11350=VERTEX_POINT('',#53172);
#11351=VERTEX_POINT('',#53176);
#11352=VERTEX_POINT('',#53178);
#11353=VERTEX_POINT('',#53182);
#11354=VERTEX_POINT('',#53184);
#11355=VERTEX_POINT('',#53188);
#11356=VERTEX_POINT('',#53190);
#11357=VERTEX_POINT('',#53194);
#11358=VERTEX_POINT('',#53196);
#11359=VERTEX_POINT('',#53200);
#11360=VERTEX_POINT('',#53202);
#11361=VERTEX_POINT('',#53206);
#11362=VERTEX_POINT('',#53208);
#11363=VERTEX_POINT('',#53212);
#11364=VERTEX_POINT('',#53214);
#11365=VERTEX_POINT('',#53218);
#11366=VERTEX_POINT('',#53220);
#11367=VERTEX_POINT('',#53224);
#11368=VERTEX_POINT('',#53226);
#11369=VERTEX_POINT('',#53230);
#11370=VERTEX_POINT('',#53232);
#11371=VERTEX_POINT('',#53236);
#11372=VERTEX_POINT('',#53238);
#11373=VERTEX_POINT('',#53242);
#11374=VERTEX_POINT('',#53244);
#11375=VERTEX_POINT('',#53248);
#11376=VERTEX_POINT('',#53250);
#11377=VERTEX_POINT('',#53254);
#11378=VERTEX_POINT('',#53256);
#11379=VERTEX_POINT('',#53260);
#11380=VERTEX_POINT('',#53262);
#11381=VERTEX_POINT('',#53266);
#11382=VERTEX_POINT('',#53268);
#11383=VERTEX_POINT('',#53272);
#11384=VERTEX_POINT('',#53274);
#11385=VERTEX_POINT('',#53278);
#11386=VERTEX_POINT('',#53280);
#11387=VERTEX_POINT('',#53284);
#11388=VERTEX_POINT('',#53286);
#11389=VERTEX_POINT('',#53290);
#11390=VERTEX_POINT('',#53292);
#11391=VERTEX_POINT('',#53296);
#11392=VERTEX_POINT('',#53298);
#11393=VERTEX_POINT('',#53302);
#11394=VERTEX_POINT('',#53304);
#11395=VERTEX_POINT('',#53308);
#11396=VERTEX_POINT('',#53310);
#11397=VERTEX_POINT('',#53314);
#11398=VERTEX_POINT('',#53316);
#11399=VERTEX_POINT('',#53320);
#11400=VERTEX_POINT('',#53322);
#11401=VERTEX_POINT('',#53326);
#11402=VERTEX_POINT('',#53328);
#11403=VERTEX_POINT('',#53332);
#11404=VERTEX_POINT('',#53334);
#11405=VERTEX_POINT('',#53338);
#11406=VERTEX_POINT('',#53340);
#11407=VERTEX_POINT('',#53344);
#11408=VERTEX_POINT('',#53346);
#11409=VERTEX_POINT('',#53350);
#11410=VERTEX_POINT('',#53351);
#11411=VERTEX_POINT('',#53353);
#11412=VERTEX_POINT('',#53355);
#11413=VERTEX_POINT('',#53357);
#11414=VERTEX_POINT('',#53359);
#11415=VERTEX_POINT('',#53361);
#11416=VERTEX_POINT('',#53363);
#11417=VERTEX_POINT('',#53367);
#11418=VERTEX_POINT('',#53368);
#11419=VERTEX_POINT('',#53370);
#11420=VERTEX_POINT('',#53372);
#11421=VERTEX_POINT('',#53376);
#11422=VERTEX_POINT('',#53377);
#11423=VERTEX_POINT('',#53379);
#11424=VERTEX_POINT('',#53381);
#11425=VERTEX_POINT('',#53385);
#11426=VERTEX_POINT('',#53386);
#11427=VERTEX_POINT('',#53388);
#11428=VERTEX_POINT('',#53390);
#11429=VERTEX_POINT('',#53397);
#11430=VERTEX_POINT('',#53399);
#11431=VERTEX_POINT('',#53406);
#11432=VERTEX_POINT('',#53408);
#11433=VERTEX_POINT('',#53412);
#11434=VERTEX_POINT('',#53413);
#11435=VERTEX_POINT('',#53415);
#11436=VERTEX_POINT('',#53417);
#11437=VERTEX_POINT('',#53419);
#11438=VERTEX_POINT('',#53421);
#11439=VERTEX_POINT('',#53423);
#11440=VERTEX_POINT('',#53425);
#11441=VERTEX_POINT('',#53471);
#11442=VERTEX_POINT('',#53473);
#11443=VERTEX_POINT('',#53477);
#11444=VERTEX_POINT('',#53478);
#11445=VERTEX_POINT('',#53480);
#11446=VERTEX_POINT('',#53482);
#11447=VERTEX_POINT('',#53484);
#11448=VERTEX_POINT('',#53486);
#11449=VERTEX_POINT('',#53488);
#11450=VERTEX_POINT('',#53491);
#11451=VERTEX_POINT('',#53493);
#11452=VERTEX_POINT('',#53495);
#11453=VERTEX_POINT('',#53499);
#11454=VERTEX_POINT('',#53501);
#11455=VERTEX_POINT('',#53505);
#11456=VERTEX_POINT('',#53506);
#11457=VERTEX_POINT('',#53508);
#11458=VERTEX_POINT('',#53510);
#11459=VERTEX_POINT('',#53512);
#11460=VERTEX_POINT('',#53514);
#11461=VERTEX_POINT('',#53516);
#11462=VERTEX_POINT('',#53519);
#11463=VERTEX_POINT('',#53521);
#11464=VERTEX_POINT('',#53523);
#11465=VERTEX_POINT('',#53527);
#11466=VERTEX_POINT('',#53529);
#11467=VERTEX_POINT('',#53533);
#11468=VERTEX_POINT('',#53534);
#11469=VERTEX_POINT('',#53536);
#11470=VERTEX_POINT('',#53538);
#11471=VERTEX_POINT('',#53540);
#11472=VERTEX_POINT('',#53542);
#11473=VERTEX_POINT('',#53544);
#11474=VERTEX_POINT('',#53547);
#11475=VERTEX_POINT('',#53549);
#11476=VERTEX_POINT('',#53551);
#11477=VERTEX_POINT('',#53555);
#11478=VERTEX_POINT('',#53557);
#11479=VERTEX_POINT('',#53561);
#11480=VERTEX_POINT('',#53562);
#11481=VERTEX_POINT('',#53564);
#11482=VERTEX_POINT('',#53566);
#11483=VERTEX_POINT('',#53568);
#11484=VERTEX_POINT('',#53570);
#11485=VERTEX_POINT('',#53572);
#11486=VERTEX_POINT('',#53575);
#11487=VERTEX_POINT('',#53577);
#11488=VERTEX_POINT('',#53579);
#11489=VERTEX_POINT('',#53583);
#11490=VERTEX_POINT('',#53585);
#11491=VERTEX_POINT('',#53589);
#11492=VERTEX_POINT('',#53590);
#11493=VERTEX_POINT('',#53592);
#11494=VERTEX_POINT('',#53594);
#11495=VERTEX_POINT('',#53596);
#11496=VERTEX_POINT('',#53598);
#11497=VERTEX_POINT('',#53600);
#11498=VERTEX_POINT('',#53603);
#11499=VERTEX_POINT('',#53605);
#11500=VERTEX_POINT('',#53607);
#11501=VERTEX_POINT('',#53611);
#11502=VERTEX_POINT('',#53613);
#11503=VERTEX_POINT('',#53617);
#11504=VERTEX_POINT('',#53618);
#11505=VERTEX_POINT('',#53620);
#11506=VERTEX_POINT('',#53622);
#11507=VERTEX_POINT('',#53624);
#11508=VERTEX_POINT('',#53626);
#11509=VERTEX_POINT('',#53628);
#11510=VERTEX_POINT('',#53631);
#11511=VERTEX_POINT('',#53633);
#11512=VERTEX_POINT('',#53635);
#11513=VERTEX_POINT('',#53639);
#11514=VERTEX_POINT('',#53641);
#11515=VERTEX_POINT('',#53645);
#11516=VERTEX_POINT('',#53646);
#11517=VERTEX_POINT('',#53648);
#11518=VERTEX_POINT('',#53650);
#11519=VERTEX_POINT('',#53652);
#11520=VERTEX_POINT('',#53654);
#11521=VERTEX_POINT('',#53656);
#11522=VERTEX_POINT('',#53659);
#11523=VERTEX_POINT('',#53661);
#11524=VERTEX_POINT('',#53663);
#11525=VERTEX_POINT('',#53667);
#11526=VERTEX_POINT('',#53669);
#11527=VERTEX_POINT('',#53673);
#11528=VERTEX_POINT('',#53674);
#11529=VERTEX_POINT('',#53676);
#11530=VERTEX_POINT('',#53678);
#11531=VERTEX_POINT('',#53680);
#11532=VERTEX_POINT('',#53682);
#11533=VERTEX_POINT('',#53684);
#11534=VERTEX_POINT('',#53687);
#11535=VERTEX_POINT('',#53689);
#11536=VERTEX_POINT('',#53691);
#11537=VERTEX_POINT('',#53695);
#11538=VERTEX_POINT('',#53697);
#11539=VERTEX_POINT('',#53713);
#11540=VERTEX_POINT('',#53715);
#11541=VERTEX_POINT('',#53717);
#11542=VERTEX_POINT('',#53721);
#11543=VERTEX_POINT('',#53723);
#11544=VERTEX_POINT('',#53725);
#11545=VERTEX_POINT('',#53727);
#11546=VERTEX_POINT('',#53768);
#11547=VERTEX_POINT('',#53770);
#11548=VERTEX_POINT('',#53776);
#11549=VERTEX_POINT('',#53778);
#11550=VERTEX_POINT('',#53780);
#11551=VERTEX_POINT('',#53782);
#11552=VERTEX_POINT('',#53784);
#11553=VERTEX_POINT('',#53786);
#11554=VERTEX_POINT('',#53788);
#11555=VERTEX_POINT('',#53790);
#11556=VERTEX_POINT('',#53792);
#11557=VERTEX_POINT('',#53794);
#11558=VERTEX_POINT('',#53796);
#11559=VERTEX_POINT('',#53798);
#11560=VERTEX_POINT('',#53800);
#11561=VERTEX_POINT('',#53802);
#11562=VERTEX_POINT('',#53804);
#11563=VERTEX_POINT('',#53806);
#11564=VERTEX_POINT('',#53808);
#11565=VERTEX_POINT('',#53810);
#11566=VERTEX_POINT('',#53812);
#11567=VERTEX_POINT('',#53814);
#11568=VERTEX_POINT('',#53816);
#11569=VERTEX_POINT('',#53818);
#11570=VERTEX_POINT('',#53820);
#11571=VERTEX_POINT('',#53822);
#11572=VERTEX_POINT('',#53824);
#11573=VERTEX_POINT('',#53826);
#11574=VERTEX_POINT('',#53828);
#11575=VERTEX_POINT('',#53830);
#11576=VERTEX_POINT('',#53832);
#11577=VERTEX_POINT('',#53834);
#11578=VERTEX_POINT('',#53836);
#11579=VERTEX_POINT('',#53838);
#11580=VERTEX_POINT('',#53840);
#11581=VERTEX_POINT('',#53842);
#11582=VERTEX_POINT('',#53844);
#11583=VERTEX_POINT('',#53846);
#11584=VERTEX_POINT('',#53848);
#11585=VERTEX_POINT('',#53850);
#11586=VERTEX_POINT('',#53852);
#11587=VERTEX_POINT('',#53854);
#11588=VERTEX_POINT('',#53857);
#11589=VERTEX_POINT('',#53862);
#11590=VERTEX_POINT('',#53864);
#11591=VERTEX_POINT('',#53866);
#11592=VERTEX_POINT('',#53868);
#11593=VERTEX_POINT('',#53870);
#11594=VERTEX_POINT('',#53872);
#11595=VERTEX_POINT('',#53874);
#11596=VERTEX_POINT('',#53876);
#11597=VERTEX_POINT('',#53878);
#11598=VERTEX_POINT('',#53880);
#11599=VERTEX_POINT('',#53882);
#11600=VERTEX_POINT('',#53884);
#11601=VERTEX_POINT('',#53886);
#11602=VERTEX_POINT('',#53888);
#11603=VERTEX_POINT('',#53890);
#11604=VERTEX_POINT('',#53892);
#11605=VERTEX_POINT('',#53894);
#11606=VERTEX_POINT('',#53896);
#11607=VERTEX_POINT('',#53898);
#11608=VERTEX_POINT('',#53900);
#11609=VERTEX_POINT('',#53902);
#11610=VERTEX_POINT('',#53904);
#11611=VERTEX_POINT('',#53906);
#11612=VERTEX_POINT('',#53908);
#11613=VERTEX_POINT('',#53910);
#11614=VERTEX_POINT('',#53912);
#11615=VERTEX_POINT('',#53914);
#11616=VERTEX_POINT('',#53916);
#11617=VERTEX_POINT('',#53918);
#11618=VERTEX_POINT('',#53920);
#11619=VERTEX_POINT('',#53922);
#11620=VERTEX_POINT('',#53924);
#11621=VERTEX_POINT('',#53926);
#11622=VERTEX_POINT('',#53928);
#11623=VERTEX_POINT('',#53930);
#11624=VERTEX_POINT('',#53932);
#11625=VERTEX_POINT('',#53934);
#11626=VERTEX_POINT('',#53936);
#11627=VERTEX_POINT('',#53938);
#11628=VERTEX_POINT('',#53940);
#11629=VERTEX_POINT('',#54038);
#11630=VERTEX_POINT('',#54040);
#11631=VERTEX_POINT('',#54044);
#11632=VERTEX_POINT('',#54046);
#11633=VERTEX_POINT('',#54050);
#11634=VERTEX_POINT('',#54052);
#11635=VERTEX_POINT('',#54056);
#11636=VERTEX_POINT('',#54059);
#11637=VERTEX_POINT('',#54062);
#11638=VERTEX_POINT('',#54064);
#11639=VERTEX_POINT('',#54068);
#11640=VERTEX_POINT('',#54070);
#11641=VERTEX_POINT('',#54074);
#11642=VERTEX_POINT('',#54076);
#11643=VERTEX_POINT('',#54080);
#11644=VERTEX_POINT('',#54082);
#11645=VERTEX_POINT('',#54086);
#11646=VERTEX_POINT('',#54088);
#11647=VERTEX_POINT('',#54092);
#11648=VERTEX_POINT('',#54094);
#11649=VERTEX_POINT('',#54098);
#11650=VERTEX_POINT('',#54100);
#11651=VERTEX_POINT('',#54104);
#11652=VERTEX_POINT('',#54106);
#11653=VERTEX_POINT('',#54108);
#11654=VERTEX_POINT('',#54110);
#11655=VERTEX_POINT('',#54112);
#11656=VERTEX_POINT('',#54116);
#11657=VERTEX_POINT('',#54119);
#11658=VERTEX_POINT('',#54122);
#11659=VERTEX_POINT('',#54124);
#11660=VERTEX_POINT('',#54126);
#11661=VERTEX_POINT('',#54128);
#11662=VERTEX_POINT('',#54130);
#11663=VERTEX_POINT('',#54160);
#11664=VERTEX_POINT('',#54161);
#11665=VERTEX_POINT('',#54172);
#11666=VERTEX_POINT('',#54183);
#11667=VERTEX_POINT('',#54194);
#11668=VERTEX_POINT('',#54198);
#11669=VERTEX_POINT('',#54201);
#11670=VERTEX_POINT('',#54212);
#11671=VERTEX_POINT('',#54234);
#11672=VERTEX_POINT('',#54238);
#11673=VERTEX_POINT('',#54240);
#11674=VERTEX_POINT('',#54244);
#11675=VERTEX_POINT('',#54245);
#11676=VERTEX_POINT('',#54247);
#11677=VERTEX_POINT('',#54249);
#11678=VERTEX_POINT('',#54253);
#11679=VERTEX_POINT('',#54255);
#11680=VERTEX_POINT('',#54257);
#11681=VERTEX_POINT('',#54261);
#11682=VERTEX_POINT('',#54262);
#11683=VERTEX_POINT('',#54264);
#11684=VERTEX_POINT('',#54266);
#11685=VERTEX_POINT('',#54270);
#11686=VERTEX_POINT('',#54272);
#11687=VERTEX_POINT('',#54274);
#11688=VERTEX_POINT('',#54278);
#11689=VERTEX_POINT('',#54279);
#11690=VERTEX_POINT('',#54281);
#11691=VERTEX_POINT('',#54283);
#11692=VERTEX_POINT('',#54287);
#11693=VERTEX_POINT('',#54288);
#11694=VERTEX_POINT('',#54290);
#11695=VERTEX_POINT('',#54292);
#11696=VERTEX_POINT('',#54296);
#11697=VERTEX_POINT('',#54297);
#11698=VERTEX_POINT('',#54299);
#11699=VERTEX_POINT('',#54301);
#11700=VERTEX_POINT('',#54305);
#11701=VERTEX_POINT('',#54306);
#11702=VERTEX_POINT('',#54308);
#11703=VERTEX_POINT('',#54310);
#11704=VERTEX_POINT('',#54314);
#11705=VERTEX_POINT('',#54315);
#11706=VERTEX_POINT('',#54317);
#11707=VERTEX_POINT('',#54319);
#11708=VERTEX_POINT('',#54323);
#11709=VERTEX_POINT('',#54324);
#11710=VERTEX_POINT('',#54326);
#11711=VERTEX_POINT('',#54328);
#11712=VERTEX_POINT('',#54332);
#11713=VERTEX_POINT('',#54333);
#11714=VERTEX_POINT('',#54335);
#11715=VERTEX_POINT('',#54337);
#11716=VERTEX_POINT('',#54341);
#11717=VERTEX_POINT('',#54342);
#11718=VERTEX_POINT('',#54344);
#11719=VERTEX_POINT('',#54346);
#11720=VERTEX_POINT('',#54350);
#11721=VERTEX_POINT('',#54351);
#11722=VERTEX_POINT('',#54353);
#11723=VERTEX_POINT('',#54355);
#11724=VERTEX_POINT('',#54359);
#11725=VERTEX_POINT('',#54361);
#11726=VERTEX_POINT('',#54365);
#11727=VERTEX_POINT('',#54366);
#11728=VERTEX_POINT('',#54368);
#11729=VERTEX_POINT('',#54370);
#11730=VERTEX_POINT('',#54374);
#11731=VERTEX_POINT('',#54376);
#11732=VERTEX_POINT('',#54380);
#11733=VERTEX_POINT('',#54381);
#11734=VERTEX_POINT('',#54383);
#11735=VERTEX_POINT('',#54385);
#11736=VERTEX_POINT('',#54389);
#11737=VERTEX_POINT('',#54390);
#11738=VERTEX_POINT('',#54392);
#11739=VERTEX_POINT('',#54394);
#11740=VERTEX_POINT('',#54398);
#11741=VERTEX_POINT('',#54399);
#11742=VERTEX_POINT('',#54401);
#11743=VERTEX_POINT('',#54403);
#11744=VERTEX_POINT('',#54407);
#11745=VERTEX_POINT('',#54408);
#11746=VERTEX_POINT('',#54410);
#11747=VERTEX_POINT('',#54412);
#11748=VERTEX_POINT('',#54419);
#11749=VERTEX_POINT('',#54420);
#11750=VERTEX_POINT('',#54422);
#11751=VERTEX_POINT('',#54424);
#11752=VERTEX_POINT('',#54428);
#11753=VERTEX_POINT('',#54429);
#11754=VERTEX_POINT('',#54431);
#11755=VERTEX_POINT('',#54433);
#11756=VERTEX_POINT('',#54437);
#11757=VERTEX_POINT('',#54438);
#11758=VERTEX_POINT('',#54440);
#11759=VERTEX_POINT('',#54442);
#11760=VERTEX_POINT('',#54446);
#11761=VERTEX_POINT('',#54447);
#11762=VERTEX_POINT('',#54449);
#11763=VERTEX_POINT('',#54451);
#11764=VERTEX_POINT('',#54504);
#11765=VERTEX_POINT('',#54505);
#11766=VERTEX_POINT('',#54507);
#11767=VERTEX_POINT('',#54509);
#11768=VERTEX_POINT('',#54513);
#11769=VERTEX_POINT('',#54515);
#11770=VERTEX_POINT('',#54518);
#11771=VERTEX_POINT('',#54520);
#11772=VERTEX_POINT('',#54524);
#11773=VERTEX_POINT('',#54528);
#11774=VERTEX_POINT('',#54534);
#11775=VERTEX_POINT('',#54538);
#11776=VERTEX_POINT('',#54544);
#11777=VERTEX_POINT('',#54546);
#11778=VERTEX_POINT('',#54550);
#11779=VERTEX_POINT('',#54554);
#11780=VERTEX_POINT('',#54558);
#11781=VERTEX_POINT('',#54562);
#11782=VERTEX_POINT('',#54569);
#11783=VERTEX_POINT('',#54570);
#11784=VERTEX_POINT('',#54572);
#11785=VERTEX_POINT('',#54574);
#11786=VERTEX_POINT('',#54576);
#11787=VERTEX_POINT('',#54578);
#11788=VERTEX_POINT('',#54580);
#11789=VERTEX_POINT('',#54582);
#11790=VERTEX_POINT('',#54584);
#11791=VERTEX_POINT('',#54586);
#11792=VERTEX_POINT('',#54588);
#11793=VERTEX_POINT('',#54590);
#11794=VERTEX_POINT('',#54592);
#11795=VERTEX_POINT('',#54594);
#11796=VERTEX_POINT('',#54596);
#11797=VERTEX_POINT('',#54598);
#11798=VERTEX_POINT('',#54600);
#11799=VERTEX_POINT('',#54602);
#11800=VERTEX_POINT('',#54604);
#11801=VERTEX_POINT('',#54606);
#11802=VERTEX_POINT('',#54608);
#11803=VERTEX_POINT('',#54610);
#11804=VERTEX_POINT('',#54612);
#11805=VERTEX_POINT('',#54614);
#11806=VERTEX_POINT('',#54616);
#11807=VERTEX_POINT('',#54618);
#11808=VERTEX_POINT('',#54620);
#11809=VERTEX_POINT('',#54622);
#11810=VERTEX_POINT('',#54624);
#11811=VERTEX_POINT('',#54626);
#11812=VERTEX_POINT('',#54628);
#11813=VERTEX_POINT('',#54630);
#11814=VERTEX_POINT('',#54632);
#11815=VERTEX_POINT('',#54634);
#11816=VERTEX_POINT('',#54636);
#11817=VERTEX_POINT('',#54638);
#11818=VERTEX_POINT('',#54640);
#11819=VERTEX_POINT('',#54642);
#11820=VERTEX_POINT('',#54644);
#11821=VERTEX_POINT('',#54646);
#11822=VERTEX_POINT('',#54648);
#11823=VERTEX_POINT('',#54650);
#11824=VERTEX_POINT('',#54652);
#11825=VERTEX_POINT('',#54654);
#11826=VERTEX_POINT('',#54658);
#11827=VERTEX_POINT('',#54659);
#11828=VERTEX_POINT('',#54664);
#11829=VERTEX_POINT('',#54668);
#11830=VERTEX_POINT('',#54672);
#11831=VERTEX_POINT('',#54676);
#11832=VERTEX_POINT('',#54680);
#11833=VERTEX_POINT('',#54684);
#11834=VERTEX_POINT('',#54688);
#11835=VERTEX_POINT('',#54692);
#11836=VERTEX_POINT('',#54696);
#11837=VERTEX_POINT('',#54700);
#11838=VERTEX_POINT('',#54704);
#11839=VERTEX_POINT('',#54708);
#11840=VERTEX_POINT('',#54712);
#11841=VERTEX_POINT('',#54716);
#11842=VERTEX_POINT('',#54720);
#11843=VERTEX_POINT('',#54724);
#11844=VERTEX_POINT('',#54728);
#11845=VERTEX_POINT('',#54732);
#11846=VERTEX_POINT('',#54736);
#11847=VERTEX_POINT('',#54740);
#11848=VERTEX_POINT('',#54744);
#11849=VERTEX_POINT('',#54748);
#11850=VERTEX_POINT('',#54752);
#11851=VERTEX_POINT('',#54756);
#11852=VERTEX_POINT('',#54760);
#11853=VERTEX_POINT('',#54764);
#11854=VERTEX_POINT('',#54768);
#11855=VERTEX_POINT('',#54772);
#11856=VERTEX_POINT('',#54776);
#11857=VERTEX_POINT('',#54780);
#11858=VERTEX_POINT('',#54784);
#11859=VERTEX_POINT('',#54788);
#11860=VERTEX_POINT('',#54792);
#11861=VERTEX_POINT('',#54796);
#11862=VERTEX_POINT('',#54800);
#11863=VERTEX_POINT('',#54804);
#11864=VERTEX_POINT('',#54808);
#11865=VERTEX_POINT('',#54812);
#11866=VERTEX_POINT('',#54816);
#11867=VERTEX_POINT('',#54820);
#11868=VERTEX_POINT('',#54824);
#11869=VERTEX_POINT('',#54828);
#11870=VERTEX_POINT('',#54835);
#11871=VERTEX_POINT('',#54837);
#11872=VERTEX_POINT('',#54841);
#11873=VERTEX_POINT('',#54842);
#11874=VERTEX_POINT('',#54844);
#11875=VERTEX_POINT('',#54846);
#11876=VERTEX_POINT('',#54848);
#11877=VERTEX_POINT('',#54850);
#11878=VERTEX_POINT('',#54852);
#11879=VERTEX_POINT('',#54854);
#11880=VERTEX_POINT('',#54856);
#11881=VERTEX_POINT('',#54858);
#11882=VERTEX_POINT('',#54860);
#11883=VERTEX_POINT('',#54862);
#11884=VERTEX_POINT('',#54864);
#11885=VERTEX_POINT('',#54866);
#11886=VERTEX_POINT('',#54868);
#11887=VERTEX_POINT('',#54870);
#11888=VERTEX_POINT('',#54872);
#11889=VERTEX_POINT('',#54874);
#11890=VERTEX_POINT('',#54876);
#11891=VERTEX_POINT('',#54878);
#11892=VERTEX_POINT('',#54880);
#11893=VERTEX_POINT('',#54882);
#11894=VERTEX_POINT('',#54884);
#11895=VERTEX_POINT('',#54886);
#11896=VERTEX_POINT('',#54888);
#11897=VERTEX_POINT('',#54890);
#11898=VERTEX_POINT('',#54892);
#11899=VERTEX_POINT('',#54894);
#11900=VERTEX_POINT('',#54896);
#11901=VERTEX_POINT('',#54898);
#11902=VERTEX_POINT('',#54900);
#11903=VERTEX_POINT('',#54902);
#11904=VERTEX_POINT('',#54904);
#11905=VERTEX_POINT('',#54906);
#11906=VERTEX_POINT('',#54908);
#11907=VERTEX_POINT('',#54910);
#11908=VERTEX_POINT('',#54912);
#11909=VERTEX_POINT('',#54914);
#11910=VERTEX_POINT('',#54916);
#11911=VERTEX_POINT('',#54918);
#11912=VERTEX_POINT('',#54920);
#11913=VERTEX_POINT('',#54922);
#11914=VERTEX_POINT('',#54924);
#11915=VERTEX_POINT('',#54926);
#11916=VERTEX_POINT('',#54928);
#11917=VERTEX_POINT('',#54930);
#11918=VERTEX_POINT('',#54932);
#11919=VERTEX_POINT('',#54934);
#11920=VERTEX_POINT('',#54938);
#11921=VERTEX_POINT('',#54942);
#11922=VERTEX_POINT('',#54949);
#11923=VERTEX_POINT('',#54951);
#11924=VERTEX_POINT('',#54955);
#11925=VERTEX_POINT('',#54956);
#11926=VERTEX_POINT('',#54961);
#11927=VERTEX_POINT('',#54965);
#11928=VERTEX_POINT('',#54969);
#11929=VERTEX_POINT('',#54973);
#11930=VERTEX_POINT('',#54974);
#11931=VERTEX_POINT('',#54977);
#11932=VERTEX_POINT('',#54982);
#11933=VERTEX_POINT('',#54986);
#11934=VERTEX_POINT('',#54990);
#11935=VERTEX_POINT('',#54994);
#11936=VERTEX_POINT('',#54998);
#11937=VERTEX_POINT('',#55002);
#11938=VERTEX_POINT('',#55006);
#11939=VERTEX_POINT('',#55010);
#11940=VERTEX_POINT('',#55014);
#11941=VERTEX_POINT('',#55018);
#11942=VERTEX_POINT('',#55022);
#11943=VERTEX_POINT('',#55026);
#11944=VERTEX_POINT('',#55030);
#11945=VERTEX_POINT('',#55034);
#11946=VERTEX_POINT('',#55038);
#11947=VERTEX_POINT('',#55042);
#11948=VERTEX_POINT('',#55046);
#11949=VERTEX_POINT('',#55050);
#11950=VERTEX_POINT('',#55054);
#11951=VERTEX_POINT('',#55058);
#11952=VERTEX_POINT('',#55062);
#11953=VERTEX_POINT('',#55066);
#11954=VERTEX_POINT('',#55070);
#11955=VERTEX_POINT('',#55074);
#11956=VERTEX_POINT('',#55078);
#11957=VERTEX_POINT('',#55082);
#11958=VERTEX_POINT('',#55086);
#11959=VERTEX_POINT('',#55090);
#11960=VERTEX_POINT('',#55094);
#11961=VERTEX_POINT('',#55098);
#11962=VERTEX_POINT('',#55102);
#11963=VERTEX_POINT('',#55106);
#11964=VERTEX_POINT('',#55110);
#11965=VERTEX_POINT('',#55114);
#11966=VERTEX_POINT('',#55118);
#11967=VERTEX_POINT('',#55122);
#11968=VERTEX_POINT('',#55126);
#11969=VERTEX_POINT('',#55130);
#11970=VERTEX_POINT('',#55137);
#11971=VERTEX_POINT('',#55138);
#11972=VERTEX_POINT('',#55140);
#11973=VERTEX_POINT('',#55142);
#11974=VERTEX_POINT('',#55146);
#11975=VERTEX_POINT('',#55147);
#11976=VERTEX_POINT('',#55149);
#11977=VERTEX_POINT('',#55151);
#11978=VERTEX_POINT('',#55155);
#11979=VERTEX_POINT('',#55159);
#11980=VERTEX_POINT('',#55165);
#11981=VERTEX_POINT('',#55167);
#11982=VERTEX_POINT('',#55171);
#11983=VERTEX_POINT('',#55173);
#11984=VERTEX_POINT('',#55175);
#11985=VERTEX_POINT('',#55179);
#11986=VERTEX_POINT('',#55181);
#11987=VERTEX_POINT('',#55185);
#11988=VERTEX_POINT('',#55186);
#11989=VERTEX_POINT('',#55188);
#11990=VERTEX_POINT('',#55190);
#11991=VERTEX_POINT('',#55194);
#11992=VERTEX_POINT('',#55197);
#11993=VERTEX_POINT('',#55201);
#11994=VERTEX_POINT('',#55205);
#11995=VERTEX_POINT('',#55206);
#11996=VERTEX_POINT('',#55208);
#11997=VERTEX_POINT('',#55210);
#11998=VERTEX_POINT('',#55212);
#11999=VERTEX_POINT('',#55214);
#12000=VERTEX_POINT('',#55216);
#12001=VERTEX_POINT('',#55218);
#12002=VERTEX_POINT('',#55220);
#12003=VERTEX_POINT('',#55222);
#12004=VERTEX_POINT('',#55224);
#12005=VERTEX_POINT('',#55226);
#12006=VERTEX_POINT('',#55228);
#12007=VERTEX_POINT('',#55230);
#12008=VERTEX_POINT('',#55232);
#12009=VERTEX_POINT('',#55234);
#12010=VERTEX_POINT('',#55236);
#12011=VERTEX_POINT('',#55238);
#12012=VERTEX_POINT('',#55240);
#12013=VERTEX_POINT('',#55242);
#12014=VERTEX_POINT('',#55244);
#12015=VERTEX_POINT('',#55246);
#12016=VERTEX_POINT('',#55248);
#12017=VERTEX_POINT('',#55250);
#12018=VERTEX_POINT('',#55252);
#12019=VERTEX_POINT('',#55254);
#12020=VERTEX_POINT('',#55256);
#12021=VERTEX_POINT('',#55258);
#12022=VERTEX_POINT('',#55260);
#12023=VERTEX_POINT('',#55262);
#12024=VERTEX_POINT('',#55264);
#12025=VERTEX_POINT('',#55266);
#12026=VERTEX_POINT('',#55268);
#12027=VERTEX_POINT('',#55270);
#12028=VERTEX_POINT('',#55272);
#12029=VERTEX_POINT('',#55274);
#12030=VERTEX_POINT('',#55276);
#12031=VERTEX_POINT('',#55278);
#12032=VERTEX_POINT('',#55280);
#12033=VERTEX_POINT('',#55282);
#12034=VERTEX_POINT('',#55284);
#12035=VERTEX_POINT('',#55286);
#12036=VERTEX_POINT('',#55288);
#12037=VERTEX_POINT('',#55290);
#12038=VERTEX_POINT('',#55294);
#12039=VERTEX_POINT('',#55298);
#12040=VERTEX_POINT('',#55302);
#12041=VERTEX_POINT('',#55303);
#12042=VERTEX_POINT('',#55308);
#12043=VERTEX_POINT('',#55310);
#12044=VERTEX_POINT('',#55314);
#12045=VERTEX_POINT('',#55316);
#12046=VERTEX_POINT('',#55320);
#12047=VERTEX_POINT('',#55322);
#12048=VERTEX_POINT('',#55330);
#12049=VERTEX_POINT('',#55332);
#12050=VERTEX_POINT('',#55334);
#12051=VERTEX_POINT('',#55338);
#12052=VERTEX_POINT('',#55339);
#12053=VERTEX_POINT('',#55344);
#12054=VERTEX_POINT('',#55346);
#12055=VERTEX_POINT('',#55350);
#12056=VERTEX_POINT('',#55351);
#12057=VERTEX_POINT('',#55356);
#12058=VERTEX_POINT('',#55361);
#12059=VERTEX_POINT('',#55363);
#12060=VERTEX_POINT('',#55370);
#12061=VERTEX_POINT('',#55371);
#12062=VERTEX_POINT('',#55376);
#12063=VERTEX_POINT('',#55380);
#12064=VERTEX_POINT('',#55384);
#12065=VERTEX_POINT('',#55388);
#12066=VERTEX_POINT('',#55392);
#12067=VERTEX_POINT('',#55396);
#12068=VERTEX_POINT('',#55400);
#12069=VERTEX_POINT('',#55404);
#12070=VERTEX_POINT('',#55408);
#12071=VERTEX_POINT('',#55412);
#12072=VERTEX_POINT('',#55416);
#12073=VERTEX_POINT('',#55420);
#12074=VERTEX_POINT('',#55424);
#12075=VERTEX_POINT('',#55428);
#12076=VERTEX_POINT('',#55432);
#12077=VERTEX_POINT('',#55436);
#12078=VERTEX_POINT('',#55440);
#12079=VERTEX_POINT('',#55444);
#12080=VERTEX_POINT('',#55448);
#12081=VERTEX_POINT('',#55452);
#12082=VERTEX_POINT('',#55456);
#12083=VERTEX_POINT('',#55460);
#12084=VERTEX_POINT('',#55464);
#12085=VERTEX_POINT('',#55468);
#12086=VERTEX_POINT('',#55472);
#12087=VERTEX_POINT('',#55476);
#12088=VERTEX_POINT('',#55480);
#12089=VERTEX_POINT('',#55484);
#12090=VERTEX_POINT('',#55488);
#12091=VERTEX_POINT('',#55492);
#12092=VERTEX_POINT('',#55496);
#12093=VERTEX_POINT('',#55500);
#12094=VERTEX_POINT('',#55504);
#12095=VERTEX_POINT('',#55508);
#12096=VERTEX_POINT('',#55512);
#12097=VERTEX_POINT('',#55516);
#12098=VERTEX_POINT('',#55520);
#12099=VERTEX_POINT('',#55524);
#12100=VERTEX_POINT('',#55528);
#12101=VERTEX_POINT('',#55532);
#12102=VERTEX_POINT('',#55536);
#12103=VERTEX_POINT('',#55540);
#12104=VERTEX_POINT('',#55546);
#12105=VERTEX_POINT('',#55547);
#12106=VERTEX_POINT('',#55549);
#12107=VERTEX_POINT('',#55551);
#12108=VERTEX_POINT('',#55555);
#12109=VERTEX_POINT('',#55557);
#12110=VERTEX_POINT('',#55561);
#12111=VERTEX_POINT('',#55563);
#12112=VERTEX_POINT('',#55567);
#12113=VERTEX_POINT('',#55569);
#12114=VERTEX_POINT('',#55573);
#12115=VERTEX_POINT('',#55575);
#12116=VERTEX_POINT('',#55579);
#12117=VERTEX_POINT('',#55580);
#12118=VERTEX_POINT('',#55582);
#12119=VERTEX_POINT('',#55584);
#12120=VERTEX_POINT('',#55588);
#12121=VERTEX_POINT('',#55590);
#12122=VERTEX_POINT('',#55594);
#12123=VERTEX_POINT('',#55596);
#12124=VERTEX_POINT('',#55603);
#12125=VERTEX_POINT('',#55605);
#12126=VERTEX_POINT('',#55607);
#12127=VERTEX_POINT('',#55611);
#12128=VERTEX_POINT('',#55613);
#12129=VERTEX_POINT('',#55617);
#12130=VERTEX_POINT('',#55618);
#12131=VERTEX_POINT('',#55623);
#12132=VERTEX_POINT('',#55624);
#12133=VERTEX_POINT('',#55629);
#12134=VERTEX_POINT('',#55630);
#12135=VERTEX_POINT('',#55635);
#12136=VERTEX_POINT('',#55636);
#12137=VERTEX_POINT('',#55641);
#12138=VERTEX_POINT('',#55643);
#12139=VERTEX_POINT('',#55647);
#12140=VERTEX_POINT('',#55648);
#12141=VERTEX_POINT('',#55653);
#12142=VERTEX_POINT('',#55654);
#12143=VERTEX_POINT('',#55659);
#12144=VERTEX_POINT('',#55660);
#12145=VERTEX_POINT('',#55665);
#12146=VERTEX_POINT('',#55667);
#12147=VERTEX_POINT('',#55671);
#12148=VERTEX_POINT('',#55673);
#12149=VERTEX_POINT('',#55677);
#12150=VERTEX_POINT('',#55679);
#12151=VERTEX_POINT('',#55683);
#12152=VERTEX_POINT('',#55685);
#12153=VERTEX_POINT('',#55689);
#12154=VERTEX_POINT('',#55694);
#12155=VERTEX_POINT('',#55696);
#12156=VERTEX_POINT('',#55700);
#12157=VERTEX_POINT('',#55701);
#12158=VERTEX_POINT('',#55706);
#12159=VERTEX_POINT('',#55708);
#12160=VERTEX_POINT('',#55712);
#12161=VERTEX_POINT('',#55714);
#12162=VERTEX_POINT('',#55718);
#12163=VERTEX_POINT('',#55719);
#12164=VERTEX_POINT('',#55728);
#12165=VERTEX_POINT('',#55732);
#12166=VERTEX_POINT('',#55734);
#12167=VERTEX_POINT('',#55738);
#12168=VERTEX_POINT('',#55740);
#12169=VERTEX_POINT('',#55745);
#12170=VERTEX_POINT('',#55752);
#12171=VERTEX_POINT('',#55754);
#12172=VERTEX_POINT('',#55756);
#12173=VERTEX_POINT('',#55758);
#12174=VERTEX_POINT('',#55760);
#12175=VERTEX_POINT('',#55762);
#12176=VERTEX_POINT('',#55764);
#12177=VERTEX_POINT('',#55766);
#12178=VERTEX_POINT('',#55768);
#12179=VERTEX_POINT('',#55770);
#12180=VERTEX_POINT('',#55772);
#12181=VERTEX_POINT('',#55774);
#12182=VERTEX_POINT('',#55776);
#12183=VERTEX_POINT('',#55778);
#12184=VERTEX_POINT('',#55780);
#12185=VERTEX_POINT('',#55782);
#12186=VERTEX_POINT('',#55784);
#12187=VERTEX_POINT('',#55786);
#12188=VERTEX_POINT('',#55788);
#12189=VERTEX_POINT('',#55790);
#12190=VERTEX_POINT('',#55792);
#12191=VERTEX_POINT('',#55794);
#12192=VERTEX_POINT('',#55796);
#12193=VERTEX_POINT('',#55798);
#12194=VERTEX_POINT('',#55800);
#12195=VERTEX_POINT('',#55802);
#12196=VERTEX_POINT('',#55804);
#12197=VERTEX_POINT('',#55806);
#12198=VERTEX_POINT('',#55808);
#12199=VERTEX_POINT('',#55810);
#12200=VERTEX_POINT('',#55812);
#12201=VERTEX_POINT('',#55814);
#12202=VERTEX_POINT('',#55816);
#12203=VERTEX_POINT('',#55818);
#12204=VERTEX_POINT('',#55820);
#12205=VERTEX_POINT('',#55822);
#12206=VERTEX_POINT('',#55826);
#12207=VERTEX_POINT('',#55828);
#12208=VERTEX_POINT('',#55830);
#12209=VERTEX_POINT('',#55832);
#12210=VERTEX_POINT('',#55834);
#12211=VERTEX_POINT('',#55836);
#12212=VERTEX_POINT('',#55838);
#12213=VERTEX_POINT('',#55840);
#12214=VERTEX_POINT('',#55842);
#12215=VERTEX_POINT('',#55844);
#12216=VERTEX_POINT('',#55846);
#12217=VERTEX_POINT('',#55848);
#12218=VERTEX_POINT('',#55852);
#12219=VERTEX_POINT('',#55853);
#12220=VERTEX_POINT('',#55858);
#12221=VERTEX_POINT('',#55859);
#12222=VERTEX_POINT('',#55864);
#12223=VERTEX_POINT('',#55868);
#12224=VERTEX_POINT('',#55872);
#12225=VERTEX_POINT('',#55876);
#12226=VERTEX_POINT('',#55878);
#12227=VERTEX_POINT('',#55882);
#12228=VERTEX_POINT('',#55884);
#12229=VERTEX_POINT('',#55890);
#12230=VERTEX_POINT('',#55896);
#12231=VERTEX_POINT('',#55897);
#12232=VERTEX_POINT('',#55902);
#12233=VERTEX_POINT('',#55903);
#12234=VERTEX_POINT('',#55910);
#12235=VERTEX_POINT('',#55911);
#12236=VERTEX_POINT('',#55916);
#12237=VERTEX_POINT('',#55917);
#12238=VERTEX_POINT('',#55926);
#12239=VERTEX_POINT('',#55927);
#12240=VERTEX_POINT('',#55932);
#12241=VERTEX_POINT('',#55933);
#12242=VERTEX_POINT('',#55940);
#12243=VERTEX_POINT('',#55942);
#12244=VERTEX_POINT('',#55948);
#12245=VERTEX_POINT('',#55949);
#12246=VERTEX_POINT('',#55954);
#12247=VERTEX_POINT('',#55955);
#12248=VERTEX_POINT('',#55962);
#12249=VERTEX_POINT('',#55963);
#12250=VERTEX_POINT('',#55968);
#12251=VERTEX_POINT('',#55969);
#12252=VERTEX_POINT('',#55980);
#12253=VERTEX_POINT('',#55981);
#12254=VERTEX_POINT('',#55986);
#12255=VERTEX_POINT('',#55987);
#12256=VERTEX_POINT('',#55994);
#12257=VERTEX_POINT('',#55996);
#12258=VERTEX_POINT('',#56000);
#12259=VERTEX_POINT('',#56002);
#12260=VERTEX_POINT('',#56006);
#12261=VERTEX_POINT('',#56007);
#12262=VERTEX_POINT('',#56012);
#12263=VERTEX_POINT('',#56016);
#12264=VERTEX_POINT('',#56022);
#12265=VERTEX_POINT('',#56038);
#12266=VERTEX_POINT('',#56045);
#12267=VERTEX_POINT('',#56049);
#12268=VERTEX_POINT('',#56061);
#12269=VERTEX_POINT('',#56063);
#12270=VERTEX_POINT('',#56093);
#12271=VERTEX_POINT('',#56097);
#12272=VERTEX_POINT('',#56101);
#12273=VERTEX_POINT('',#56104);
#12274=VERTEX_POINT('',#56105);
#12275=VERTEX_POINT('',#56107);
#12276=VERTEX_POINT('',#56115);
#12277=VERTEX_POINT('',#56116);
#12278=VERTEX_POINT('',#56118);
#12279=VERTEX_POINT('',#56126);
#12280=VERTEX_POINT('',#56127);
#12281=VERTEX_POINT('',#56129);
#12282=VERTEX_POINT('',#56140);
#12283=VERTEX_POINT('',#56154);
#12284=VERTEX_POINT('',#56156);
#12285=VERTEX_POINT('',#56159);
#12286=VERTEX_POINT('',#56161);
#12287=VERTEX_POINT('',#56163);
#12288=VERTEX_POINT('',#56165);
#12289=VERTEX_POINT('',#56167);
#12290=VERTEX_POINT('',#56169);
#12291=VERTEX_POINT('',#56173);
#12292=VERTEX_POINT('',#56176);
#12293=VERTEX_POINT('',#56178);
#12294=VERTEX_POINT('',#56180);
#12295=VERTEX_POINT('',#56182);
#12296=VERTEX_POINT('',#56186);
#12297=VERTEX_POINT('',#56188);
#12298=VERTEX_POINT('',#56190);
#12299=VERTEX_POINT('',#56192);
#12300=VERTEX_POINT('',#56196);
#12301=VERTEX_POINT('',#56200);
#12302=VERTEX_POINT('',#56204);
#12303=VERTEX_POINT('',#56208);
#12304=VERTEX_POINT('',#56212);
#12305=VERTEX_POINT('',#56216);
#12306=VERTEX_POINT('',#56220);
#12307=VERTEX_POINT('',#56221);
#12308=VERTEX_POINT('',#56226);
#12309=VERTEX_POINT('',#56230);
#12310=VERTEX_POINT('',#56234);
#12311=VERTEX_POINT('',#56238);
#12312=VERTEX_POINT('',#56245);
#12313=VERTEX_POINT('',#56253);
#12314=VERTEX_POINT('',#56261);
#12315=VERTEX_POINT('',#56269);
#12316=VERTEX_POINT('',#56277);
#12317=VERTEX_POINT('',#56285);
#12318=VERTEX_POINT('',#56293);
#12319=VERTEX_POINT('',#56301);
#12320=VERTEX_POINT('',#56309);
#12321=VERTEX_POINT('',#56317);
#12322=VERTEX_POINT('',#56349);
#12323=VERTEX_POINT('',#56351);
#12324=VERTEX_POINT('',#56355);
#12325=VERTEX_POINT('',#56358);
#12326=VERTEX_POINT('',#56360);
#12327=VERTEX_POINT('',#56364);
#12328=VERTEX_POINT('',#56367);
#12329=VERTEX_POINT('',#56369);
#12330=VERTEX_POINT('',#56373);
#12331=VERTEX_POINT('',#56376);
#12332=VERTEX_POINT('',#56378);
#12333=VERTEX_POINT('',#56382);
#12334=VERTEX_POINT('',#56385);
#12335=VERTEX_POINT('',#56387);
#12336=VERTEX_POINT('',#56391);
#12337=VERTEX_POINT('',#56394);
#12338=VERTEX_POINT('',#56396);
#12339=VERTEX_POINT('',#56400);
#12340=VERTEX_POINT('',#56403);
#12341=VERTEX_POINT('',#56405);
#12342=VERTEX_POINT('',#56409);
#12343=VERTEX_POINT('',#56412);
#12344=VERTEX_POINT('',#56414);
#12345=VERTEX_POINT('',#56418);
#12346=VERTEX_POINT('',#56421);
#12347=VERTEX_POINT('',#56422);
#12348=VERTEX_POINT('',#56424);
#12349=VERTEX_POINT('',#56426);
#12350=VERTEX_POINT('',#56430);
#12351=VERTEX_POINT('',#56432);
#12352=VERTEX_POINT('',#56434);
#12353=VERTEX_POINT('',#56436);
#12354=VERTEX_POINT('',#56438);
#12355=VERTEX_POINT('',#56440);
#12356=VERTEX_POINT('',#56442);
#12357=VERTEX_POINT('',#56444);
#12358=VERTEX_POINT('',#56448);
#12359=VERTEX_POINT('',#56450);
#12360=VERTEX_POINT('',#56454);
#12361=VERTEX_POINT('',#56455);
#12362=VERTEX_POINT('',#56457);
#12363=VERTEX_POINT('',#56459);
#12364=VERTEX_POINT('',#56461);
#12365=VERTEX_POINT('',#56465);
#12366=VERTEX_POINT('',#56484);
#12367=VERTEX_POINT('',#56485);
#12368=VERTEX_POINT('',#56488);
#12369=VERTEX_POINT('',#56492);
#12370=VERTEX_POINT('',#56493);
#12371=VERTEX_POINT('',#56495);
#12372=VERTEX_POINT('',#56497);
#12373=VERTEX_POINT('',#56499);
#12374=VERTEX_POINT('',#56501);
#12375=VERTEX_POINT('',#56503);
#12376=VERTEX_POINT('',#56505);
#12377=VERTEX_POINT('',#56509);
#12378=VERTEX_POINT('',#56513);
#12379=VERTEX_POINT('',#56515);
#12380=VERTEX_POINT('',#56519);
#12381=VERTEX_POINT('',#56521);
#12382=VERTEX_POINT('',#56525);
#12383=VERTEX_POINT('',#56526);
#12384=VERTEX_POINT('',#56528);
#12385=VERTEX_POINT('',#56530);
#12386=VERTEX_POINT('',#56532);
#12387=VERTEX_POINT('',#56534);
#12388=VERTEX_POINT('',#56541);
#12389=VERTEX_POINT('',#56544);
#12390=VERTEX_POINT('',#56548);
#12391=VERTEX_POINT('',#56553);
#12392=VERTEX_POINT('',#56558);
#12393=VERTEX_POINT('',#56563);
#12394=VERTEX_POINT('',#56577);
#12395=VERTEX_POINT('',#56579);
#12396=VERTEX_POINT('',#56583);
#12397=VERTEX_POINT('',#56585);
#12398=VERTEX_POINT('',#56591);
#12399=VERTEX_POINT('',#56592);
#12400=VERTEX_POINT('',#56594);
#12401=VERTEX_POINT('',#56596);
#12402=VERTEX_POINT('',#56600);
#12403=VERTEX_POINT('',#56601);
#12404=VERTEX_POINT('',#56603);
#12405=VERTEX_POINT('',#56605);
#12406=VERTEX_POINT('',#56618);
#12407=VERTEX_POINT('',#56620);
#12408=VERTEX_POINT('',#56624);
#12409=VERTEX_POINT('',#56628);
#12410=VERTEX_POINT('',#56629);
#12411=VERTEX_POINT('',#56631);
#12412=VERTEX_POINT('',#56636);
#12413=VERTEX_POINT('',#56641);
#12414=VERTEX_POINT('',#56642);
#12415=VERTEX_POINT('',#56644);
#12416=VERTEX_POINT('',#56646);
#12417=VERTEX_POINT('',#56648);
#12418=VERTEX_POINT('',#56650);
#12419=VERTEX_POINT('',#56655);
#12420=VERTEX_POINT('',#56657);
#12421=VERTEX_POINT('',#56661);
#12422=VERTEX_POINT('',#56665);
#12423=VERTEX_POINT('',#56669);
#12424=VERTEX_POINT('',#56673);
#12425=VERTEX_POINT('',#56681);
#12426=VERTEX_POINT('',#56682);
#12427=VERTEX_POINT('',#56685);
#12428=VERTEX_POINT('',#56689);
#12429=VERTEX_POINT('',#56690);
#12430=VERTEX_POINT('',#56692);
#12431=VERTEX_POINT('',#56694);
#12432=VERTEX_POINT('',#56696);
#12433=VERTEX_POINT('',#56698);
#12434=VERTEX_POINT('',#56700);
#12435=VERTEX_POINT('',#56702);
#12436=VERTEX_POINT('',#56706);
#12437=VERTEX_POINT('',#56710);
#12438=VERTEX_POINT('',#56712);
#12439=VERTEX_POINT('',#56716);
#12440=VERTEX_POINT('',#56718);
#12441=VERTEX_POINT('',#56722);
#12442=VERTEX_POINT('',#56723);
#12443=VERTEX_POINT('',#56725);
#12444=VERTEX_POINT('',#56727);
#12445=VERTEX_POINT('',#56729);
#12446=VERTEX_POINT('',#56731);
#12447=VERTEX_POINT('',#56738);
#12448=VERTEX_POINT('',#56741);
#12449=VERTEX_POINT('',#56745);
#12450=VERTEX_POINT('',#56750);
#12451=VERTEX_POINT('',#56755);
#12452=VERTEX_POINT('',#56760);
#12453=VERTEX_POINT('',#56774);
#12454=VERTEX_POINT('',#56776);
#12455=VERTEX_POINT('',#56780);
#12456=VERTEX_POINT('',#56782);
#12457=VERTEX_POINT('',#56788);
#12458=VERTEX_POINT('',#56789);
#12459=VERTEX_POINT('',#56791);
#12460=VERTEX_POINT('',#56793);
#12461=VERTEX_POINT('',#56797);
#12462=VERTEX_POINT('',#56798);
#12463=VERTEX_POINT('',#56800);
#12464=VERTEX_POINT('',#56802);
#12465=VERTEX_POINT('',#56815);
#12466=VERTEX_POINT('',#56817);
#12467=VERTEX_POINT('',#56821);
#12468=VERTEX_POINT('',#56825);
#12469=VERTEX_POINT('',#56826);
#12470=VERTEX_POINT('',#56828);
#12471=VERTEX_POINT('',#56833);
#12472=VERTEX_POINT('',#56838);
#12473=VERTEX_POINT('',#56839);
#12474=VERTEX_POINT('',#56841);
#12475=VERTEX_POINT('',#56843);
#12476=VERTEX_POINT('',#56845);
#12477=VERTEX_POINT('',#56847);
#12478=VERTEX_POINT('',#56852);
#12479=VERTEX_POINT('',#56854);
#12480=VERTEX_POINT('',#56858);
#12481=VERTEX_POINT('',#56862);
#12482=VERTEX_POINT('',#56866);
#12483=VERTEX_POINT('',#56870);
#12484=VERTEX_POINT('',#56878);
#12485=VERTEX_POINT('',#56880);
#12486=VERTEX_POINT('',#56884);
#12487=VERTEX_POINT('',#56888);
#12488=VERTEX_POINT('',#56889);
#12489=VERTEX_POINT('',#56891);
#12490=VERTEX_POINT('',#56896);
#12491=VERTEX_POINT('',#56901);
#12492=VERTEX_POINT('',#56902);
#12493=VERTEX_POINT('',#56904);
#12494=VERTEX_POINT('',#56906);
#12495=VERTEX_POINT('',#56908);
#12496=VERTEX_POINT('',#56910);
#12497=VERTEX_POINT('',#56915);
#12498=VERTEX_POINT('',#56917);
#12499=VERTEX_POINT('',#56921);
#12500=VERTEX_POINT('',#56925);
#12501=VERTEX_POINT('',#56929);
#12502=VERTEX_POINT('',#56933);
#12503=EDGE_CURVE('',#10279,#10279,#9185,.T.);
#12504=EDGE_CURVE('',#10279,#10280,#5251,.T.);
#12505=EDGE_CURVE('',#10280,#10280,#9186,.T.);
#12506=EDGE_CURVE('',#10281,#10281,#9187,.T.);
#12507=EDGE_CURVE('',#10281,#10282,#5252,.T.);
#12508=EDGE_CURVE('',#10282,#10282,#9188,.T.);
#12509=EDGE_CURVE('',#10283,#10283,#9189,.T.);
#12510=EDGE_CURVE('',#10283,#10284,#5253,.T.);
#12511=EDGE_CURVE('',#10284,#10284,#9190,.T.);
#12512=EDGE_CURVE('',#10285,#10285,#9191,.T.);
#12513=EDGE_CURVE('',#10285,#10286,#5254,.T.);
#12514=EDGE_CURVE('',#10286,#10286,#9192,.T.);
#12515=EDGE_CURVE('',#10287,#10287,#9193,.T.);
#12516=EDGE_CURVE('',#10287,#10288,#5255,.T.);
#12517=EDGE_CURVE('',#10288,#10288,#9194,.T.);
#12518=EDGE_CURVE('',#10289,#10289,#9195,.T.);
#12519=EDGE_CURVE('',#10289,#10290,#5256,.T.);
#12520=EDGE_CURVE('',#10290,#10290,#9196,.T.);
#12521=EDGE_CURVE('',#10291,#10291,#9197,.T.);
#12522=EDGE_CURVE('',#10291,#10292,#5257,.T.);
#12523=EDGE_CURVE('',#10292,#10292,#9198,.T.);
#12524=EDGE_CURVE('',#10293,#10293,#9199,.T.);
#12525=EDGE_CURVE('',#10293,#10294,#5258,.T.);
#12526=EDGE_CURVE('',#10294,#10294,#9200,.T.);
#12527=EDGE_CURVE('',#10295,#10295,#9201,.T.);
#12528=EDGE_CURVE('',#10295,#10296,#5259,.T.);
#12529=EDGE_CURVE('',#10296,#10296,#9202,.T.);
#12530=EDGE_CURVE('',#10297,#10295,#5260,.T.);
#12531=EDGE_CURVE('',#10298,#10298,#9203,.T.);
#12532=EDGE_CURVE('',#10298,#10299,#5261,.T.);
#12533=EDGE_CURVE('',#10299,#10299,#9204,.T.);
#12534=EDGE_CURVE('',#10300,#10298,#5262,.T.);
#12535=EDGE_CURVE('',#10301,#10301,#9205,.T.);
#12536=EDGE_CURVE('',#10301,#10302,#5263,.T.);
#12537=EDGE_CURVE('',#10302,#10302,#9206,.T.);
#12538=EDGE_CURVE('',#10303,#10301,#5264,.T.);
#12539=EDGE_CURVE('',#10304,#10304,#9207,.T.);
#12540=EDGE_CURVE('',#10304,#10305,#5265,.T.);
#12541=EDGE_CURVE('',#10305,#10305,#9208,.T.);
#12542=EDGE_CURVE('',#10306,#10304,#5266,.T.);
#12543=EDGE_CURVE('',#10307,#10308,#5267,.T.);
#12544=EDGE_CURVE('',#10308,#10309,#5268,.T.);
#12545=EDGE_CURVE('',#10310,#10309,#5269,.T.);
#12546=EDGE_CURVE('',#10310,#10307,#5270,.T.);
#12547=EDGE_CURVE('',#10311,#10312,#5271,.T.);
#12548=EDGE_CURVE('',#10313,#10312,#5272,.T.);
#12549=EDGE_CURVE('',#10314,#10313,#5273,.T.);
#12550=EDGE_CURVE('',#10314,#10311,#5274,.T.);
#12551=EDGE_CURVE('',#10312,#10315,#5275,.T.);
#12552=EDGE_CURVE('',#10316,#10315,#5276,.T.);
#12553=EDGE_CURVE('',#10313,#10316,#5277,.T.);
#12554=EDGE_CURVE('',#10315,#10307,#5278,.T.);
#12555=EDGE_CURVE('',#10316,#10310,#5279,.T.);
#12556=EDGE_CURVE('',#10317,#10314,#5280,.T.);
#12557=EDGE_CURVE('',#10318,#10317,#5281,.T.);
#12558=EDGE_CURVE('',#10318,#10311,#5282,.T.);
#12559=EDGE_CURVE('',#10319,#10309,#5283,.T.);
#12560=EDGE_CURVE('',#10320,#10319,#5284,.T.);
#12561=EDGE_CURVE('',#10317,#10320,#5285,.T.);
#12562=EDGE_CURVE('',#10321,#10308,#5286,.T.);
#12563=EDGE_CURVE('',#10318,#10322,#5287,.T.);
#12564=EDGE_CURVE('',#10322,#10321,#5288,.T.);
#12565=EDGE_CURVE('',#10321,#10319,#5289,.T.);
#12566=EDGE_CURVE('',#10322,#10320,#5290,.T.);
#12567=EDGE_CURVE('',#10323,#10323,#9209,.T.);
#12568=EDGE_CURVE('',#10323,#10324,#5291,.T.);
#12569=EDGE_CURVE('',#10324,#10325,#9210,.T.);
#12570=EDGE_CURVE('',#10325,#10326,#5292,.T.);
#12571=EDGE_CURVE('',#10326,#10327,#649,.F.);
#12572=EDGE_CURVE('',#10327,#10328,#5293,.T.);
#12573=EDGE_CURVE('',#10328,#10324,#9211,.T.);
#12574=EDGE_CURVE('',#10329,#10329,#9212,.T.);
#12575=EDGE_CURVE('',#10329,#10323,#9213,.T.);
#12576=EDGE_CURVE('',#10330,#10330,#9214,.T.);
#12577=EDGE_CURVE('',#10330,#10331,#5294,.T.);
#12578=EDGE_CURVE('',#10331,#10331,#9215,.T.);
#12579=EDGE_CURVE('',#10332,#10332,#9216,.T.);
#12580=EDGE_CURVE('',#10332,#10330,#5295,.T.);
#12581=EDGE_CURVE('',#10333,#10333,#9217,.T.);
#12582=EDGE_CURVE('',#10333,#10332,#9218,.T.);
#12583=EDGE_CURVE('',#10334,#10334,#9219,.T.);
#12584=EDGE_CURVE('',#10334,#10335,#5296,.T.);
#12585=EDGE_CURVE('',#10335,#10335,#9220,.T.);
#12586=EDGE_CURVE('',#10336,#10337,#9221,.T.);
#12587=EDGE_CURVE('',#10337,#10336,#9222,.T.);
#12588=EDGE_CURVE('',#10337,#10334,#5297,.T.);
#12589=EDGE_CURVE('',#10336,#10338,#5298,.T.);
#12590=EDGE_CURVE('',#10338,#10338,#9223,.T.);
#12591=EDGE_CURVE('',#10339,#10339,#9224,.T.);
#12592=EDGE_CURVE('',#10339,#10340,#9225,.T.);
#12593=EDGE_CURVE('',#10340,#10340,#9226,.T.);
#12594=EDGE_CURVE('',#10341,#10341,#9227,.T.);
#12595=EDGE_CURVE('',#10341,#10339,#5299,.T.);
#12596=EDGE_CURVE('',#10342,#10342,#9228,.T.);
#12597=EDGE_CURVE('',#10342,#10343,#5300,.T.);
#12598=EDGE_CURVE('',#10343,#10343,#9229,.T.);
#12599=EDGE_CURVE('',#10344,#10345,#9230,.T.);
#12600=EDGE_CURVE('',#10345,#10344,#9231,.T.);
#12601=EDGE_CURVE('',#10345,#10346,#5301,.T.);
#12602=EDGE_CURVE('',#10346,#10346,#9232,.T.);
#12603=EDGE_CURVE('',#10344,#10347,#5302,.T.);
#12604=EDGE_CURVE('',#10347,#10347,#9233,.T.);
#12605=EDGE_CURVE('',#10328,#10348,#650,.T.);
#12606=EDGE_CURVE('',#10348,#10349,#9234,.T.);
#12607=EDGE_CURVE('',#10349,#10325,#651,.T.);
#12608=EDGE_CURVE('',#10350,#10348,#5303,.T.);
#12609=EDGE_CURVE('',#10351,#10350,#5304,.T.);
#12610=EDGE_CURVE('',#10351,#10349,#5305,.T.);
#12611=EDGE_CURVE('',#10327,#10352,#5306,.T.);
#12612=EDGE_CURVE('',#10352,#10350,#5307,.T.);
#12613=EDGE_CURVE('',#10353,#10351,#5308,.T.);
#12614=EDGE_CURVE('',#10353,#10326,#5309,.T.);
#12615=EDGE_CURVE('',#10352,#10353,#9235,.T.);
#12616=EDGE_CURVE('',#10354,#10354,#652,.T.);
#12617=EDGE_CURVE('',#10354,#10355,#5310,.T.);
#12618=EDGE_CURVE('',#10355,#10355,#653,.T.);
#12619=EDGE_CURVE('',#10356,#10356,#9236,.T.);
#12620=EDGE_CURVE('',#10356,#10357,#5311,.T.);
#12621=EDGE_CURVE('',#10357,#10357,#9237,.T.);
#12622=EDGE_CURVE('',#10358,#10358,#9238,.T.);
#12623=EDGE_CURVE('',#10358,#10359,#5312,.T.);
#12624=EDGE_CURVE('',#10359,#10359,#9239,.T.);
#12625=EDGE_CURVE('',#10360,#10360,#9240,.T.);
#12626=EDGE_CURVE('',#10360,#10361,#5313,.T.);
#12627=EDGE_CURVE('',#10361,#10361,#9241,.T.);
#12628=EDGE_CURVE('',#10362,#10362,#9242,.T.);
#12629=EDGE_CURVE('',#10362,#10363,#5314,.T.);
#12630=EDGE_CURVE('',#10363,#10363,#9243,.T.);
#12631=EDGE_CURVE('',#10364,#10364,#9244,.T.);
#12632=EDGE_CURVE('',#10364,#10365,#5315,.T.);
#12633=EDGE_CURVE('',#10365,#10365,#9245,.T.);
#12634=EDGE_CURVE('',#10366,#10366,#9246,.T.);
#12635=EDGE_CURVE('',#10366,#10367,#5316,.T.);
#12636=EDGE_CURVE('',#10367,#10367,#9247,.T.);
#12637=EDGE_CURVE('',#10368,#10368,#9248,.T.);
#12638=EDGE_CURVE('',#10368,#10369,#5317,.T.);
#12639=EDGE_CURVE('',#10369,#10369,#9249,.T.);
#12640=EDGE_CURVE('',#10370,#10370,#9250,.T.);
#12641=EDGE_CURVE('',#10370,#10371,#5318,.T.);
#12642=EDGE_CURVE('',#10371,#10371,#9251,.T.);
#12643=EDGE_CURVE('',#10372,#10372,#9252,.T.);
#12644=EDGE_CURVE('',#10372,#10373,#5319,.T.);
#12645=EDGE_CURVE('',#10373,#10373,#9253,.T.);
#12646=EDGE_CURVE('',#10374,#10374,#9254,.T.);
#12647=EDGE_CURVE('',#10374,#10375,#5320,.T.);
#12648=EDGE_CURVE('',#10375,#10375,#9255,.T.);
#12649=EDGE_CURVE('',#10376,#10376,#9256,.T.);
#12650=EDGE_CURVE('',#10376,#10377,#5321,.T.);
#12651=EDGE_CURVE('',#10377,#10377,#9257,.T.);
#12652=EDGE_CURVE('',#10378,#10378,#9258,.T.);
#12653=EDGE_CURVE('',#10378,#10379,#5322,.T.);
#12654=EDGE_CURVE('',#10379,#10379,#9259,.T.);
#12655=EDGE_CURVE('',#10380,#10380,#9260,.T.);
#12656=EDGE_CURVE('',#10380,#10368,#9261,.T.);
#12657=EDGE_CURVE('',#10381,#10382,#5323,.T.);
#12658=EDGE_CURVE('',#10383,#10382,#9262,.T.);
#12659=EDGE_CURVE('',#10383,#10384,#5324,.T.);
#12660=EDGE_CURVE('',#10381,#10384,#9263,.T.);
#12661=EDGE_CURVE('',#10385,#10382,#654,.T.);
#12662=EDGE_CURVE('',#10386,#10385,#9264,.T.);
#12663=EDGE_CURVE('',#10383,#10386,#655,.T.);
#12664=EDGE_CURVE('',#10381,#10387,#656,.T.);
#12665=EDGE_CURVE('',#10388,#10384,#657,.T.);
#12666=EDGE_CURVE('',#10387,#10388,#9265,.T.);
#12667=EDGE_CURVE('',#10389,#10388,#5325,.T.);
#12668=EDGE_CURVE('',#10390,#10389,#9266,.T.);
#12669=EDGE_CURVE('',#10387,#10390,#5326,.T.);
#12670=EDGE_CURVE('',#10386,#10391,#5327,.T.);
#12671=EDGE_CURVE('',#10392,#10385,#5328,.T.);
#12672=EDGE_CURVE('',#10391,#10392,#9267,.T.);
#12673=EDGE_CURVE('',#10393,#10392,#658,.T.);
#12674=EDGE_CURVE('',#10394,#10393,#9268,.T.);
#12675=EDGE_CURVE('',#10391,#10394,#659,.T.);
#12676=EDGE_CURVE('',#10390,#10395,#660,.T.);
#12677=EDGE_CURVE('',#10396,#10389,#661,.T.);
#12678=EDGE_CURVE('',#10395,#10396,#9269,.T.);
#12679=EDGE_CURVE('',#10395,#10393,#5329,.T.);
#12680=EDGE_CURVE('',#10394,#10396,#5330,.T.);
#12681=EDGE_CURVE('',#10397,#10397,#9270,.T.);
#12682=EDGE_CURVE('',#10397,#10398,#5331,.T.);
#12683=EDGE_CURVE('',#10398,#10398,#9271,.T.);
#12684=EDGE_CURVE('',#10399,#10399,#9272,.T.);
#12685=EDGE_CURVE('',#10399,#10400,#5332,.T.);
#12686=EDGE_CURVE('',#10400,#10400,#9273,.T.);
#12687=EDGE_CURVE('',#10401,#10401,#9274,.T.);
#12688=EDGE_CURVE('',#10401,#10402,#5333,.T.);
#12689=EDGE_CURVE('',#10402,#10402,#9275,.T.);
#12690=EDGE_CURVE('',#10403,#10403,#9276,.T.);
#12691=EDGE_CURVE('',#10403,#10404,#5334,.T.);
#12692=EDGE_CURVE('',#10404,#10404,#9277,.T.);
#12693=EDGE_CURVE('',#10405,#10405,#9278,.T.);
#12694=EDGE_CURVE('',#10405,#10406,#5335,.T.);
#12695=EDGE_CURVE('',#10406,#10406,#9279,.T.);
#12696=EDGE_CURVE('',#10407,#10407,#9280,.T.);
#12697=EDGE_CURVE('',#10407,#10408,#5336,.T.);
#12698=EDGE_CURVE('',#10408,#10408,#9281,.T.);
#12699=EDGE_CURVE('',#10409,#10409,#9282,.T.);
#12700=EDGE_CURVE('',#10409,#10410,#5337,.T.);
#12701=EDGE_CURVE('',#10410,#10410,#9283,.T.);
#12702=EDGE_CURVE('',#10411,#10412,#5338,.T.);
#12703=EDGE_CURVE('',#10412,#10413,#9284,.T.);
#12704=EDGE_CURVE('',#10413,#10414,#9285,.T.);
#12705=EDGE_CURVE('',#10414,#10415,#9286,.T.);
#12706=EDGE_CURVE('',#10415,#10416,#9287,.T.);
#12707=EDGE_CURVE('',#10416,#10417,#9288,.T.);
#12708=EDGE_CURVE('',#10417,#10412,#9289,.T.);
#12709=EDGE_CURVE('',#10418,#10419,#5339,.T.);
#12710=EDGE_CURVE('',#10419,#10420,#9290,.T.);
#12711=EDGE_CURVE('',#10420,#10421,#9291,.T.);
#12712=EDGE_CURVE('',#10421,#10422,#9292,.T.);
#12713=EDGE_CURVE('',#10422,#10423,#9293,.T.);
#12714=EDGE_CURVE('',#10423,#10424,#9294,.T.);
#12715=EDGE_CURVE('',#10424,#10419,#9295,.T.);
#12716=EDGE_CURVE('',#10425,#10426,#5340,.T.);
#12717=EDGE_CURVE('',#10426,#10427,#9296,.T.);
#12718=EDGE_CURVE('',#10427,#10428,#9297,.T.);
#12719=EDGE_CURVE('',#10428,#10429,#9298,.T.);
#12720=EDGE_CURVE('',#10429,#10430,#9299,.T.);
#12721=EDGE_CURVE('',#10430,#10431,#9300,.T.);
#12722=EDGE_CURVE('',#10431,#10426,#9301,.T.);
#12723=EDGE_CURVE('',#10432,#10433,#5341,.T.);
#12724=EDGE_CURVE('',#10433,#10434,#9302,.T.);
#12725=EDGE_CURVE('',#10434,#10435,#9303,.T.);
#12726=EDGE_CURVE('',#10435,#10436,#9304,.T.);
#12727=EDGE_CURVE('',#10436,#10437,#9305,.T.);
#12728=EDGE_CURVE('',#10437,#10438,#9306,.T.);
#12729=EDGE_CURVE('',#10438,#10433,#9307,.T.);
#12730=EDGE_CURVE('',#10439,#10439,#9308,.T.);
#12731=EDGE_CURVE('',#10439,#10440,#5342,.T.);
#12732=EDGE_CURVE('',#10440,#10440,#9309,.T.);
#12733=EDGE_CURVE('',#10441,#10441,#9310,.T.);
#12734=EDGE_CURVE('',#10441,#10442,#5343,.T.);
#12735=EDGE_CURVE('',#10442,#10442,#9311,.T.);
#12736=EDGE_CURVE('',#10443,#10443,#9312,.T.);
#12737=EDGE_CURVE('',#10443,#10444,#5344,.T.);
#12738=EDGE_CURVE('',#10444,#10444,#9313,.T.);
#12739=EDGE_CURVE('',#10445,#10445,#9314,.T.);
#12740=EDGE_CURVE('',#10445,#10446,#5345,.T.);
#12741=EDGE_CURVE('',#10446,#10446,#9315,.T.);
#12742=EDGE_CURVE('',#10447,#10447,#9316,.T.);
#12743=EDGE_CURVE('',#10447,#10448,#5346,.T.);
#12744=EDGE_CURVE('',#10448,#10448,#9317,.T.);
#12745=EDGE_CURVE('',#10449,#10449,#9318,.T.);
#12746=EDGE_CURVE('',#10449,#10450,#5347,.T.);
#12747=EDGE_CURVE('',#10450,#10450,#9319,.T.);
#12748=EDGE_CURVE('',#10451,#10451,#9320,.T.);
#12749=EDGE_CURVE('',#10451,#10452,#5348,.T.);
#12750=EDGE_CURVE('',#10452,#10452,#9321,.T.);
#12751=EDGE_CURVE('',#10453,#10453,#9322,.T.);
#12752=EDGE_CURVE('',#10453,#10454,#5349,.T.);
#12753=EDGE_CURVE('',#10454,#10454,#9323,.T.);
#12754=EDGE_CURVE('',#10455,#10456,#5350,.T.);
#12755=EDGE_CURVE('',#10456,#10457,#5351,.T.);
#12756=EDGE_CURVE('',#10457,#10458,#5352,.T.);
#12757=EDGE_CURVE('',#10458,#10459,#5353,.T.);
#12758=EDGE_CURVE('',#10459,#10460,#5354,.T.);
#12759=EDGE_CURVE('',#10460,#10461,#5355,.T.);
#12760=EDGE_CURVE('',#10461,#10462,#5356,.T.);
#12761=EDGE_CURVE('',#10462,#10463,#5357,.T.);
#12762=EDGE_CURVE('',#10463,#10464,#5358,.T.);
#12763=EDGE_CURVE('',#10464,#10465,#5359,.T.);
#12764=EDGE_CURVE('',#10465,#10466,#5360,.T.);
#12765=EDGE_CURVE('',#10466,#10455,#5361,.T.);
#12766=EDGE_CURVE('',#10467,#10468,#5362,.T.);
#12767=EDGE_CURVE('',#10469,#10467,#5363,.T.);
#12768=EDGE_CURVE('',#10470,#10469,#5364,.T.);
#12769=EDGE_CURVE('',#10471,#10470,#5365,.T.);
#12770=EDGE_CURVE('',#10472,#10471,#5366,.T.);
#12771=EDGE_CURVE('',#10473,#10472,#5367,.T.);
#12772=EDGE_CURVE('',#10474,#10473,#5368,.T.);
#12773=EDGE_CURVE('',#10468,#10474,#5369,.T.);
#12774=EDGE_CURVE('',#10475,#10476,#5370,.T.);
#12775=EDGE_CURVE('',#10456,#10476,#5371,.T.);
#12776=EDGE_CURVE('',#10455,#10475,#5372,.T.);
#12777=EDGE_CURVE('',#10476,#10477,#5373,.T.);
#12778=EDGE_CURVE('',#10457,#10477,#5374,.T.);
#12779=EDGE_CURVE('',#10477,#10478,#5375,.T.);
#12780=EDGE_CURVE('',#10458,#10478,#5376,.T.);
#12781=EDGE_CURVE('',#10478,#10479,#5377,.T.);
#12782=EDGE_CURVE('',#10459,#10479,#5378,.T.);
#12783=EDGE_CURVE('',#10479,#10480,#5379,.T.);
#12784=EDGE_CURVE('',#10460,#10480,#5380,.T.);
#12785=EDGE_CURVE('',#10480,#10481,#5381,.T.);
#12786=EDGE_CURVE('',#10461,#10481,#5382,.T.);
#12787=EDGE_CURVE('',#10481,#10482,#5383,.T.);
#12788=EDGE_CURVE('',#10462,#10482,#5384,.T.);
#12789=EDGE_CURVE('',#10482,#10483,#5385,.T.);
#12790=EDGE_CURVE('',#10463,#10483,#5386,.T.);
#12791=EDGE_CURVE('',#10483,#10484,#5387,.T.);
#12792=EDGE_CURVE('',#10464,#10484,#5388,.T.);
#12793=EDGE_CURVE('',#10484,#10485,#5389,.T.);
#12794=EDGE_CURVE('',#10465,#10485,#5390,.T.);
#12795=EDGE_CURVE('',#10485,#10486,#5391,.T.);
#12796=EDGE_CURVE('',#10466,#10486,#5392,.T.);
#12797=EDGE_CURVE('',#10486,#10475,#5393,.T.);
#12798=EDGE_CURVE('',#10487,#10488,#5394,.T.);
#12799=EDGE_CURVE('',#10488,#10489,#5395,.T.);
#12800=EDGE_CURVE('',#10489,#10490,#5396,.T.);
#12801=EDGE_CURVE('',#10490,#10491,#5397,.T.);
#12802=EDGE_CURVE('',#10491,#10492,#5398,.T.);
#12803=EDGE_CURVE('',#10492,#10493,#5399,.T.);
#12804=EDGE_CURVE('',#10493,#10494,#5400,.T.);
#12805=EDGE_CURVE('',#10494,#10487,#5401,.T.);
#12806=EDGE_CURVE('',#10488,#10467,#5402,.T.);
#12807=EDGE_CURVE('',#10487,#10469,#5403,.T.);
#12808=EDGE_CURVE('',#10489,#10468,#5404,.T.);
#12809=EDGE_CURVE('',#10490,#10474,#5405,.T.);
#12810=EDGE_CURVE('',#10491,#10473,#5406,.T.);
#12811=EDGE_CURVE('',#10492,#10472,#5407,.T.);
#12812=EDGE_CURVE('',#10493,#10471,#5408,.T.);
#12813=EDGE_CURVE('',#10494,#10470,#5409,.T.);
#12814=EDGE_CURVE('',#10495,#10496,#5410,.T.);
#12815=EDGE_CURVE('',#10497,#10495,#5411,.T.);
#12816=EDGE_CURVE('',#10498,#10497,#5412,.T.);
#12817=EDGE_CURVE('',#10499,#10498,#5413,.T.);
#12818=EDGE_CURVE('',#10500,#10499,#5414,.T.);
#12819=EDGE_CURVE('',#10496,#10500,#5415,.T.);
#12820=EDGE_CURVE('',#10501,#10502,#5416,.T.);
#12821=EDGE_CURVE('',#10503,#10501,#5417,.T.);
#12822=EDGE_CURVE('',#10504,#10503,#5418,.T.);
#12823=EDGE_CURVE('',#10505,#10504,#5419,.T.);
#12824=EDGE_CURVE('',#10506,#10505,#5420,.T.);
#12825=EDGE_CURVE('',#10502,#10506,#5421,.T.);
#12826=EDGE_CURVE('',#10507,#10508,#5422,.T.);
#12827=EDGE_CURVE('',#10509,#10507,#5423,.T.);
#12828=EDGE_CURVE('',#10510,#10509,#5424,.T.);
#12829=EDGE_CURVE('',#10511,#10510,#5425,.T.);
#12830=EDGE_CURVE('',#10512,#10511,#5426,.T.);
#12831=EDGE_CURVE('',#10508,#10512,#5427,.T.);
#12832=EDGE_CURVE('',#10513,#10514,#5428,.T.);
#12833=EDGE_CURVE('',#10515,#10513,#5429,.T.);
#12834=EDGE_CURVE('',#10516,#10515,#5430,.T.);
#12835=EDGE_CURVE('',#10517,#10516,#5431,.T.);
#12836=EDGE_CURVE('',#10518,#10517,#5432,.T.);
#12837=EDGE_CURVE('',#10514,#10518,#5433,.T.);
#12838=EDGE_CURVE('',#10519,#10499,#5434,.T.);
#12839=EDGE_CURVE('',#10434,#10519,#5435,.T.);
#12840=EDGE_CURVE('',#10520,#10434,#5436,.T.);
#12841=EDGE_CURVE('',#10520,#10500,#5437,.T.);
#12842=EDGE_CURVE('',#10433,#10520,#5438,.T.);
#12843=EDGE_CURVE('',#10521,#10433,#5439,.T.);
#12844=EDGE_CURVE('',#10521,#10496,#5440,.T.);
#12845=EDGE_CURVE('',#10438,#10521,#5441,.T.);
#12846=EDGE_CURVE('',#10522,#10438,#5442,.T.);
#12847=EDGE_CURVE('',#10522,#10495,#5443,.T.);
#12848=EDGE_CURVE('',#10437,#10522,#5444,.T.);
#12849=EDGE_CURVE('',#10523,#10437,#5445,.T.);
#12850=EDGE_CURVE('',#10523,#10497,#5446,.T.);
#12851=EDGE_CURVE('',#10436,#10523,#5447,.T.);
#12852=EDGE_CURVE('',#10524,#10436,#5448,.T.);
#12853=EDGE_CURVE('',#10524,#10498,#5449,.T.);
#12854=EDGE_CURVE('',#10435,#10524,#5450,.T.);
#12855=EDGE_CURVE('',#10519,#10435,#5451,.T.);
#12856=EDGE_CURVE('',#10525,#10505,#5452,.T.);
#12857=EDGE_CURVE('',#10428,#10525,#5453,.T.);
#12858=EDGE_CURVE('',#10526,#10428,#5454,.T.);
#12859=EDGE_CURVE('',#10526,#10506,#5455,.T.);
#12860=EDGE_CURVE('',#10427,#10526,#5456,.T.);
#12861=EDGE_CURVE('',#10527,#10427,#5457,.T.);
#12862=EDGE_CURVE('',#10527,#10502,#5458,.T.);
#12863=EDGE_CURVE('',#10426,#10527,#5459,.T.);
#12864=EDGE_CURVE('',#10528,#10426,#5460,.T.);
#12865=EDGE_CURVE('',#10528,#10501,#5461,.T.);
#12866=EDGE_CURVE('',#10431,#10528,#5462,.T.);
#12867=EDGE_CURVE('',#10529,#10431,#5463,.T.);
#12868=EDGE_CURVE('',#10529,#10503,#5464,.T.);
#12869=EDGE_CURVE('',#10430,#10529,#5465,.T.);
#12870=EDGE_CURVE('',#10530,#10430,#5466,.T.);
#12871=EDGE_CURVE('',#10530,#10504,#5467,.T.);
#12872=EDGE_CURVE('',#10429,#10530,#5468,.T.);
#12873=EDGE_CURVE('',#10525,#10429,#5469,.T.);
#12874=EDGE_CURVE('',#10531,#10517,#5470,.T.);
#12875=EDGE_CURVE('',#10421,#10531,#5471,.T.);
#12876=EDGE_CURVE('',#10532,#10421,#5472,.T.);
#12877=EDGE_CURVE('',#10532,#10518,#5473,.T.);
#12878=EDGE_CURVE('',#10420,#10532,#5474,.T.);
#12879=EDGE_CURVE('',#10533,#10420,#5475,.T.);
#12880=EDGE_CURVE('',#10533,#10514,#5476,.T.);
#12881=EDGE_CURVE('',#10419,#10533,#5477,.T.);
#12882=EDGE_CURVE('',#10534,#10419,#5478,.T.);
#12883=EDGE_CURVE('',#10534,#10513,#5479,.T.);
#12884=EDGE_CURVE('',#10424,#10534,#5480,.T.);
#12885=EDGE_CURVE('',#10535,#10424,#5481,.T.);
#12886=EDGE_CURVE('',#10535,#10515,#5482,.T.);
#12887=EDGE_CURVE('',#10423,#10535,#5483,.T.);
#12888=EDGE_CURVE('',#10536,#10423,#5484,.T.);
#12889=EDGE_CURVE('',#10536,#10516,#5485,.T.);
#12890=EDGE_CURVE('',#10422,#10536,#5486,.T.);
#12891=EDGE_CURVE('',#10531,#10422,#5487,.T.);
#12892=EDGE_CURVE('',#10537,#10511,#5488,.T.);
#12893=EDGE_CURVE('',#10414,#10537,#5489,.T.);
#12894=EDGE_CURVE('',#10538,#10414,#5490,.T.);
#12895=EDGE_CURVE('',#10538,#10512,#5491,.T.);
#12896=EDGE_CURVE('',#10413,#10538,#5492,.T.);
#12897=EDGE_CURVE('',#10539,#10413,#5493,.T.);
#12898=EDGE_CURVE('',#10539,#10508,#5494,.T.);
#12899=EDGE_CURVE('',#10412,#10539,#5495,.T.);
#12900=EDGE_CURVE('',#10540,#10412,#5496,.T.);
#12901=EDGE_CURVE('',#10540,#10507,#5497,.T.);
#12902=EDGE_CURVE('',#10417,#10540,#5498,.T.);
#12903=EDGE_CURVE('',#10541,#10417,#5499,.T.);
#12904=EDGE_CURVE('',#10541,#10509,#5500,.T.);
#12905=EDGE_CURVE('',#10416,#10541,#5501,.T.);
#12906=EDGE_CURVE('',#10542,#10416,#5502,.T.);
#12907=EDGE_CURVE('',#10542,#10510,#5503,.T.);
#12908=EDGE_CURVE('',#10415,#10542,#5504,.T.);
#12909=EDGE_CURVE('',#10537,#10415,#5505,.T.);
#12910=EDGE_CURVE('',#10543,#10543,#662,.T.);
#12911=EDGE_CURVE('',#10543,#10544,#5506,.T.);
#12912=EDGE_CURVE('',#10544,#10544,#663,.T.);
#12913=EDGE_CURVE('',#10545,#10546,#9324,.T.);
#12914=EDGE_CURVE('',#10546,#10547,#5507,.T.);
#12915=EDGE_CURVE('',#10547,#10547,#9325,.T.);
#12916=EDGE_CURVE('',#10546,#10545,#9326,.T.);
#12917=EDGE_CURVE('',#10548,#10548,#9327,.T.);
#12918=EDGE_CURVE('',#10548,#10549,#5508,.T.);
#12919=EDGE_CURVE('',#10549,#10549,#9328,.T.);
#12920=EDGE_CURVE('',#10545,#10548,#5509,.T.);
#12921=EDGE_CURVE('',#10550,#10551,#9329,.T.);
#12922=EDGE_CURVE('',#10551,#10552,#5510,.T.);
#12923=EDGE_CURVE('',#10553,#10552,#9330,.T.);
#12924=EDGE_CURVE('',#10553,#10550,#5511,.T.);
#12925=EDGE_CURVE('',#10554,#10554,#9331,.T.);
#12926=EDGE_CURVE('',#10554,#10555,#5512,.T.);
#12927=EDGE_CURVE('',#10555,#10555,#9332,.T.);
#12928=EDGE_CURVE('',#10556,#10557,#9333,.T.);
#12929=EDGE_CURVE('',#10557,#10558,#5513,.T.);
#12930=EDGE_CURVE('',#10559,#10558,#9334,.T.);
#12931=EDGE_CURVE('',#10559,#10556,#5514,.T.);
#12932=EDGE_CURVE('',#10560,#10561,#9335,.T.);
#12933=EDGE_CURVE('',#10561,#10562,#5515,.T.);
#12934=EDGE_CURVE('',#10563,#10562,#9336,.T.);
#12935=EDGE_CURVE('',#10563,#10560,#5516,.T.);
#12936=EDGE_CURVE('',#10564,#10565,#9337,.T.);
#12937=EDGE_CURVE('',#10565,#10566,#5517,.T.);
#12938=EDGE_CURVE('',#10567,#10566,#9338,.T.);
#12939=EDGE_CURVE('',#10567,#10564,#5518,.T.);
#12940=EDGE_CURVE('',#10558,#10553,#5519,.T.);
#12941=EDGE_CURVE('',#10552,#10567,#5520,.T.);
#12942=EDGE_CURVE('',#10566,#10563,#5521,.T.);
#12943=EDGE_CURVE('',#10562,#10559,#5522,.T.);
#12944=EDGE_CURVE('',#10550,#10557,#5523,.T.);
#12945=EDGE_CURVE('',#10556,#10561,#5524,.T.);
#12946=EDGE_CURVE('',#10560,#10565,#5525,.T.);
#12947=EDGE_CURVE('',#10564,#10551,#5526,.T.);
#12948=EDGE_CURVE('',#10568,#10568,#9339,.T.);
#12949=EDGE_CURVE('',#10568,#10569,#5527,.T.);
#12950=EDGE_CURVE('',#10569,#10569,#9340,.T.);
#12951=EDGE_CURVE('',#10570,#10571,#9341,.T.);
#12952=EDGE_CURVE('',#10571,#10572,#5528,.T.);
#12953=EDGE_CURVE('',#10572,#10572,#9342,.T.);
#12954=EDGE_CURVE('',#10571,#10570,#9343,.T.);
#12955=EDGE_CURVE('',#10570,#10568,#5529,.T.);
#12956=EDGE_CURVE('',#10573,#10574,#5530,.T.);
#12957=EDGE_CURVE('',#10575,#10573,#5531,.T.);
#12958=EDGE_CURVE('',#10576,#10575,#5532,.T.);
#12959=EDGE_CURVE('',#10577,#10576,#5533,.T.);
#12960=EDGE_CURVE('',#10578,#10577,#5534,.T.);
#12961=EDGE_CURVE('',#10574,#10578,#5535,.T.);
#12962=EDGE_CURVE('',#10579,#10574,#5536,.T.);
#12963=EDGE_CURVE('',#10580,#10579,#5537,.T.);
#12964=EDGE_CURVE('',#10580,#10573,#5538,.T.);
#12965=EDGE_CURVE('',#10581,#10580,#5539,.T.);
#12966=EDGE_CURVE('',#10581,#10575,#5540,.T.);
#12967=EDGE_CURVE('',#10582,#10581,#5541,.T.);
#12968=EDGE_CURVE('',#10582,#10576,#5542,.T.);
#12969=EDGE_CURVE('',#10583,#10582,#5543,.T.);
#12970=EDGE_CURVE('',#10583,#10577,#5544,.T.);
#12971=EDGE_CURVE('',#10584,#10583,#5545,.T.);
#12972=EDGE_CURVE('',#10584,#10578,#5546,.T.);
#12973=EDGE_CURVE('',#10579,#10584,#5547,.T.);
#12974=EDGE_CURVE('',#10585,#10585,#9344,.T.);
#12975=EDGE_CURVE('',#10585,#10586,#5548,.T.);
#12976=EDGE_CURVE('',#10586,#10586,#9345,.T.);
#12977=EDGE_CURVE('',#10587,#10587,#9346,.T.);
#12978=EDGE_CURVE('',#10587,#10588,#5549,.T.);
#12979=EDGE_CURVE('',#10588,#10588,#9347,.T.);
#12980=EDGE_CURVE('',#10589,#10589,#9348,.T.);
#12981=EDGE_CURVE('',#10589,#10590,#5550,.T.);
#12982=EDGE_CURVE('',#10590,#10590,#9349,.T.);
#12983=EDGE_CURVE('',#10591,#10591,#9350,.T.);
#12984=EDGE_CURVE('',#10591,#10592,#5551,.T.);
#12985=EDGE_CURVE('',#10592,#10592,#9351,.T.);
#12986=EDGE_CURVE('',#10593,#10593,#9352,.T.);
#12987=EDGE_CURVE('',#10593,#10594,#5552,.T.);
#12988=EDGE_CURVE('',#10594,#10594,#9353,.T.);
#12989=EDGE_CURVE('',#10595,#10596,#5553,.T.);
#12990=EDGE_CURVE('',#10596,#10597,#5554,.T.);
#12991=EDGE_CURVE('',#10597,#10598,#5555,.T.);
#12992=EDGE_CURVE('',#10598,#10599,#5556,.T.);
#12993=EDGE_CURVE('',#10599,#10600,#5557,.T.);
#12994=EDGE_CURVE('',#10600,#10601,#5558,.T.);
#12995=EDGE_CURVE('',#10601,#10602,#5559,.T.);
#12996=EDGE_CURVE('',#10602,#10603,#5560,.T.);
#12997=EDGE_CURVE('',#10603,#10604,#5561,.T.);
#12998=EDGE_CURVE('',#10604,#10605,#5562,.T.);
#12999=EDGE_CURVE('',#10605,#10606,#5563,.T.);
#13000=EDGE_CURVE('',#10606,#10595,#5564,.T.);
#13001=EDGE_CURVE('',#10607,#10608,#5565,.T.);
#13002=EDGE_CURVE('',#10609,#10607,#5566,.T.);
#13003=EDGE_CURVE('',#10610,#10609,#5567,.T.);
#13004=EDGE_CURVE('',#10611,#10610,#5568,.T.);
#13005=EDGE_CURVE('',#10612,#10611,#5569,.T.);
#13006=EDGE_CURVE('',#10613,#10612,#5570,.T.);
#13007=EDGE_CURVE('',#10614,#10613,#5571,.T.);
#13008=EDGE_CURVE('',#10615,#10614,#5572,.T.);
#13009=EDGE_CURVE('',#10616,#10615,#5573,.T.);
#13010=EDGE_CURVE('',#10617,#10616,#5574,.T.);
#13011=EDGE_CURVE('',#10618,#10617,#5575,.T.);
#13012=EDGE_CURVE('',#10608,#10618,#5576,.T.);
#13013=EDGE_CURVE('',#10596,#10608,#5577,.T.);
#13014=EDGE_CURVE('',#10595,#10607,#5578,.T.);
#13015=EDGE_CURVE('',#10597,#10618,#5579,.T.);
#13016=EDGE_CURVE('',#10598,#10617,#5580,.T.);
#13017=EDGE_CURVE('',#10599,#10616,#5581,.T.);
#13018=EDGE_CURVE('',#10600,#10615,#5582,.T.);
#13019=EDGE_CURVE('',#10601,#10614,#5583,.T.);
#13020=EDGE_CURVE('',#10602,#10613,#5584,.T.);
#13021=EDGE_CURVE('',#10603,#10612,#5585,.T.);
#13022=EDGE_CURVE('',#10604,#10611,#5586,.T.);
#13023=EDGE_CURVE('',#10605,#10610,#5587,.T.);
#13024=EDGE_CURVE('',#10606,#10609,#5588,.T.);
#13025=EDGE_CURVE('',#10619,#10619,#9354,.T.);
#13026=EDGE_CURVE('',#10619,#10620,#9355,.T.);
#13027=EDGE_CURVE('',#10620,#10620,#9356,.T.);
#13028=EDGE_CURVE('',#10620,#10621,#5589,.T.);
#13029=EDGE_CURVE('',#10621,#10621,#9357,.T.);
#13030=EDGE_CURVE('',#10621,#10622,#9358,.T.);
#13031=EDGE_CURVE('',#10622,#10622,#9359,.T.);
#13032=EDGE_CURVE('',#10623,#10623,#9360,.T.);
#13033=EDGE_CURVE('',#10623,#10624,#5590,.T.);
#13034=EDGE_CURVE('',#10624,#10624,#9361,.T.);
#13035=EDGE_CURVE('',#10625,#10625,#9362,.T.);
#13036=EDGE_CURVE('',#10625,#10626,#5591,.T.);
#13037=EDGE_CURVE('',#10626,#10626,#9363,.T.);
#13038=EDGE_CURVE('',#10627,#10627,#9364,.T.);
#13039=EDGE_CURVE('',#10627,#10628,#9365,.T.);
#13040=EDGE_CURVE('',#10628,#10628,#9366,.T.);
#13041=EDGE_CURVE('',#10628,#10629,#5592,.T.);
#13042=EDGE_CURVE('',#10629,#10629,#9367,.T.);
#13043=EDGE_CURVE('',#10629,#10630,#9368,.T.);
#13044=EDGE_CURVE('',#10630,#10630,#9369,.T.);
#13045=EDGE_CURVE('',#10631,#10631,#9370,.T.);
#13046=EDGE_CURVE('',#10631,#10632,#5593,.T.);
#13047=EDGE_CURVE('',#10632,#10632,#9371,.T.);
#13048=EDGE_CURVE('',#10633,#10633,#9372,.T.);
#13049=EDGE_CURVE('',#10633,#10634,#5594,.T.);
#13050=EDGE_CURVE('',#10634,#10634,#9373,.T.);
#13051=EDGE_CURVE('',#10635,#10635,#9374,.T.);
#13052=EDGE_CURVE('',#10635,#10636,#5595,.T.);
#13053=EDGE_CURVE('',#10636,#10636,#9375,.T.);
#13054=EDGE_CURVE('',#10637,#10637,#9376,.T.);
#13055=EDGE_CURVE('',#10637,#10638,#5596,.T.);
#13056=EDGE_CURVE('',#10638,#10638,#9377,.T.);
#13057=EDGE_CURVE('',#10639,#10640,#9378,.T.);
#13058=EDGE_CURVE('',#10639,#10641,#5597,.T.);
#13059=EDGE_CURVE('',#10641,#10642,#9379,.T.);
#13060=EDGE_CURVE('',#10640,#10642,#5598,.T.);
#13061=EDGE_CURVE('',#10643,#10644,#9380,.T.);
#13062=EDGE_CURVE('',#10643,#10645,#5599,.T.);
#13063=EDGE_CURVE('',#10645,#10646,#9381,.T.);
#13064=EDGE_CURVE('',#10644,#10646,#5600,.T.);
#13065=EDGE_CURVE('',#10647,#10648,#5601,.T.);
#13066=EDGE_CURVE('',#10648,#10649,#9382,.T.);
#13067=EDGE_CURVE('',#10649,#10650,#5602,.T.);
#13068=EDGE_CURVE('',#10650,#10643,#9383,.T.);
#13069=EDGE_CURVE('',#10644,#10651,#9384,.T.);
#13070=EDGE_CURVE('',#10651,#10652,#5603,.T.);
#13071=EDGE_CURVE('',#10652,#10653,#9385,.T.);
#13072=EDGE_CURVE('',#10653,#10654,#5604,.T.);
#13073=EDGE_CURVE('',#10654,#10639,#5605,.T.);
#13074=EDGE_CURVE('',#10640,#10647,#5606,.T.);
#13075=EDGE_CURVE('',#10655,#10656,#5607,.T.);
#13076=EDGE_CURVE('',#10642,#10655,#5608,.T.);
#13077=EDGE_CURVE('',#10657,#10641,#5609,.T.);
#13078=EDGE_CURVE('',#10658,#10657,#5610,.T.);
#13079=EDGE_CURVE('',#10659,#10658,#9386,.T.);
#13080=EDGE_CURVE('',#10660,#10659,#5611,.T.);
#13081=EDGE_CURVE('',#10646,#10660,#9387,.T.);
#13082=EDGE_CURVE('',#10661,#10645,#9388,.T.);
#13083=EDGE_CURVE('',#10662,#10661,#5612,.T.);
#13084=EDGE_CURVE('',#10656,#10662,#9389,.T.);
#13085=EDGE_CURVE('',#10648,#10656,#5613,.T.);
#13086=EDGE_CURVE('',#10647,#10655,#5614,.T.);
#13087=EDGE_CURVE('',#10649,#10662,#5615,.T.);
#13088=EDGE_CURVE('',#10650,#10661,#5616,.T.);
#13089=EDGE_CURVE('',#10651,#10660,#5617,.T.);
#13090=EDGE_CURVE('',#10652,#10659,#5618,.T.);
#13091=EDGE_CURVE('',#10653,#10658,#5619,.T.);
#13092=EDGE_CURVE('',#10654,#10657,#5620,.T.);
#13093=EDGE_CURVE('',#10663,#10663,#9390,.T.);
#13094=EDGE_CURVE('',#10663,#10664,#5621,.T.);
#13095=EDGE_CURVE('',#10664,#10664,#9391,.T.);
#13096=EDGE_CURVE('',#10665,#10665,#9392,.T.);
#13097=EDGE_CURVE('',#10665,#10666,#5622,.T.);
#13098=EDGE_CURVE('',#10666,#10666,#9393,.T.);
#13099=EDGE_CURVE('',#10667,#10667,#9394,.T.);
#13100=EDGE_CURVE('',#10667,#10668,#5623,.T.);
#13101=EDGE_CURVE('',#10668,#10668,#9395,.T.);
#13102=EDGE_CURVE('',#10669,#10669,#9396,.T.);
#13103=EDGE_CURVE('',#10669,#10670,#5624,.T.);
#13104=EDGE_CURVE('',#10670,#10670,#9397,.T.);
#13105=EDGE_CURVE('',#10671,#10672,#5625,.T.);
#13106=EDGE_CURVE('',#10673,#10671,#5626,.T.);
#13107=EDGE_CURVE('',#10673,#10674,#5627,.T.);
#13108=EDGE_CURVE('',#10674,#10672,#5628,.T.);
#13109=EDGE_CURVE('',#10675,#10673,#5629,.T.);
#13110=EDGE_CURVE('',#10676,#10675,#5630,.T.);
#13111=EDGE_CURVE('',#10676,#10677,#5631,.T.);
#13112=EDGE_CURVE('',#10677,#10678,#5632,.T.);
#13113=EDGE_CURVE('',#10674,#10678,#5633,.T.);
#13114=EDGE_CURVE('',#10679,#10680,#5634,.T.);
#13115=EDGE_CURVE('',#10679,#10672,#5635,.T.);
#13116=EDGE_CURVE('',#10678,#10681,#5636,.T.);
#13117=EDGE_CURVE('',#10680,#10681,#5637,.T.);
#13118=EDGE_CURVE('',#10682,#10683,#5638,.T.);
#13119=EDGE_CURVE('',#10684,#10682,#5639,.T.);
#13120=EDGE_CURVE('',#10680,#10684,#5640,.T.);
#13121=EDGE_CURVE('',#10681,#10685,#5641,.T.);
#13122=EDGE_CURVE('',#10683,#10685,#5642,.T.);
#13123=EDGE_CURVE('',#10686,#10676,#5643,.T.);
#13124=EDGE_CURVE('',#10686,#10687,#5644,.T.);
#13125=EDGE_CURVE('',#10683,#10687,#5645,.T.);
#13126=EDGE_CURVE('',#10685,#10677,#5646,.T.);
#13127=EDGE_CURVE('',#10688,#10687,#5647,.T.);
#13128=EDGE_CURVE('',#10682,#10688,#5648,.T.);
#13129=EDGE_CURVE('',#10689,#10679,#5649,.T.);
#13130=EDGE_CURVE('',#10689,#10671,#5650,.T.);
#13131=EDGE_CURVE('',#10675,#10689,#5651,.T.);
#13132=EDGE_CURVE('',#10690,#10686,#5652,.T.);
#13133=EDGE_CURVE('',#10690,#10688,#5653,.T.);
#13134=EDGE_CURVE('',#10684,#10690,#5654,.T.);
#13135=EDGE_CURVE('',#10691,#10691,#9398,.T.);
#13136=EDGE_CURVE('',#10691,#10692,#5655,.T.);
#13137=EDGE_CURVE('',#10692,#10692,#9399,.T.);
#13138=EDGE_CURVE('',#10693,#10693,#9400,.T.);
#13139=EDGE_CURVE('',#10693,#10694,#5656,.T.);
#13140=EDGE_CURVE('',#10694,#10694,#9401,.T.);
#13141=EDGE_CURVE('',#10695,#10695,#9402,.T.);
#13142=EDGE_CURVE('',#10695,#10696,#5657,.T.);
#13143=EDGE_CURVE('',#10696,#10696,#9403,.T.);
#13144=EDGE_CURVE('',#10697,#10697,#9404,.T.);
#13145=EDGE_CURVE('',#10697,#10698,#5658,.T.);
#13146=EDGE_CURVE('',#10698,#10698,#9405,.T.);
#13147=EDGE_CURVE('',#10699,#10700,#5659,.T.);
#13148=EDGE_CURVE('',#10701,#10699,#5660,.T.);
#13149=EDGE_CURVE('',#10701,#10702,#5661,.T.);
#13150=EDGE_CURVE('',#10702,#10700,#5662,.T.);
#13151=EDGE_CURVE('',#10703,#10701,#5663,.T.);
#13152=EDGE_CURVE('',#10704,#10703,#5664,.T.);
#13153=EDGE_CURVE('',#10704,#10705,#5665,.T.);
#13154=EDGE_CURVE('',#10705,#10706,#5666,.T.);
#13155=EDGE_CURVE('',#10702,#10706,#5667,.T.);
#13156=EDGE_CURVE('',#10707,#10708,#5668,.T.);
#13157=EDGE_CURVE('',#10707,#10700,#5669,.T.);
#13158=EDGE_CURVE('',#10706,#10709,#5670,.T.);
#13159=EDGE_CURVE('',#10708,#10709,#5671,.T.);
#13160=EDGE_CURVE('',#10710,#10711,#5672,.T.);
#13161=EDGE_CURVE('',#10712,#10710,#5673,.T.);
#13162=EDGE_CURVE('',#10708,#10712,#5674,.T.);
#13163=EDGE_CURVE('',#10709,#10713,#5675,.T.);
#13164=EDGE_CURVE('',#10711,#10713,#5676,.T.);
#13165=EDGE_CURVE('',#10714,#10704,#5677,.T.);
#13166=EDGE_CURVE('',#10714,#10715,#5678,.T.);
#13167=EDGE_CURVE('',#10711,#10715,#5679,.T.);
#13168=EDGE_CURVE('',#10713,#10705,#5680,.T.);
#13169=EDGE_CURVE('',#10716,#10715,#5681,.T.);
#13170=EDGE_CURVE('',#10710,#10716,#5682,.T.);
#13171=EDGE_CURVE('',#10717,#10707,#5683,.T.);
#13172=EDGE_CURVE('',#10717,#10699,#5684,.T.);
#13173=EDGE_CURVE('',#10703,#10717,#5685,.T.);
#13174=EDGE_CURVE('',#10718,#10714,#5686,.T.);
#13175=EDGE_CURVE('',#10718,#10716,#5687,.T.);
#13176=EDGE_CURVE('',#10712,#10718,#5688,.T.);
#13177=EDGE_CURVE('',#10719,#10719,#9406,.T.);
#13178=EDGE_CURVE('',#10719,#10720,#5689,.T.);
#13179=EDGE_CURVE('',#10720,#10720,#9407,.T.);
#13180=EDGE_CURVE('',#10721,#10721,#9408,.T.);
#13181=EDGE_CURVE('',#10721,#10722,#5690,.T.);
#13182=EDGE_CURVE('',#10722,#10722,#9409,.T.);
#13183=EDGE_CURVE('',#10723,#10723,#9410,.T.);
#13184=EDGE_CURVE('',#10723,#10724,#5691,.T.);
#13185=EDGE_CURVE('',#10724,#10724,#9411,.T.);
#13186=EDGE_CURVE('',#10725,#10725,#9412,.T.);
#13187=EDGE_CURVE('',#10725,#10726,#5692,.T.);
#13188=EDGE_CURVE('',#10726,#10726,#9413,.T.);
#13189=EDGE_CURVE('',#10727,#10727,#9414,.T.);
#13190=EDGE_CURVE('',#10727,#10728,#5693,.T.);
#13191=EDGE_CURVE('',#10728,#10728,#9415,.T.);
#13192=EDGE_CURVE('',#10729,#10729,#9416,.T.);
#13193=EDGE_CURVE('',#10729,#10730,#5694,.T.);
#13194=EDGE_CURVE('',#10730,#10730,#9417,.T.);
#13195=EDGE_CURVE('',#10731,#10731,#9418,.T.);
#13196=EDGE_CURVE('',#10731,#10732,#5695,.T.);
#13197=EDGE_CURVE('',#10732,#10732,#9419,.T.);
#13198=EDGE_CURVE('',#10733,#10733,#9420,.T.);
#13199=EDGE_CURVE('',#10733,#10734,#5696,.T.);
#13200=EDGE_CURVE('',#10734,#10734,#9421,.T.);
#13201=EDGE_CURVE('',#10735,#10735,#9422,.T.);
#13202=EDGE_CURVE('',#10735,#10736,#5697,.T.);
#13203=EDGE_CURVE('',#10736,#10736,#9423,.T.);
#13204=EDGE_CURVE('',#10737,#10737,#9424,.T.);
#13205=EDGE_CURVE('',#10737,#10738,#5698,.T.);
#13206=EDGE_CURVE('',#10738,#10738,#9425,.T.);
#13207=EDGE_CURVE('',#10739,#10739,#9426,.T.);
#13208=EDGE_CURVE('',#10739,#10740,#5699,.T.);
#13209=EDGE_CURVE('',#10740,#10740,#9427,.T.);
#13210=EDGE_CURVE('',#10741,#10741,#9428,.T.);
#13211=EDGE_CURVE('',#10741,#10742,#5700,.T.);
#13212=EDGE_CURVE('',#10742,#10742,#9429,.T.);
#13213=EDGE_CURVE('',#10743,#10744,#5701,.T.);
#13214=EDGE_CURVE('',#10744,#10745,#5702,.T.);
#13215=EDGE_CURVE('',#10745,#10746,#5703,.T.);
#13216=EDGE_CURVE('',#10746,#10743,#5704,.T.);
#13217=EDGE_CURVE('',#10747,#10748,#5705,.T.);
#13218=EDGE_CURVE('',#10744,#10748,#5706,.T.);
#13219=EDGE_CURVE('',#10743,#10747,#5707,.T.);
#13220=EDGE_CURVE('',#10748,#10749,#5708,.T.);
#13221=EDGE_CURVE('',#10745,#10749,#5709,.T.);
#13222=EDGE_CURVE('',#10749,#10750,#5710,.T.);
#13223=EDGE_CURVE('',#10746,#10750,#5711,.T.);
#13224=EDGE_CURVE('',#10750,#10747,#5712,.T.);
#13225=EDGE_CURVE('',#10751,#10751,#9430,.T.);
#13226=EDGE_CURVE('',#10751,#10752,#5713,.T.);
#13227=EDGE_CURVE('',#10752,#10752,#9431,.T.);
#13228=EDGE_CURVE('',#10753,#10753,#9432,.T.);
#13229=EDGE_CURVE('',#10753,#10754,#5714,.T.);
#13230=EDGE_CURVE('',#10754,#10754,#9433,.T.);
#13231=EDGE_CURVE('',#10755,#10755,#9434,.T.);
#13232=EDGE_CURVE('',#10756,#10756,#9435,.T.);
#13233=EDGE_CURVE('',#10756,#10755,#5715,.T.);
#13234=EDGE_CURVE('',#10757,#10758,#9436,.T.);
#13235=EDGE_CURVE('',#10759,#10757,#9437,.T.);
#13236=EDGE_CURVE('',#10758,#10759,#9438,.T.);
#13237=EDGE_CURVE('',#10760,#10759,#664,.T.);
#13238=EDGE_CURVE('',#10761,#10757,#665,.T.);
#13239=EDGE_CURVE('',#10760,#10761,#666,.T.);
#13240=EDGE_CURVE('',#10761,#10762,#9439,.T.);
#13241=EDGE_CURVE('',#10763,#10762,#667,.T.);
#13242=EDGE_CURVE('',#10760,#10763,#668,.T.);
#13243=EDGE_CURVE('',#10764,#10765,#9440,.T.);
#13244=EDGE_CURVE('',#10766,#10765,#669,.T.);
#13245=EDGE_CURVE('',#10767,#10766,#670,.T.);
#13246=EDGE_CURVE('',#10767,#10764,#671,.T.);
#13247=EDGE_CURVE('',#10768,#10767,#672,.T.);
#13248=EDGE_CURVE('',#10768,#10769,#9441,.T.);
#13249=EDGE_CURVE('',#10769,#10764,#673,.T.);
#13250=EDGE_CURVE('',#10770,#10771,#9442,.T.);
#13251=EDGE_CURVE('',#10771,#10772,#54,.T.);
#13252=EDGE_CURVE('',#10772,#10768,#9443,.T.);
#13253=EDGE_CURVE('',#10770,#10768,#674,.T.);
#13254=EDGE_CURVE('',#10769,#10772,#9444,.T.);
#13255=EDGE_CURVE('',#10773,#10772,#675,.T.);
#13256=EDGE_CURVE('',#10773,#10774,#9445,.T.);
#13257=EDGE_CURVE('',#10774,#10769,#676,.T.);
#13258=EDGE_CURVE('',#10774,#10775,#677,.T.);
#13259=EDGE_CURVE('',#10764,#10775,#678,.T.);
#13260=EDGE_CURVE('',#10775,#10776,#9446,.T.);
#13261=EDGE_CURVE('',#10765,#10776,#679,.T.);
#13262=EDGE_CURVE('',#10777,#10778,#680,.T.);
#13263=EDGE_CURVE('',#10776,#10778,#681,.T.);
#13264=EDGE_CURVE('',#10775,#10777,#682,.T.);
#13265=EDGE_CURVE('',#10774,#10779,#9447,.T.);
#13266=EDGE_CURVE('',#10779,#10777,#683,.T.);
#13267=EDGE_CURVE('',#10779,#10773,#9448,.T.);
#13268=EDGE_CURVE('',#10780,#10781,#9449,.T.);
#13269=EDGE_CURVE('',#10782,#10781,#684,.T.);
#13270=EDGE_CURVE('',#10783,#10782,#685,.T.);
#13271=EDGE_CURVE('',#10783,#10780,#686,.T.);
#13272=EDGE_CURVE('',#10783,#10784,#687,.T.);
#13273=EDGE_CURVE('',#10784,#10785,#9450,.T.);
#13274=EDGE_CURVE('',#10780,#10785,#688,.T.);
#13275=EDGE_CURVE('',#10785,#10786,#9451,.T.);
#13276=EDGE_CURVE('',#10786,#10784,#9452,.T.);
#13277=EDGE_CURVE('',#10786,#10773,#55,.T.);
#13278=EDGE_CURVE('',#10784,#10779,#689,.T.);
#13279=EDGE_CURVE('',#10786,#10771,#690,.T.);
#13280=EDGE_CURVE('',#10771,#10787,#9453,.T.);
#13281=EDGE_CURVE('',#10785,#10787,#691,.T.);
#13282=EDGE_CURVE('',#10787,#10770,#9454,.T.);
#13283=EDGE_CURVE('',#10788,#10789,#692,.T.);
#13284=EDGE_CURVE('',#10790,#10789,#693,.T.);
#13285=EDGE_CURVE('',#10791,#10790,#9455,.T.);
#13286=EDGE_CURVE('',#10791,#10788,#694,.T.);
#13287=EDGE_CURVE('',#10791,#10787,#695,.T.);
#13288=EDGE_CURVE('',#10788,#10770,#696,.T.);
#13289=EDGE_CURVE('',#10780,#10791,#697,.T.);
#13290=EDGE_CURVE('',#10781,#10790,#698,.T.);
#13291=EDGE_CURVE('',#10792,#10793,#9456,.T.);
#13292=EDGE_CURVE('',#10794,#10793,#699,.T.);
#13293=EDGE_CURVE('',#10795,#10794,#700,.T.);
#13294=EDGE_CURVE('',#10795,#10792,#701,.T.);
#13295=EDGE_CURVE('',#10796,#10795,#702,.T.);
#13296=EDGE_CURVE('',#10796,#10797,#9457,.T.);
#13297=EDGE_CURVE('',#10797,#10792,#703,.T.);
#13298=EDGE_CURVE('',#10798,#10799,#9458,.T.);
#13299=EDGE_CURVE('',#10799,#10800,#56,.T.);
#13300=EDGE_CURVE('',#10800,#10796,#9459,.T.);
#13301=EDGE_CURVE('',#10798,#10796,#704,.T.);
#13302=EDGE_CURVE('',#10797,#10800,#9460,.T.);
#13303=EDGE_CURVE('',#10801,#10800,#705,.T.);
#13304=EDGE_CURVE('',#10801,#10802,#9461,.T.);
#13305=EDGE_CURVE('',#10802,#10797,#706,.T.);
#13306=EDGE_CURVE('',#10802,#10803,#707,.T.);
#13307=EDGE_CURVE('',#10792,#10803,#708,.T.);
#13308=EDGE_CURVE('',#10803,#10804,#9462,.T.);
#13309=EDGE_CURVE('',#10793,#10804,#709,.T.);
#13310=EDGE_CURVE('',#10805,#10806,#710,.T.);
#13311=EDGE_CURVE('',#10804,#10806,#711,.T.);
#13312=EDGE_CURVE('',#10803,#10805,#712,.T.);
#13313=EDGE_CURVE('',#10802,#10807,#9463,.T.);
#13314=EDGE_CURVE('',#10807,#10805,#713,.T.);
#13315=EDGE_CURVE('',#10807,#10801,#9464,.T.);
#13316=EDGE_CURVE('',#10808,#10809,#9465,.T.);
#13317=EDGE_CURVE('',#10810,#10809,#714,.T.);
#13318=EDGE_CURVE('',#10811,#10810,#715,.T.);
#13319=EDGE_CURVE('',#10811,#10808,#716,.T.);
#13320=EDGE_CURVE('',#10811,#10812,#717,.T.);
#13321=EDGE_CURVE('',#10812,#10813,#9466,.T.);
#13322=EDGE_CURVE('',#10808,#10813,#718,.T.);
#13323=EDGE_CURVE('',#10813,#10814,#9467,.T.);
#13324=EDGE_CURVE('',#10814,#10812,#9468,.T.);
#13325=EDGE_CURVE('',#10814,#10801,#57,.T.);
#13326=EDGE_CURVE('',#10812,#10807,#719,.T.);
#13327=EDGE_CURVE('',#10814,#10799,#720,.T.);
#13328=EDGE_CURVE('',#10799,#10815,#9469,.T.);
#13329=EDGE_CURVE('',#10813,#10815,#721,.T.);
#13330=EDGE_CURVE('',#10815,#10798,#9470,.T.);
#13331=EDGE_CURVE('',#10816,#10817,#722,.T.);
#13332=EDGE_CURVE('',#10818,#10817,#723,.T.);
#13333=EDGE_CURVE('',#10819,#10818,#9471,.T.);
#13334=EDGE_CURVE('',#10819,#10816,#724,.T.);
#13335=EDGE_CURVE('',#10819,#10815,#725,.T.);
#13336=EDGE_CURVE('',#10816,#10798,#726,.T.);
#13337=EDGE_CURVE('',#10808,#10819,#727,.T.);
#13338=EDGE_CURVE('',#10809,#10818,#728,.T.);
#13339=EDGE_CURVE('',#10820,#10821,#9472,.T.);
#13340=EDGE_CURVE('',#10822,#10821,#729,.T.);
#13341=EDGE_CURVE('',#10823,#10822,#730,.T.);
#13342=EDGE_CURVE('',#10823,#10820,#731,.T.);
#13343=EDGE_CURVE('',#10824,#10823,#732,.T.);
#13344=EDGE_CURVE('',#10824,#10825,#9473,.T.);
#13345=EDGE_CURVE('',#10825,#10820,#733,.T.);
#13346=EDGE_CURVE('',#10826,#10827,#9474,.T.);
#13347=EDGE_CURVE('',#10827,#10828,#58,.T.);
#13348=EDGE_CURVE('',#10828,#10824,#9475,.T.);
#13349=EDGE_CURVE('',#10826,#10824,#734,.T.);
#13350=EDGE_CURVE('',#10825,#10828,#9476,.T.);
#13351=EDGE_CURVE('',#10829,#10828,#735,.T.);
#13352=EDGE_CURVE('',#10829,#10830,#9477,.T.);
#13353=EDGE_CURVE('',#10830,#10825,#736,.T.);
#13354=EDGE_CURVE('',#10830,#10831,#737,.T.);
#13355=EDGE_CURVE('',#10820,#10831,#738,.T.);
#13356=EDGE_CURVE('',#10831,#10832,#9478,.T.);
#13357=EDGE_CURVE('',#10821,#10832,#739,.T.);
#13358=EDGE_CURVE('',#10833,#10834,#740,.T.);
#13359=EDGE_CURVE('',#10832,#10834,#741,.T.);
#13360=EDGE_CURVE('',#10831,#10833,#742,.T.);
#13361=EDGE_CURVE('',#10830,#10835,#9479,.T.);
#13362=EDGE_CURVE('',#10835,#10833,#743,.T.);
#13363=EDGE_CURVE('',#10835,#10829,#9480,.T.);
#13364=EDGE_CURVE('',#10836,#10837,#9481,.T.);
#13365=EDGE_CURVE('',#10838,#10837,#744,.T.);
#13366=EDGE_CURVE('',#10839,#10838,#745,.T.);
#13367=EDGE_CURVE('',#10839,#10836,#746,.T.);
#13368=EDGE_CURVE('',#10839,#10840,#747,.T.);
#13369=EDGE_CURVE('',#10840,#10841,#9482,.T.);
#13370=EDGE_CURVE('',#10836,#10841,#748,.T.);
#13371=EDGE_CURVE('',#10841,#10842,#9483,.T.);
#13372=EDGE_CURVE('',#10842,#10840,#9484,.T.);
#13373=EDGE_CURVE('',#10842,#10829,#59,.T.);
#13374=EDGE_CURVE('',#10840,#10835,#749,.T.);
#13375=EDGE_CURVE('',#10842,#10827,#750,.T.);
#13376=EDGE_CURVE('',#10827,#10843,#9485,.T.);
#13377=EDGE_CURVE('',#10841,#10843,#751,.T.);
#13378=EDGE_CURVE('',#10843,#10826,#9486,.T.);
#13379=EDGE_CURVE('',#10844,#10845,#752,.T.);
#13380=EDGE_CURVE('',#10846,#10845,#753,.T.);
#13381=EDGE_CURVE('',#10847,#10846,#9487,.T.);
#13382=EDGE_CURVE('',#10847,#10844,#754,.T.);
#13383=EDGE_CURVE('',#10847,#10843,#755,.T.);
#13384=EDGE_CURVE('',#10844,#10826,#756,.T.);
#13385=EDGE_CURVE('',#10836,#10847,#757,.T.);
#13386=EDGE_CURVE('',#10837,#10846,#758,.T.);
#13387=EDGE_CURVE('',#10848,#10849,#9488,.T.);
#13388=EDGE_CURVE('',#10850,#10849,#759,.T.);
#13389=EDGE_CURVE('',#10851,#10850,#760,.T.);
#13390=EDGE_CURVE('',#10851,#10848,#761,.T.);
#13391=EDGE_CURVE('',#10852,#10851,#762,.T.);
#13392=EDGE_CURVE('',#10852,#10853,#9489,.T.);
#13393=EDGE_CURVE('',#10853,#10848,#763,.T.);
#13394=EDGE_CURVE('',#10854,#10855,#9490,.T.);
#13395=EDGE_CURVE('',#10855,#10856,#60,.T.);
#13396=EDGE_CURVE('',#10856,#10852,#9491,.T.);
#13397=EDGE_CURVE('',#10854,#10852,#764,.T.);
#13398=EDGE_CURVE('',#10853,#10856,#9492,.T.);
#13399=EDGE_CURVE('',#10857,#10856,#765,.T.);
#13400=EDGE_CURVE('',#10857,#10858,#9493,.T.);
#13401=EDGE_CURVE('',#10858,#10853,#766,.T.);
#13402=EDGE_CURVE('',#10858,#10859,#767,.T.);
#13403=EDGE_CURVE('',#10848,#10859,#768,.T.);
#13404=EDGE_CURVE('',#10859,#10860,#9494,.T.);
#13405=EDGE_CURVE('',#10849,#10860,#769,.T.);
#13406=EDGE_CURVE('',#10861,#10862,#770,.T.);
#13407=EDGE_CURVE('',#10860,#10862,#771,.T.);
#13408=EDGE_CURVE('',#10859,#10861,#772,.T.);
#13409=EDGE_CURVE('',#10858,#10863,#9495,.T.);
#13410=EDGE_CURVE('',#10863,#10861,#773,.T.);
#13411=EDGE_CURVE('',#10863,#10857,#9496,.T.);
#13412=EDGE_CURVE('',#10864,#10865,#9497,.T.);
#13413=EDGE_CURVE('',#10866,#10865,#774,.T.);
#13414=EDGE_CURVE('',#10867,#10866,#775,.T.);
#13415=EDGE_CURVE('',#10867,#10864,#776,.T.);
#13416=EDGE_CURVE('',#10867,#10868,#777,.T.);
#13417=EDGE_CURVE('',#10868,#10869,#9498,.T.);
#13418=EDGE_CURVE('',#10864,#10869,#778,.T.);
#13419=EDGE_CURVE('',#10869,#10870,#9499,.T.);
#13420=EDGE_CURVE('',#10870,#10868,#9500,.T.);
#13421=EDGE_CURVE('',#10870,#10857,#61,.T.);
#13422=EDGE_CURVE('',#10868,#10863,#779,.T.);
#13423=EDGE_CURVE('',#10870,#10855,#780,.T.);
#13424=EDGE_CURVE('',#10855,#10871,#9501,.T.);
#13425=EDGE_CURVE('',#10869,#10871,#781,.T.);
#13426=EDGE_CURVE('',#10871,#10854,#9502,.T.);
#13427=EDGE_CURVE('',#10872,#10873,#782,.T.);
#13428=EDGE_CURVE('',#10874,#10873,#783,.T.);
#13429=EDGE_CURVE('',#10875,#10874,#9503,.T.);
#13430=EDGE_CURVE('',#10875,#10872,#784,.T.);
#13431=EDGE_CURVE('',#10875,#10871,#785,.T.);
#13432=EDGE_CURVE('',#10872,#10854,#786,.T.);
#13433=EDGE_CURVE('',#10864,#10875,#787,.T.);
#13434=EDGE_CURVE('',#10865,#10874,#788,.T.);
#13435=EDGE_CURVE('',#10876,#10877,#9504,.T.);
#13436=EDGE_CURVE('',#10878,#10876,#9505,.T.);
#13437=EDGE_CURVE('',#10877,#10878,#9506,.T.);
#13438=EDGE_CURVE('',#10877,#10879,#62,.T.);
#13439=EDGE_CURVE('',#10879,#10880,#9507,.T.);
#13440=EDGE_CURVE('',#10876,#10880,#789,.T.);
#13441=EDGE_CURVE('',#10880,#10881,#9508,.T.);
#13442=EDGE_CURVE('',#10881,#10879,#9509,.T.);
#13443=EDGE_CURVE('',#10880,#10882,#790,.T.);
#13444=EDGE_CURVE('',#10881,#10883,#791,.T.);
#13445=EDGE_CURVE('',#10882,#10883,#792,.T.);
#13446=EDGE_CURVE('',#10883,#10884,#9510,.T.);
#13447=EDGE_CURVE('',#10885,#10884,#793,.T.);
#13448=EDGE_CURVE('',#10882,#10885,#794,.T.);
#13449=EDGE_CURVE('',#10886,#10887,#9511,.T.);
#13450=EDGE_CURVE('',#10884,#10887,#795,.T.);
#13451=EDGE_CURVE('',#10883,#10886,#796,.T.);
#13452=EDGE_CURVE('',#10888,#10881,#797,.T.);
#13453=EDGE_CURVE('',#10888,#10886,#798,.T.);
#13454=EDGE_CURVE('',#10889,#10879,#799,.T.);
#13455=EDGE_CURVE('',#10889,#10888,#9512,.T.);
#13456=EDGE_CURVE('',#10890,#10889,#9513,.T.);
#13457=EDGE_CURVE('',#10888,#10890,#9514,.T.);
#13458=EDGE_CURVE('',#10890,#10891,#800,.T.);
#13459=EDGE_CURVE('',#10886,#10891,#801,.T.);
#13460=EDGE_CURVE('',#10891,#10892,#802,.T.);
#13461=EDGE_CURVE('',#10887,#10892,#803,.T.);
#13462=EDGE_CURVE('',#10893,#10894,#9515,.T.);
#13463=EDGE_CURVE('',#10895,#10894,#804,.T.);
#13464=EDGE_CURVE('',#10896,#10895,#805,.T.);
#13465=EDGE_CURVE('',#10896,#10893,#806,.T.);
#13466=EDGE_CURVE('',#10897,#10896,#807,.T.);
#13467=EDGE_CURVE('',#10897,#10898,#9516,.T.);
#13468=EDGE_CURVE('',#10898,#10893,#808,.T.);
#13469=EDGE_CURVE('',#10899,#10900,#9517,.T.);
#13470=EDGE_CURVE('',#10900,#10901,#63,.T.);
#13471=EDGE_CURVE('',#10901,#10897,#9518,.T.);
#13472=EDGE_CURVE('',#10899,#10897,#809,.T.);
#13473=EDGE_CURVE('',#10898,#10901,#9519,.T.);
#13474=EDGE_CURVE('',#10902,#10901,#810,.T.);
#13475=EDGE_CURVE('',#10902,#10903,#9520,.T.);
#13476=EDGE_CURVE('',#10903,#10898,#811,.T.);
#13477=EDGE_CURVE('',#10903,#10904,#812,.T.);
#13478=EDGE_CURVE('',#10893,#10904,#813,.T.);
#13479=EDGE_CURVE('',#10904,#10905,#9521,.T.);
#13480=EDGE_CURVE('',#10894,#10905,#814,.T.);
#13481=EDGE_CURVE('',#10906,#10907,#815,.T.);
#13482=EDGE_CURVE('',#10905,#10907,#816,.T.);
#13483=EDGE_CURVE('',#10904,#10906,#817,.T.);
#13484=EDGE_CURVE('',#10903,#10908,#9522,.T.);
#13485=EDGE_CURVE('',#10908,#10906,#818,.T.);
#13486=EDGE_CURVE('',#10908,#10902,#9523,.T.);
#13487=EDGE_CURVE('',#10909,#10910,#9524,.T.);
#13488=EDGE_CURVE('',#10911,#10910,#819,.T.);
#13489=EDGE_CURVE('',#10912,#10911,#820,.T.);
#13490=EDGE_CURVE('',#10912,#10909,#821,.T.);
#13491=EDGE_CURVE('',#10912,#10913,#822,.T.);
#13492=EDGE_CURVE('',#10913,#10914,#9525,.T.);
#13493=EDGE_CURVE('',#10909,#10914,#823,.T.);
#13494=EDGE_CURVE('',#10914,#10915,#9526,.T.);
#13495=EDGE_CURVE('',#10915,#10913,#9527,.T.);
#13496=EDGE_CURVE('',#10915,#10902,#64,.T.);
#13497=EDGE_CURVE('',#10913,#10908,#824,.T.);
#13498=EDGE_CURVE('',#10915,#10900,#825,.T.);
#13499=EDGE_CURVE('',#10900,#10916,#9528,.T.);
#13500=EDGE_CURVE('',#10914,#10916,#826,.T.);
#13501=EDGE_CURVE('',#10916,#10899,#9529,.T.);
#13502=EDGE_CURVE('',#10917,#10918,#827,.T.);
#13503=EDGE_CURVE('',#10919,#10918,#828,.T.);
#13504=EDGE_CURVE('',#10920,#10919,#9530,.T.);
#13505=EDGE_CURVE('',#10920,#10917,#829,.T.);
#13506=EDGE_CURVE('',#10920,#10916,#830,.T.);
#13507=EDGE_CURVE('',#10917,#10899,#831,.T.);
#13508=EDGE_CURVE('',#10909,#10920,#832,.T.);
#13509=EDGE_CURVE('',#10910,#10919,#833,.T.);
#13510=EDGE_CURVE('',#10921,#10922,#834,.T.);
#13511=EDGE_CURVE('',#10766,#10922,#9531,.T.);
#13512=EDGE_CURVE('',#10763,#10778,#9532,.T.);
#13513=EDGE_CURVE('',#10762,#10921,#835,.T.);
#13514=EDGE_CURVE('',#10794,#10789,#9533,.T.);
#13515=EDGE_CURVE('',#10782,#10806,#9534,.T.);
#13516=EDGE_CURVE('',#10822,#10817,#9535,.T.);
#13517=EDGE_CURVE('',#10810,#10834,#9536,.T.);
#13518=EDGE_CURVE('',#10850,#10845,#9537,.T.);
#13519=EDGE_CURVE('',#10838,#10862,#9538,.T.);
#13520=EDGE_CURVE('',#10895,#10873,#9539,.T.);
#13521=EDGE_CURVE('',#10866,#10907,#9540,.T.);
#13522=EDGE_CURVE('',#10885,#10918,#9541,.T.);
#13523=EDGE_CURVE('',#10911,#10892,#9542,.T.);
#13524=EDGE_CURVE('',#10923,#10923,#9543,.T.);
#13525=EDGE_CURVE('',#10924,#10924,#9544,.T.);
#13526=EDGE_CURVE('',#10924,#10923,#5716,.T.);
#13527=EDGE_CURVE('',#10925,#10925,#9545,.T.);
#13528=EDGE_CURVE('',#10926,#10926,#9546,.T.);
#13529=EDGE_CURVE('',#10926,#10925,#5717,.T.);
#13530=EDGE_CURVE('',#10759,#10890,#836,.T.);
#13531=EDGE_CURVE('',#10758,#10889,#65,.T.);
#13532=EDGE_CURVE('',#10758,#10877,#837,.T.);
#13533=EDGE_CURVE('',#10757,#10878,#838,.T.);
#13534=EDGE_CURVE('',#10927,#10878,#839,.T.);
#13535=EDGE_CURVE('',#10761,#10927,#840,.T.);
#13536=EDGE_CURVE('',#10927,#10921,#9547,.T.);
#13537=EDGE_CURVE('',#10928,#10922,#841,.T.);
#13538=EDGE_CURVE('',#10927,#10928,#842,.T.);
#13539=EDGE_CURVE('',#10928,#10876,#843,.T.);
#13540=EDGE_CURVE('',#10929,#10929,#9548,.T.);
#13541=EDGE_CURVE('',#10929,#10930,#5718,.T.);
#13542=EDGE_CURVE('',#10930,#10930,#9549,.T.);
#13543=EDGE_CURVE('',#10931,#10931,#9550,.T.);
#13544=EDGE_CURVE('',#10931,#10932,#5719,.T.);
#13545=EDGE_CURVE('',#10932,#10932,#9551,.T.);
#13546=EDGE_CURVE('',#10933,#10933,#9552,.T.);
#13547=EDGE_CURVE('',#10934,#10935,#5720,.T.);
#13548=EDGE_CURVE('',#10935,#10936,#5721,.T.);
#13549=EDGE_CURVE('',#10936,#10937,#5722,.T.);
#13550=EDGE_CURVE('',#10937,#10938,#5723,.T.);
#13551=EDGE_CURVE('',#10938,#10939,#5724,.T.);
#13552=EDGE_CURVE('',#10939,#10934,#5725,.T.);
#13553=EDGE_CURVE('',#10940,#10940,#9553,.T.);
#13554=EDGE_CURVE('',#10933,#10940,#5726,.T.);
#13555=EDGE_CURVE('',#10941,#10942,#5727,.T.);
#13556=EDGE_CURVE('',#10943,#10941,#5728,.T.);
#13557=EDGE_CURVE('',#10944,#10943,#5729,.T.);
#13558=EDGE_CURVE('',#10945,#10944,#5730,.T.);
#13559=EDGE_CURVE('',#10946,#10945,#5731,.T.);
#13560=EDGE_CURVE('',#10942,#10946,#5732,.T.);
#13561=EDGE_CURVE('',#10941,#10939,#5733,.T.);
#13562=EDGE_CURVE('',#10942,#10934,#5734,.T.);
#13563=EDGE_CURVE('',#10943,#10938,#5735,.T.);
#13564=EDGE_CURVE('',#10944,#10937,#5736,.T.);
#13565=EDGE_CURVE('',#10945,#10936,#5737,.T.);
#13566=EDGE_CURVE('',#10946,#10935,#5738,.T.);
#13567=EDGE_CURVE('',#10947,#10948,#9554,.T.);
#13568=EDGE_CURVE('',#10949,#10948,#9555,.T.);
#13569=EDGE_CURVE('',#10949,#10950,#9556,.T.);
#13570=EDGE_CURVE('',#10950,#10947,#9557,.T.);
#13571=EDGE_CURVE('',#10951,#10951,#9558,.T.);
#13572=EDGE_CURVE('',#10952,#10953,#5739,.T.);
#13573=EDGE_CURVE('',#10953,#10954,#9559,.T.);
#13574=EDGE_CURVE('',#10954,#10955,#5740,.T.);
#13575=EDGE_CURVE('',#10955,#10952,#5741,.T.);
#13576=EDGE_CURVE('',#10956,#10956,#9560,.T.);
#13577=EDGE_CURVE('',#10956,#10951,#5742,.T.);
#13578=EDGE_CURVE('',#10957,#10958,#5743,.T.);
#13579=EDGE_CURVE('',#10958,#10959,#844,.T.);
#13580=EDGE_CURVE('',#10959,#10960,#5744,.T.);
#13581=EDGE_CURVE('',#10960,#10957,#9561,.T.);
#13582=EDGE_CURVE('',#10961,#10962,#9562,.T.);
#13583=EDGE_CURVE('',#10963,#10962,#9563,.T.);
#13584=EDGE_CURVE('',#10963,#10964,#9564,.T.);
#13585=EDGE_CURVE('',#10964,#10961,#9565,.T.);
#13586=EDGE_CURVE('',#10965,#10966,#9566,.T.);
#13587=EDGE_CURVE('',#10966,#10967,#9567,.T.);
#13588=EDGE_CURVE('',#10967,#10968,#9568,.T.);
#13589=EDGE_CURVE('',#10965,#10968,#9569,.T.);
#13590=EDGE_CURVE('',#10969,#10970,#9570,.T.);
#13591=EDGE_CURVE('',#10948,#10970,#5745,.T.);
#13592=EDGE_CURVE('',#10969,#10947,#5746,.T.);
#13593=EDGE_CURVE('',#10966,#10971,#5747,.T.);
#13594=EDGE_CURVE('',#10971,#10972,#9571,.T.);
#13595=EDGE_CURVE('',#10972,#10967,#5748,.T.);
#13596=EDGE_CURVE('',#10964,#10973,#5749,.T.);
#13597=EDGE_CURVE('',#10973,#10974,#9572,.T.);
#13598=EDGE_CURVE('',#10974,#10961,#5750,.T.);
#13599=EDGE_CURVE('',#10950,#10975,#5751,.T.);
#13600=EDGE_CURVE('',#10975,#10969,#9573,.T.);
#13601=EDGE_CURVE('',#10976,#10963,#5752,.T.);
#13602=EDGE_CURVE('',#10976,#10973,#9574,.T.);
#13603=EDGE_CURVE('',#10972,#10977,#9575,.T.);
#13604=EDGE_CURVE('',#10968,#10977,#5753,.T.);
#13605=EDGE_CURVE('',#10970,#10978,#9576,.T.);
#13606=EDGE_CURVE('',#10979,#10975,#9577,.T.);
#13607=EDGE_CURVE('',#10980,#10979,#9578,.T.);
#13608=EDGE_CURVE('',#10981,#10980,#9579,.T.);
#13609=EDGE_CURVE('',#10974,#10981,#9580,.T.);
#13610=EDGE_CURVE('',#10977,#10976,#9581,.T.);
#13611=EDGE_CURVE('',#10978,#10971,#9582,.T.);
#13612=EDGE_CURVE('',#10982,#10983,#5754,.T.);
#13613=EDGE_CURVE('',#10983,#10984,#5755,.T.);
#13614=EDGE_CURVE('',#10984,#10985,#5756,.T.);
#13615=EDGE_CURVE('',#10985,#10982,#9583,.T.);
#13616=EDGE_CURVE('',#10979,#10949,#5757,.T.);
#13617=EDGE_CURVE('',#10962,#10981,#5758,.T.);
#13618=EDGE_CURVE('',#10978,#10965,#5759,.T.);
#13619=EDGE_CURVE('',#10954,#10985,#5760,.T.);
#13620=EDGE_CURVE('',#10982,#10953,#5761,.T.);
#13621=EDGE_CURVE('',#10952,#10983,#5762,.T.);
#13622=EDGE_CURVE('',#10984,#10955,#5763,.T.);
#13623=EDGE_CURVE('',#10986,#10986,#9584,.T.);
#13624=EDGE_CURVE('',#10986,#10987,#5764,.T.);
#13625=EDGE_CURVE('',#10988,#10987,#845,.T.);
#13626=EDGE_CURVE('',#10989,#10988,#846,.T.);
#13627=EDGE_CURVE('',#10987,#10989,#847,.T.);
#13628=EDGE_CURVE('',#10956,#10987,#5765,.T.);
#13629=EDGE_CURVE('',#10988,#10980,#5766,.T.);
#13630=EDGE_CURVE('',#10990,#10991,#848,.F.);
#13631=EDGE_CURVE('',#10991,#10992,#9585,.T.);
#13632=EDGE_CURVE('',#10992,#10993,#5767,.T.);
#13633=EDGE_CURVE('',#10993,#10994,#9586,.T.);
#13634=EDGE_CURVE('',#10994,#10995,#5768,.T.);
#13635=EDGE_CURVE('',#10995,#10996,#9587,.T.);
#13636=EDGE_CURVE('',#10996,#10997,#5769,.T.);
#13637=EDGE_CURVE('',#10997,#10998,#9588,.T.);
#13638=EDGE_CURVE('',#10998,#10990,#5770,.T.);
#13639=EDGE_CURVE('',#10999,#11000,#9589,.T.);
#13640=EDGE_CURVE('',#11000,#11001,#5771,.T.);
#13641=EDGE_CURVE('',#11001,#11002,#9590,.T.);
#13642=EDGE_CURVE('',#11002,#11003,#5772,.T.);
#13643=EDGE_CURVE('',#11003,#11004,#9591,.T.);
#13644=EDGE_CURVE('',#11004,#11005,#5773,.T.);
#13645=EDGE_CURVE('',#11005,#11006,#9592,.T.);
#13646=EDGE_CURVE('',#11006,#10999,#5774,.T.);
#13647=EDGE_CURVE('',#11007,#11008,#5775,.T.);
#13648=EDGE_CURVE('',#11008,#11009,#66,.T.);
#13649=EDGE_CURVE('',#11009,#11010,#67,.T.);
#13650=EDGE_CURVE('',#11010,#11011,#5776,.T.);
#13651=EDGE_CURVE('',#11011,#11012,#68,.T.);
#13652=EDGE_CURVE('',#11012,#11007,#69,.T.);
#13653=EDGE_CURVE('',#11013,#11014,#70,.F.);
#13654=EDGE_CURVE('',#11014,#11015,#5777,.T.);
#13655=EDGE_CURVE('',#11015,#11016,#71,.T.);
#13656=EDGE_CURVE('',#11016,#11017,#9593,.T.);
#13657=EDGE_CURVE('',#11017,#11018,#5778,.T.);
#13658=EDGE_CURVE('',#11018,#11019,#9594,.T.);
#13659=EDGE_CURVE('',#11019,#11020,#5779,.T.);
#13660=EDGE_CURVE('',#11020,#11021,#9595,.T.);
#13661=EDGE_CURVE('',#11021,#11022,#72,.T.);
#13662=EDGE_CURVE('',#11022,#11023,#5780,.T.);
#13663=EDGE_CURVE('',#11023,#11013,#73,.T.);
#13664=EDGE_CURVE('',#11024,#11025,#74,.T.);
#13665=EDGE_CURVE('',#11025,#11026,#5781,.T.);
#13666=EDGE_CURVE('',#11026,#11027,#75,.T.);
#13667=EDGE_CURVE('',#11027,#11028,#76,.T.);
#13668=EDGE_CURVE('',#11028,#11029,#5782,.T.);
#13669=EDGE_CURVE('',#11029,#11024,#77,.T.);
#13670=EDGE_CURVE('',#11030,#11031,#9596,.T.);
#13671=EDGE_CURVE('',#11031,#11032,#5783,.T.);
#13672=EDGE_CURVE('',#11032,#11033,#9597,.T.);
#13673=EDGE_CURVE('',#11033,#11034,#5784,.T.);
#13674=EDGE_CURVE('',#11034,#11035,#9598,.T.);
#13675=EDGE_CURVE('',#11035,#11036,#5785,.T.);
#13676=EDGE_CURVE('',#11036,#11037,#9599,.T.);
#13677=EDGE_CURVE('',#11037,#11030,#5786,.T.);
#13678=EDGE_CURVE('',#11037,#11001,#5787,.T.);
#13679=EDGE_CURVE('',#11036,#11002,#5788,.T.);
#13680=EDGE_CURVE('',#11030,#11000,#5789,.T.);
#13681=EDGE_CURVE('',#11035,#11003,#5790,.T.);
#13682=EDGE_CURVE('',#11034,#11004,#5791,.T.);
#13683=EDGE_CURVE('',#11033,#11005,#5792,.T.);
#13684=EDGE_CURVE('',#11032,#11006,#5793,.T.);
#13685=EDGE_CURVE('',#11031,#10999,#5794,.T.);
#13686=EDGE_CURVE('',#11038,#11015,#5795,.T.);
#13687=EDGE_CURVE('',#11039,#11038,#78,.T.);
#13688=EDGE_CURVE('',#11039,#11016,#5796,.T.);
#13689=EDGE_CURVE('',#11040,#11014,#5797,.T.);
#13690=EDGE_CURVE('',#11038,#11040,#5798,.T.);
#13691=EDGE_CURVE('',#11041,#11013,#5799,.T.);
#13692=EDGE_CURVE('',#11040,#11041,#79,.F.);
#13693=EDGE_CURVE('',#11042,#11022,#5800,.T.);
#13694=EDGE_CURVE('',#11043,#11042,#5801,.T.);
#13695=EDGE_CURVE('',#11043,#11023,#5802,.T.);
#13696=EDGE_CURVE('',#11044,#11021,#5803,.T.);
#13697=EDGE_CURVE('',#11042,#11044,#80,.T.);
#13698=EDGE_CURVE('',#11045,#11020,#5804,.T.);
#13699=EDGE_CURVE('',#11044,#11045,#9600,.T.);
#13700=EDGE_CURVE('',#11046,#11019,#5805,.T.);
#13701=EDGE_CURVE('',#11045,#11046,#5806,.T.);
#13702=EDGE_CURVE('',#11047,#11018,#5807,.T.);
#13703=EDGE_CURVE('',#11046,#11047,#9601,.T.);
#13704=EDGE_CURVE('',#11048,#11017,#5808,.T.);
#13705=EDGE_CURVE('',#11047,#11048,#5809,.T.);
#13706=EDGE_CURVE('',#11048,#11039,#9602,.T.);
#13707=EDGE_CURVE('',#11041,#11043,#81,.T.);
#13708=EDGE_CURVE('',#11049,#11050,#82,.T.);
#13709=EDGE_CURVE('',#11050,#11051,#5810,.T.);
#13710=EDGE_CURVE('',#11051,#11052,#83,.T.);
#13711=EDGE_CURVE('',#11052,#11053,#84,.T.);
#13712=EDGE_CURVE('',#11053,#11054,#5811,.T.);
#13713=EDGE_CURVE('',#11054,#11049,#85,.T.);
#13714=EDGE_CURVE('',#11052,#11009,#5812,.T.);
#13715=EDGE_CURVE('',#11051,#11010,#5813,.T.);
#13716=EDGE_CURVE('',#11053,#11008,#5814,.T.);
#13717=EDGE_CURVE('',#11050,#11011,#5815,.T.);
#13718=EDGE_CURVE('',#11049,#11012,#5816,.T.);
#13719=EDGE_CURVE('',#11054,#11007,#5817,.T.);
#13720=EDGE_CURVE('',#11055,#11028,#5818,.T.);
#13721=EDGE_CURVE('',#11056,#11055,#5819,.T.);
#13722=EDGE_CURVE('',#11056,#11029,#5820,.T.);
#13723=EDGE_CURVE('',#11057,#11027,#5821,.T.);
#13724=EDGE_CURVE('',#11055,#11057,#86,.T.);
#13725=EDGE_CURVE('',#11058,#11026,#5822,.T.);
#13726=EDGE_CURVE('',#11057,#11058,#87,.T.);
#13727=EDGE_CURVE('',#11059,#11025,#5823,.T.);
#13728=EDGE_CURVE('',#11058,#11059,#5824,.T.);
#13729=EDGE_CURVE('',#11060,#11056,#88,.T.);
#13730=EDGE_CURVE('',#11060,#11024,#5825,.T.);
#13731=EDGE_CURVE('',#11059,#11060,#89,.T.);
#13732=EDGE_CURVE('',#11061,#10993,#5826,.T.);
#13733=EDGE_CURVE('',#11062,#11061,#9603,.T.);
#13734=EDGE_CURVE('',#11062,#10994,#5827,.T.);
#13735=EDGE_CURVE('',#11063,#10992,#5828,.T.);
#13736=EDGE_CURVE('',#11061,#11063,#5829,.T.);
#13737=EDGE_CURVE('',#11064,#10991,#5830,.T.);
#13738=EDGE_CURVE('',#11063,#11064,#9604,.T.);
#13739=EDGE_CURVE('',#11065,#10990,#5831,.T.);
#13740=EDGE_CURVE('',#11064,#11065,#849,.F.);
#13741=EDGE_CURVE('',#11066,#10998,#5832,.T.);
#13742=EDGE_CURVE('',#11065,#11066,#5833,.T.);
#13743=EDGE_CURVE('',#11067,#10960,#5834,.T.);
#13744=EDGE_CURVE('',#11068,#11067,#9605,.T.);
#13745=EDGE_CURVE('',#11068,#10957,#5835,.T.);
#13746=EDGE_CURVE('',#11069,#10959,#5836,.T.);
#13747=EDGE_CURVE('',#11067,#11069,#5837,.T.);
#13748=EDGE_CURVE('',#11070,#10997,#5838,.T.);
#13749=EDGE_CURVE('',#11066,#11070,#9606,.T.);
#13750=EDGE_CURVE('',#11071,#10996,#5839,.T.);
#13751=EDGE_CURVE('',#11070,#11071,#5840,.T.);
#13752=EDGE_CURVE('',#11072,#10995,#5841,.T.);
#13753=EDGE_CURVE('',#11071,#11072,#9607,.T.);
#13754=EDGE_CURVE('',#11072,#11062,#5842,.T.);
#13755=EDGE_CURVE('',#11073,#10958,#5843,.T.);
#13756=EDGE_CURVE('',#11069,#11073,#850,.T.);
#13757=EDGE_CURVE('',#11073,#11068,#5844,.T.);
#13758=EDGE_CURVE('',#11074,#11074,#9608,.T.);
#13759=EDGE_CURVE('',#11075,#11076,#5845,.T.);
#13760=EDGE_CURVE('',#11076,#11077,#5846,.T.);
#13761=EDGE_CURVE('',#11077,#11078,#5847,.T.);
#13762=EDGE_CURVE('',#11078,#11079,#5848,.T.);
#13763=EDGE_CURVE('',#11079,#11080,#5849,.T.);
#13764=EDGE_CURVE('',#11080,#11075,#5850,.T.);
#13765=EDGE_CURVE('',#11081,#11081,#9609,.T.);
#13766=EDGE_CURVE('',#11074,#11081,#5851,.T.);
#13767=EDGE_CURVE('',#11082,#11083,#5852,.T.);
#13768=EDGE_CURVE('',#11084,#11082,#5853,.T.);
#13769=EDGE_CURVE('',#11085,#11084,#5854,.T.);
#13770=EDGE_CURVE('',#11086,#11085,#5855,.T.);
#13771=EDGE_CURVE('',#11087,#11086,#5856,.T.);
#13772=EDGE_CURVE('',#11083,#11087,#5857,.T.);
#13773=EDGE_CURVE('',#11082,#11080,#5858,.T.);
#13774=EDGE_CURVE('',#11083,#11075,#5859,.T.);
#13775=EDGE_CURVE('',#11084,#11079,#5860,.T.);
#13776=EDGE_CURVE('',#11085,#11078,#5861,.T.);
#13777=EDGE_CURVE('',#11086,#11077,#5862,.T.);
#13778=EDGE_CURVE('',#11087,#11076,#5863,.T.);
#13779=EDGE_CURVE('',#11088,#11089,#9610,.T.);
#13780=EDGE_CURVE('',#11090,#11089,#9611,.T.);
#13781=EDGE_CURVE('',#11090,#11091,#9612,.T.);
#13782=EDGE_CURVE('',#11091,#11088,#9613,.T.);
#13783=EDGE_CURVE('',#11092,#11092,#9614,.T.);
#13784=EDGE_CURVE('',#11093,#11094,#5864,.T.);
#13785=EDGE_CURVE('',#11094,#11095,#5865,.T.);
#13786=EDGE_CURVE('',#11095,#11096,#5866,.T.);
#13787=EDGE_CURVE('',#11096,#11093,#9615,.T.);
#13788=EDGE_CURVE('',#11097,#11097,#9616,.T.);
#13789=EDGE_CURVE('',#11097,#11092,#5867,.T.);
#13790=EDGE_CURVE('',#11098,#11099,#5868,.T.);
#13791=EDGE_CURVE('',#11099,#11100,#851,.T.);
#13792=EDGE_CURVE('',#11100,#11101,#5869,.T.);
#13793=EDGE_CURVE('',#11101,#11098,#9617,.T.);
#13794=EDGE_CURVE('',#11102,#11103,#9618,.T.);
#13795=EDGE_CURVE('',#11104,#11103,#9619,.T.);
#13796=EDGE_CURVE('',#11104,#11105,#9620,.T.);
#13797=EDGE_CURVE('',#11105,#11102,#9621,.T.);
#13798=EDGE_CURVE('',#11106,#11107,#9622,.T.);
#13799=EDGE_CURVE('',#11107,#11108,#9623,.T.);
#13800=EDGE_CURVE('',#11108,#11109,#9624,.T.);
#13801=EDGE_CURVE('',#11106,#11109,#9625,.T.);
#13802=EDGE_CURVE('',#11110,#11111,#9626,.T.);
#13803=EDGE_CURVE('',#11089,#11111,#5870,.T.);
#13804=EDGE_CURVE('',#11110,#11088,#5871,.T.);
#13805=EDGE_CURVE('',#11107,#11112,#5872,.T.);
#13806=EDGE_CURVE('',#11112,#11113,#9627,.T.);
#13807=EDGE_CURVE('',#11113,#11108,#5873,.T.);
#13808=EDGE_CURVE('',#11105,#11114,#5874,.T.);
#13809=EDGE_CURVE('',#11114,#11115,#9628,.T.);
#13810=EDGE_CURVE('',#11115,#11102,#5875,.T.);
#13811=EDGE_CURVE('',#11091,#11116,#5876,.T.);
#13812=EDGE_CURVE('',#11116,#11110,#9629,.T.);
#13813=EDGE_CURVE('',#11117,#11104,#5877,.T.);
#13814=EDGE_CURVE('',#11117,#11114,#9630,.T.);
#13815=EDGE_CURVE('',#11113,#11118,#9631,.T.);
#13816=EDGE_CURVE('',#11109,#11118,#5878,.T.);
#13817=EDGE_CURVE('',#11111,#11119,#9632,.T.);
#13818=EDGE_CURVE('',#11120,#11116,#9633,.T.);
#13819=EDGE_CURVE('',#11121,#11120,#9634,.T.);
#13820=EDGE_CURVE('',#11122,#11121,#9635,.T.);
#13821=EDGE_CURVE('',#11115,#11122,#9636,.T.);
#13822=EDGE_CURVE('',#11118,#11117,#9637,.T.);
#13823=EDGE_CURVE('',#11119,#11112,#9638,.T.);
#13824=EDGE_CURVE('',#11123,#11124,#5879,.T.);
#13825=EDGE_CURVE('',#11124,#11125,#9639,.T.);
#13826=EDGE_CURVE('',#11125,#11126,#5880,.T.);
#13827=EDGE_CURVE('',#11126,#11123,#5881,.T.);
#13828=EDGE_CURVE('',#11120,#11090,#5882,.T.);
#13829=EDGE_CURVE('',#11103,#11122,#5883,.T.);
#13830=EDGE_CURVE('',#11119,#11106,#5884,.T.);
#13831=EDGE_CURVE('',#11127,#11124,#5885,.T.);
#13832=EDGE_CURVE('',#11128,#11127,#852,.T.);
#13833=EDGE_CURVE('',#11093,#11128,#5886,.T.);
#13834=EDGE_CURVE('',#11129,#11096,#5887,.T.);
#13835=EDGE_CURVE('',#11130,#11129,#853,.T.);
#13836=EDGE_CURVE('',#11125,#11130,#5888,.T.);
#13837=EDGE_CURVE('',#11131,#11130,#5889,.T.);
#13838=EDGE_CURVE('',#11131,#11126,#5890,.T.);
#13839=EDGE_CURVE('',#11129,#11132,#5891,.T.);
#13840=EDGE_CURVE('',#11095,#11132,#5892,.T.);
#13841=EDGE_CURVE('',#11133,#11131,#9640,.T.);
#13842=EDGE_CURVE('',#11123,#11133,#5893,.T.);
#13843=EDGE_CURVE('',#11132,#11134,#9641,.T.);
#13844=EDGE_CURVE('',#11135,#11094,#5894,.T.);
#13845=EDGE_CURVE('',#11134,#11135,#9642,.T.);
#13846=EDGE_CURVE('',#11127,#11133,#5895,.T.);
#13847=EDGE_CURVE('',#11135,#11128,#5896,.T.);
#13848=EDGE_CURVE('',#11134,#11136,#5897,.T.);
#13849=EDGE_CURVE('',#11137,#11136,#854,.T.);
#13850=EDGE_CURVE('',#11138,#11137,#855,.T.);
#13851=EDGE_CURVE('',#11136,#11138,#856,.T.);
#13852=EDGE_CURVE('',#11097,#11136,#5898,.T.);
#13853=EDGE_CURVE('',#11137,#11121,#5899,.T.);
#13854=EDGE_CURVE('',#11139,#11140,#857,.F.);
#13855=EDGE_CURVE('',#11140,#11141,#9643,.T.);
#13856=EDGE_CURVE('',#11141,#11142,#5900,.T.);
#13857=EDGE_CURVE('',#11142,#11143,#9644,.T.);
#13858=EDGE_CURVE('',#11143,#11144,#5901,.T.);
#13859=EDGE_CURVE('',#11144,#11145,#9645,.T.);
#13860=EDGE_CURVE('',#11145,#11146,#5902,.T.);
#13861=EDGE_CURVE('',#11146,#11147,#9646,.T.);
#13862=EDGE_CURVE('',#11147,#11139,#5903,.T.);
#13863=EDGE_CURVE('',#11148,#11149,#9647,.T.);
#13864=EDGE_CURVE('',#11149,#11150,#5904,.T.);
#13865=EDGE_CURVE('',#11150,#11151,#9648,.T.);
#13866=EDGE_CURVE('',#11151,#11152,#5905,.T.);
#13867=EDGE_CURVE('',#11152,#11153,#9649,.T.);
#13868=EDGE_CURVE('',#11153,#11154,#5906,.T.);
#13869=EDGE_CURVE('',#11154,#11155,#9650,.T.);
#13870=EDGE_CURVE('',#11155,#11148,#5907,.T.);
#13871=EDGE_CURVE('',#11156,#11157,#5908,.T.);
#13872=EDGE_CURVE('',#11157,#11158,#90,.T.);
#13873=EDGE_CURVE('',#11158,#11159,#91,.T.);
#13874=EDGE_CURVE('',#11159,#11160,#5909,.T.);
#13875=EDGE_CURVE('',#11160,#11161,#92,.T.);
#13876=EDGE_CURVE('',#11161,#11156,#93,.T.);
#13877=EDGE_CURVE('',#11162,#11163,#94,.F.);
#13878=EDGE_CURVE('',#11163,#11164,#5910,.T.);
#13879=EDGE_CURVE('',#11164,#11165,#95,.T.);
#13880=EDGE_CURVE('',#11165,#11166,#9651,.T.);
#13881=EDGE_CURVE('',#11166,#11167,#5911,.T.);
#13882=EDGE_CURVE('',#11167,#11168,#9652,.T.);
#13883=EDGE_CURVE('',#11168,#11169,#5912,.T.);
#13884=EDGE_CURVE('',#11169,#11170,#9653,.T.);
#13885=EDGE_CURVE('',#11170,#11171,#96,.T.);
#13886=EDGE_CURVE('',#11171,#11172,#5913,.T.);
#13887=EDGE_CURVE('',#11172,#11162,#97,.T.);
#13888=EDGE_CURVE('',#11173,#11174,#98,.T.);
#13889=EDGE_CURVE('',#11174,#11175,#5914,.T.);
#13890=EDGE_CURVE('',#11175,#11176,#99,.T.);
#13891=EDGE_CURVE('',#11176,#11177,#100,.T.);
#13892=EDGE_CURVE('',#11177,#11178,#5915,.T.);
#13893=EDGE_CURVE('',#11178,#11173,#101,.T.);
#13894=EDGE_CURVE('',#11179,#11180,#9654,.T.);
#13895=EDGE_CURVE('',#11180,#11181,#5916,.T.);
#13896=EDGE_CURVE('',#11181,#11182,#9655,.T.);
#13897=EDGE_CURVE('',#11182,#11183,#5917,.T.);
#13898=EDGE_CURVE('',#11183,#11184,#9656,.T.);
#13899=EDGE_CURVE('',#11184,#11185,#5918,.T.);
#13900=EDGE_CURVE('',#11185,#11186,#9657,.T.);
#13901=EDGE_CURVE('',#11186,#11179,#5919,.T.);
#13902=EDGE_CURVE('',#11186,#11150,#5920,.T.);
#13903=EDGE_CURVE('',#11185,#11151,#5921,.T.);
#13904=EDGE_CURVE('',#11179,#11149,#5922,.T.);
#13905=EDGE_CURVE('',#11184,#11152,#5923,.T.);
#13906=EDGE_CURVE('',#11183,#11153,#5924,.T.);
#13907=EDGE_CURVE('',#11182,#11154,#5925,.T.);
#13908=EDGE_CURVE('',#11181,#11155,#5926,.T.);
#13909=EDGE_CURVE('',#11180,#11148,#5927,.T.);
#13910=EDGE_CURVE('',#11187,#11164,#5928,.T.);
#13911=EDGE_CURVE('',#11188,#11187,#102,.T.);
#13912=EDGE_CURVE('',#11188,#11165,#5929,.T.);
#13913=EDGE_CURVE('',#11189,#11163,#5930,.T.);
#13914=EDGE_CURVE('',#11187,#11189,#5931,.T.);
#13915=EDGE_CURVE('',#11190,#11162,#5932,.T.);
#13916=EDGE_CURVE('',#11189,#11190,#103,.F.);
#13917=EDGE_CURVE('',#11191,#11171,#5933,.T.);
#13918=EDGE_CURVE('',#11192,#11191,#5934,.T.);
#13919=EDGE_CURVE('',#11192,#11172,#5935,.T.);
#13920=EDGE_CURVE('',#11193,#11170,#5936,.T.);
#13921=EDGE_CURVE('',#11191,#11193,#104,.T.);
#13922=EDGE_CURVE('',#11194,#11169,#5937,.T.);
#13923=EDGE_CURVE('',#11193,#11194,#9658,.T.);
#13924=EDGE_CURVE('',#11195,#11168,#5938,.T.);
#13925=EDGE_CURVE('',#11194,#11195,#5939,.T.);
#13926=EDGE_CURVE('',#11196,#11167,#5940,.T.);
#13927=EDGE_CURVE('',#11195,#11196,#9659,.T.);
#13928=EDGE_CURVE('',#11197,#11166,#5941,.T.);
#13929=EDGE_CURVE('',#11196,#11197,#5942,.T.);
#13930=EDGE_CURVE('',#11197,#11188,#9660,.T.);
#13931=EDGE_CURVE('',#11190,#11192,#105,.T.);
#13932=EDGE_CURVE('',#11198,#11199,#106,.T.);
#13933=EDGE_CURVE('',#11199,#11200,#5943,.T.);
#13934=EDGE_CURVE('',#11200,#11201,#107,.T.);
#13935=EDGE_CURVE('',#11201,#11202,#108,.T.);
#13936=EDGE_CURVE('',#11202,#11203,#5944,.T.);
#13937=EDGE_CURVE('',#11203,#11198,#109,.T.);
#13938=EDGE_CURVE('',#11201,#11158,#5945,.T.);
#13939=EDGE_CURVE('',#11200,#11159,#5946,.T.);
#13940=EDGE_CURVE('',#11202,#11157,#5947,.T.);
#13941=EDGE_CURVE('',#11199,#11160,#5948,.T.);
#13942=EDGE_CURVE('',#11198,#11161,#5949,.T.);
#13943=EDGE_CURVE('',#11203,#11156,#5950,.T.);
#13944=EDGE_CURVE('',#11204,#11177,#5951,.T.);
#13945=EDGE_CURVE('',#11205,#11204,#5952,.T.);
#13946=EDGE_CURVE('',#11205,#11178,#5953,.T.);
#13947=EDGE_CURVE('',#11206,#11176,#5954,.T.);
#13948=EDGE_CURVE('',#11204,#11206,#110,.T.);
#13949=EDGE_CURVE('',#11207,#11175,#5955,.T.);
#13950=EDGE_CURVE('',#11206,#11207,#111,.T.);
#13951=EDGE_CURVE('',#11208,#11174,#5956,.T.);
#13952=EDGE_CURVE('',#11207,#11208,#5957,.T.);
#13953=EDGE_CURVE('',#11209,#11205,#112,.T.);
#13954=EDGE_CURVE('',#11209,#11173,#5958,.T.);
#13955=EDGE_CURVE('',#11208,#11209,#113,.T.);
#13956=EDGE_CURVE('',#11210,#11142,#5959,.T.);
#13957=EDGE_CURVE('',#11211,#11210,#9661,.T.);
#13958=EDGE_CURVE('',#11211,#11143,#5960,.T.);
#13959=EDGE_CURVE('',#11212,#11141,#5961,.T.);
#13960=EDGE_CURVE('',#11210,#11212,#5962,.T.);
#13961=EDGE_CURVE('',#11213,#11140,#5963,.T.);
#13962=EDGE_CURVE('',#11212,#11213,#9662,.T.);
#13963=EDGE_CURVE('',#11214,#11139,#5964,.T.);
#13964=EDGE_CURVE('',#11213,#11214,#858,.F.);
#13965=EDGE_CURVE('',#11215,#11147,#5965,.T.);
#13966=EDGE_CURVE('',#11214,#11215,#5966,.T.);
#13967=EDGE_CURVE('',#11216,#11101,#5967,.T.);
#13968=EDGE_CURVE('',#11217,#11216,#9663,.T.);
#13969=EDGE_CURVE('',#11217,#11098,#5968,.T.);
#13970=EDGE_CURVE('',#11218,#11100,#5969,.T.);
#13971=EDGE_CURVE('',#11216,#11218,#5970,.T.);
#13972=EDGE_CURVE('',#11219,#11146,#5971,.T.);
#13973=EDGE_CURVE('',#11215,#11219,#9664,.T.);
#13974=EDGE_CURVE('',#11220,#11145,#5972,.T.);
#13975=EDGE_CURVE('',#11219,#11220,#5973,.T.);
#13976=EDGE_CURVE('',#11221,#11144,#5974,.T.);
#13977=EDGE_CURVE('',#11220,#11221,#9665,.T.);
#13978=EDGE_CURVE('',#11221,#11211,#5975,.T.);
#13979=EDGE_CURVE('',#11222,#11099,#5976,.T.);
#13980=EDGE_CURVE('',#11218,#11222,#859,.T.);
#13981=EDGE_CURVE('',#11222,#11217,#5977,.T.);
#13982=EDGE_CURVE('',#11223,#11223,#9666,.T.);
#13983=EDGE_CURVE('',#11223,#11224,#5978,.T.);
#13984=EDGE_CURVE('',#11224,#11224,#9667,.T.);
#13985=EDGE_CURVE('',#11225,#11225,#9668,.T.);
#13986=EDGE_CURVE('',#11225,#11226,#5979,.T.);
#13987=EDGE_CURVE('',#11226,#11226,#9669,.T.);
#13988=EDGE_CURVE('',#11227,#11227,#9670,.T.);
#13989=EDGE_CURVE('',#11227,#11228,#5980,.T.);
#13990=EDGE_CURVE('',#11228,#11228,#9671,.T.);
#13991=EDGE_CURVE('',#11229,#11229,#9672,.T.);
#13992=EDGE_CURVE('',#11229,#11230,#5981,.T.);
#13993=EDGE_CURVE('',#11230,#11230,#9673,.T.);
#13994=EDGE_CURVE('',#11231,#11231,#9674,.T.);
#13995=EDGE_CURVE('',#11231,#11232,#5982,.T.);
#13996=EDGE_CURVE('',#11232,#11232,#9675,.T.);
#13997=EDGE_CURVE('',#11233,#11233,#9676,.T.);
#13998=EDGE_CURVE('',#11233,#11234,#5983,.T.);
#13999=EDGE_CURVE('',#11234,#11234,#9677,.T.);
#14000=EDGE_CURVE('',#11235,#11235,#9678,.T.);
#14001=EDGE_CURVE('',#11235,#11236,#5984,.T.);
#14002=EDGE_CURVE('',#11236,#11236,#9679,.T.);
#14003=EDGE_CURVE('',#11237,#11238,#5985,.T.);
#14004=EDGE_CURVE('',#11237,#11239,#9680,.T.);
#14005=EDGE_CURVE('',#11240,#11239,#5986,.T.);
#14006=EDGE_CURVE('',#11240,#11241,#5987,.T.);
#14007=EDGE_CURVE('',#11241,#11242,#5988,.T.);
#14008=EDGE_CURVE('',#11242,#11238,#9681,.T.);
#14009=EDGE_CURVE('',#11243,#11244,#5989,.T.);
#14010=EDGE_CURVE('',#11243,#11237,#5990,.T.);
#14011=EDGE_CURVE('',#11238,#11244,#5991,.T.);
#14012=EDGE_CURVE('',#11245,#11246,#5992,.T.);
#14013=EDGE_CURVE('',#11245,#11243,#9682,.T.);
#14014=EDGE_CURVE('',#11244,#11247,#9683,.T.);
#14015=EDGE_CURVE('',#11247,#11248,#5993,.T.);
#14016=EDGE_CURVE('',#11246,#11248,#5994,.T.);
#14017=EDGE_CURVE('',#11248,#11241,#5995,.T.);
#14018=EDGE_CURVE('',#11246,#11240,#5996,.T.);
#14019=EDGE_CURVE('',#11239,#11245,#5997,.T.);
#14020=EDGE_CURVE('',#11247,#11242,#5998,.T.);
#14021=EDGE_CURVE('',#11249,#11249,#9684,.T.);
#14022=EDGE_CURVE('',#11249,#11250,#5999,.T.);
#14023=EDGE_CURVE('',#11250,#11250,#9685,.T.);
#14024=EDGE_CURVE('',#11251,#11251,#9686,.T.);
#14025=EDGE_CURVE('',#11251,#11252,#6000,.T.);
#14026=EDGE_CURVE('',#11252,#11252,#9687,.T.);
#14027=EDGE_CURVE('',#11253,#11253,#9688,.T.);
#14028=EDGE_CURVE('',#11253,#11254,#6001,.T.);
#14029=EDGE_CURVE('',#11254,#11254,#9689,.T.);
#14030=EDGE_CURVE('',#11255,#11255,#9690,.T.);
#14031=EDGE_CURVE('',#11255,#11256,#6002,.T.);
#14032=EDGE_CURVE('',#11256,#11256,#9691,.T.);
#14033=EDGE_CURVE('',#11257,#11257,#9692,.T.);
#14034=EDGE_CURVE('',#11257,#11258,#6003,.T.);
#14035=EDGE_CURVE('',#11258,#11258,#9693,.T.);
#14036=EDGE_CURVE('',#11259,#11259,#9694,.T.);
#14037=EDGE_CURVE('',#11259,#11260,#6004,.T.);
#14038=EDGE_CURVE('',#11260,#11260,#9695,.T.);
#14039=EDGE_CURVE('',#11261,#11262,#6005,.T.);
#14040=EDGE_CURVE('',#11263,#11262,#6006,.T.);
#14041=EDGE_CURVE('',#11264,#11263,#6007,.T.);
#14042=EDGE_CURVE('',#11264,#11261,#6008,.T.);
#14043=EDGE_CURVE('',#11262,#11265,#6009,.T.);
#14044=EDGE_CURVE('',#11266,#11265,#6010,.T.);
#14045=EDGE_CURVE('',#11263,#11266,#6011,.T.);
#14046=EDGE_CURVE('',#11265,#11267,#6012,.T.);
#14047=EDGE_CURVE('',#11268,#11267,#6013,.T.);
#14048=EDGE_CURVE('',#11266,#11268,#6014,.T.);
#14049=EDGE_CURVE('',#11267,#11261,#6015,.T.);
#14050=EDGE_CURVE('',#11268,#11264,#6016,.T.);
#14051=EDGE_CURVE('',#11269,#11269,#9696,.T.);
#14052=EDGE_CURVE('',#11269,#11270,#6017,.T.);
#14053=EDGE_CURVE('',#11270,#11270,#9697,.T.);
#14054=EDGE_CURVE('',#11271,#11271,#9698,.T.);
#14055=EDGE_CURVE('',#11271,#11272,#6018,.T.);
#14056=EDGE_CURVE('',#11272,#11272,#9699,.T.);
#14057=EDGE_CURVE('',#11273,#11273,#9700,.T.);
#14058=EDGE_CURVE('',#11273,#11274,#6019,.T.);
#14059=EDGE_CURVE('',#11274,#11274,#9701,.T.);
#14060=EDGE_CURVE('',#11275,#11275,#9702,.T.);
#14061=EDGE_CURVE('',#11275,#11276,#6020,.T.);
#14062=EDGE_CURVE('',#11276,#11276,#9703,.T.);
#14063=EDGE_CURVE('',#11277,#11277,#9704,.T.);
#14064=EDGE_CURVE('',#11277,#11278,#6021,.T.);
#14065=EDGE_CURVE('',#11278,#11278,#9705,.T.);
#14066=EDGE_CURVE('',#11279,#11279,#9706,.T.);
#14067=EDGE_CURVE('',#11279,#11280,#6022,.T.);
#14068=EDGE_CURVE('',#11280,#11280,#9707,.T.);
#14069=EDGE_CURVE('',#11281,#11282,#6023,.T.);
#14070=EDGE_CURVE('',#11283,#11282,#6024,.T.);
#14071=EDGE_CURVE('',#11284,#11283,#6025,.T.);
#14072=EDGE_CURVE('',#11284,#11281,#6026,.T.);
#14073=EDGE_CURVE('',#11282,#11285,#6027,.T.);
#14074=EDGE_CURVE('',#11286,#11285,#6028,.T.);
#14075=EDGE_CURVE('',#11283,#11286,#6029,.T.);
#14076=EDGE_CURVE('',#11285,#11287,#6030,.T.);
#14077=EDGE_CURVE('',#11288,#11287,#6031,.T.);
#14078=EDGE_CURVE('',#11286,#11288,#6032,.T.);
#14079=EDGE_CURVE('',#11287,#11281,#6033,.T.);
#14080=EDGE_CURVE('',#11288,#11284,#6034,.T.);
#14081=EDGE_CURVE('',#11289,#11290,#6035,.T.);
#14082=EDGE_CURVE('',#11291,#11289,#6036,.T.);
#14083=EDGE_CURVE('',#11291,#11292,#6037,.T.);
#14084=EDGE_CURVE('',#11292,#11290,#6038,.T.);
#14085=EDGE_CURVE('',#11293,#11289,#6039,.T.);
#14086=EDGE_CURVE('',#11294,#11293,#6040,.T.);
#14087=EDGE_CURVE('',#11294,#11291,#6041,.T.);
#14088=EDGE_CURVE('',#11295,#11293,#6042,.T.);
#14089=EDGE_CURVE('',#11296,#11295,#6043,.T.);
#14090=EDGE_CURVE('',#11296,#11294,#6044,.T.);
#14091=EDGE_CURVE('',#11295,#11297,#6045,.T.);
#14092=EDGE_CURVE('',#11298,#11297,#6046,.T.);
#14093=EDGE_CURVE('',#11296,#11298,#6047,.T.);
#14094=EDGE_CURVE('',#11297,#11290,#6048,.T.);
#14095=EDGE_CURVE('',#11298,#11292,#6049,.T.);
#14096=EDGE_CURVE('',#11299,#11300,#6050,.T.);
#14097=EDGE_CURVE('',#11301,#11300,#6051,.T.);
#14098=EDGE_CURVE('',#11302,#11301,#6052,.T.);
#14099=EDGE_CURVE('',#11302,#11299,#6053,.T.);
#14100=EDGE_CURVE('',#11303,#11299,#6054,.T.);
#14101=EDGE_CURVE('',#11304,#11302,#6055,.T.);
#14102=EDGE_CURVE('',#11304,#11303,#6056,.T.);
#14103=EDGE_CURVE('',#11305,#11303,#6057,.T.);
#14104=EDGE_CURVE('',#11306,#11304,#6058,.T.);
#14105=EDGE_CURVE('',#11306,#11305,#6059,.T.);
#14106=EDGE_CURVE('',#11305,#11307,#6060,.T.);
#14107=EDGE_CURVE('',#11306,#11308,#6061,.T.);
#14108=EDGE_CURVE('',#11308,#11307,#6062,.T.);
#14109=EDGE_CURVE('',#11307,#11300,#6063,.T.);
#14110=EDGE_CURVE('',#11308,#11301,#6064,.T.);
#14111=EDGE_CURVE('',#11309,#11310,#9708,.T.);
#14112=EDGE_CURVE('',#11310,#11311,#6065,.T.);
#14113=EDGE_CURVE('',#11311,#11312,#9709,.T.);
#14114=EDGE_CURVE('',#11309,#11312,#6066,.T.);
#14115=EDGE_CURVE('',#11313,#11313,#9710,.T.);
#14116=EDGE_CURVE('',#11313,#11314,#6067,.T.);
#14117=EDGE_CURVE('',#11314,#11314,#9711,.T.);
#14118=EDGE_CURVE('',#11315,#11315,#9712,.T.);
#14119=EDGE_CURVE('',#11315,#11316,#6068,.T.);
#14120=EDGE_CURVE('',#11316,#11316,#9713,.T.);
#14121=EDGE_CURVE('',#11317,#11317,#9714,.T.);
#14122=EDGE_CURVE('',#11317,#11318,#6069,.T.);
#14123=EDGE_CURVE('',#11318,#11318,#9715,.T.);
#14124=EDGE_CURVE('',#11319,#11319,#9716,.T.);
#14125=EDGE_CURVE('',#11319,#11320,#6070,.T.);
#14126=EDGE_CURVE('',#11320,#11320,#9717,.T.);
#14127=EDGE_CURVE('',#11321,#11321,#9718,.T.);
#14128=EDGE_CURVE('',#11321,#11322,#6071,.T.);
#14129=EDGE_CURVE('',#11322,#11322,#9719,.T.);
#14130=EDGE_CURVE('',#11323,#11323,#9720,.T.);
#14131=EDGE_CURVE('',#11323,#11324,#6072,.T.);
#14132=EDGE_CURVE('',#11324,#11324,#9721,.T.);
#14133=EDGE_CURVE('',#11325,#11325,#9722,.T.);
#14134=EDGE_CURVE('',#11325,#11326,#6073,.T.);
#14135=EDGE_CURVE('',#11326,#11326,#9723,.T.);
#14136=EDGE_CURVE('',#11327,#11327,#9724,.T.);
#14137=EDGE_CURVE('',#11327,#11328,#6074,.T.);
#14138=EDGE_CURVE('',#11328,#11328,#9725,.T.);
#14139=EDGE_CURVE('',#11329,#11329,#9726,.T.);
#14140=EDGE_CURVE('',#11329,#11330,#6075,.T.);
#14141=EDGE_CURVE('',#11330,#11330,#9727,.T.);
#14142=EDGE_CURVE('',#11331,#11331,#9728,.T.);
#14143=EDGE_CURVE('',#11331,#11332,#6076,.T.);
#14144=EDGE_CURVE('',#11332,#11332,#9729,.T.);
#14145=EDGE_CURVE('',#11333,#11333,#9730,.T.);
#14146=EDGE_CURVE('',#11333,#11334,#6077,.T.);
#14147=EDGE_CURVE('',#11334,#11334,#9731,.T.);
#14148=EDGE_CURVE('',#11335,#11335,#9732,.T.);
#14149=EDGE_CURVE('',#11335,#11336,#6078,.T.);
#14150=EDGE_CURVE('',#11336,#11336,#9733,.T.);
#14151=EDGE_CURVE('',#11337,#11337,#9734,.T.);
#14152=EDGE_CURVE('',#11337,#11338,#6079,.T.);
#14153=EDGE_CURVE('',#11338,#11338,#9735,.T.);
#14154=EDGE_CURVE('',#11339,#11339,#9736,.T.);
#14155=EDGE_CURVE('',#11339,#11340,#6080,.T.);
#14156=EDGE_CURVE('',#11340,#11340,#9737,.T.);
#14157=EDGE_CURVE('',#11341,#11341,#9738,.T.);
#14158=EDGE_CURVE('',#11341,#11342,#6081,.T.);
#14159=EDGE_CURVE('',#11342,#11342,#9739,.T.);
#14160=EDGE_CURVE('',#11343,#11343,#9740,.T.);
#14161=EDGE_CURVE('',#11343,#11344,#6082,.T.);
#14162=EDGE_CURVE('',#11344,#11344,#9741,.T.);
#14163=EDGE_CURVE('',#11345,#11345,#9742,.T.);
#14164=EDGE_CURVE('',#11345,#11346,#6083,.T.);
#14165=EDGE_CURVE('',#11346,#11346,#9743,.T.);
#14166=EDGE_CURVE('',#11347,#11347,#9744,.T.);
#14167=EDGE_CURVE('',#11347,#11348,#6084,.T.);
#14168=EDGE_CURVE('',#11348,#11348,#9745,.T.);
#14169=EDGE_CURVE('',#11349,#11349,#9746,.T.);
#14170=EDGE_CURVE('',#11349,#11350,#6085,.T.);
#14171=EDGE_CURVE('',#11350,#11350,#9747,.T.);
#14172=EDGE_CURVE('',#11351,#11351,#9748,.T.);
#14173=EDGE_CURVE('',#11351,#11352,#6086,.T.);
#14174=EDGE_CURVE('',#11352,#11352,#9749,.T.);
#14175=EDGE_CURVE('',#11353,#11353,#9750,.T.);
#14176=EDGE_CURVE('',#11353,#11354,#6087,.T.);
#14177=EDGE_CURVE('',#11354,#11354,#9751,.T.);
#14178=EDGE_CURVE('',#11355,#11355,#9752,.T.);
#14179=EDGE_CURVE('',#11355,#11356,#6088,.T.);
#14180=EDGE_CURVE('',#11356,#11356,#9753,.T.);
#14181=EDGE_CURVE('',#11357,#11357,#9754,.T.);
#14182=EDGE_CURVE('',#11357,#11358,#6089,.T.);
#14183=EDGE_CURVE('',#11358,#11358,#9755,.T.);
#14184=EDGE_CURVE('',#11359,#11359,#9756,.T.);
#14185=EDGE_CURVE('',#11359,#11360,#6090,.T.);
#14186=EDGE_CURVE('',#11360,#11360,#9757,.T.);
#14187=EDGE_CURVE('',#11361,#11361,#9758,.T.);
#14188=EDGE_CURVE('',#11361,#11362,#6091,.T.);
#14189=EDGE_CURVE('',#11362,#11362,#9759,.T.);
#14190=EDGE_CURVE('',#11363,#11363,#9760,.T.);
#14191=EDGE_CURVE('',#11363,#11364,#6092,.T.);
#14192=EDGE_CURVE('',#11364,#11364,#9761,.T.);
#14193=EDGE_CURVE('',#11365,#11365,#9762,.T.);
#14194=EDGE_CURVE('',#11365,#11366,#6093,.T.);
#14195=EDGE_CURVE('',#11366,#11366,#9763,.T.);
#14196=EDGE_CURVE('',#11367,#11367,#9764,.T.);
#14197=EDGE_CURVE('',#11367,#11368,#6094,.T.);
#14198=EDGE_CURVE('',#11368,#11368,#9765,.T.);
#14199=EDGE_CURVE('',#11369,#11369,#9766,.T.);
#14200=EDGE_CURVE('',#11369,#11370,#6095,.T.);
#14201=EDGE_CURVE('',#11370,#11370,#9767,.T.);
#14202=EDGE_CURVE('',#11371,#11371,#9768,.T.);
#14203=EDGE_CURVE('',#11371,#11372,#6096,.T.);
#14204=EDGE_CURVE('',#11372,#11372,#9769,.T.);
#14205=EDGE_CURVE('',#11373,#11373,#9770,.T.);
#14206=EDGE_CURVE('',#11373,#11374,#6097,.T.);
#14207=EDGE_CURVE('',#11374,#11374,#9771,.T.);
#14208=EDGE_CURVE('',#11375,#11375,#9772,.T.);
#14209=EDGE_CURVE('',#11375,#11376,#6098,.T.);
#14210=EDGE_CURVE('',#11376,#11376,#9773,.T.);
#14211=EDGE_CURVE('',#11377,#11377,#9774,.T.);
#14212=EDGE_CURVE('',#11377,#11378,#6099,.T.);
#14213=EDGE_CURVE('',#11378,#11378,#9775,.T.);
#14214=EDGE_CURVE('',#11379,#11379,#9776,.T.);
#14215=EDGE_CURVE('',#11379,#11380,#6100,.T.);
#14216=EDGE_CURVE('',#11380,#11380,#9777,.T.);
#14217=EDGE_CURVE('',#11381,#11381,#9778,.T.);
#14218=EDGE_CURVE('',#11381,#11382,#6101,.T.);
#14219=EDGE_CURVE('',#11382,#11382,#9779,.T.);
#14220=EDGE_CURVE('',#11383,#11383,#9780,.T.);
#14221=EDGE_CURVE('',#11383,#11384,#6102,.T.);
#14222=EDGE_CURVE('',#11384,#11384,#9781,.T.);
#14223=EDGE_CURVE('',#11385,#11385,#9782,.T.);
#14224=EDGE_CURVE('',#11385,#11386,#6103,.T.);
#14225=EDGE_CURVE('',#11386,#11386,#9783,.T.);
#14226=EDGE_CURVE('',#11387,#11387,#9784,.T.);
#14227=EDGE_CURVE('',#11387,#11388,#6104,.T.);
#14228=EDGE_CURVE('',#11388,#11388,#9785,.T.);
#14229=EDGE_CURVE('',#11389,#11389,#9786,.T.);
#14230=EDGE_CURVE('',#11389,#11390,#6105,.T.);
#14231=EDGE_CURVE('',#11390,#11390,#9787,.T.);
#14232=EDGE_CURVE('',#11391,#11391,#9788,.T.);
#14233=EDGE_CURVE('',#11391,#11392,#6106,.T.);
#14234=EDGE_CURVE('',#11392,#11392,#9789,.T.);
#14235=EDGE_CURVE('',#11393,#11393,#9790,.T.);
#14236=EDGE_CURVE('',#11393,#11394,#6107,.T.);
#14237=EDGE_CURVE('',#11394,#11394,#9791,.T.);
#14238=EDGE_CURVE('',#11395,#11395,#9792,.T.);
#14239=EDGE_CURVE('',#11395,#11396,#6108,.T.);
#14240=EDGE_CURVE('',#11396,#11396,#9793,.T.);
#14241=EDGE_CURVE('',#11397,#11397,#9794,.T.);
#14242=EDGE_CURVE('',#11397,#11398,#6109,.T.);
#14243=EDGE_CURVE('',#11398,#11398,#9795,.T.);
#14244=EDGE_CURVE('',#11399,#11399,#9796,.T.);
#14245=EDGE_CURVE('',#11399,#11400,#6110,.T.);
#14246=EDGE_CURVE('',#11400,#11400,#9797,.T.);
#14247=EDGE_CURVE('',#11401,#11401,#9798,.T.);
#14248=EDGE_CURVE('',#11401,#11402,#6111,.T.);
#14249=EDGE_CURVE('',#11402,#11402,#9799,.T.);
#14250=EDGE_CURVE('',#11403,#11403,#9800,.T.);
#14251=EDGE_CURVE('',#11403,#11404,#6112,.T.);
#14252=EDGE_CURVE('',#11404,#11404,#9801,.T.);
#14253=EDGE_CURVE('',#11405,#11405,#9802,.T.);
#14254=EDGE_CURVE('',#11405,#11406,#6113,.T.);
#14255=EDGE_CURVE('',#11406,#11406,#9803,.T.);
#14256=EDGE_CURVE('',#11407,#11407,#9804,.T.);
#14257=EDGE_CURVE('',#11407,#11408,#6114,.T.);
#14258=EDGE_CURVE('',#11408,#11408,#9805,.T.);
#14259=EDGE_CURVE('',#11409,#11410,#6115,.T.);
#14260=EDGE_CURVE('',#11409,#11411,#6116,.T.);
#14261=EDGE_CURVE('',#11412,#11411,#6117,.T.);
#14262=EDGE_CURVE('',#11412,#11413,#6118,.T.);
#14263=EDGE_CURVE('',#11414,#11413,#6119,.T.);
#14264=EDGE_CURVE('',#11414,#11415,#6120,.T.);
#14265=EDGE_CURVE('',#11416,#11415,#6121,.T.);
#14266=EDGE_CURVE('',#11416,#11410,#6122,.T.);
#14267=EDGE_CURVE('',#11417,#11418,#6123,.T.);
#14268=EDGE_CURVE('',#11418,#11419,#6124,.T.);
#14269=EDGE_CURVE('',#11420,#11419,#6125,.T.);
#14270=EDGE_CURVE('',#11420,#11417,#6126,.T.);
#14271=EDGE_CURVE('',#11421,#11422,#6127,.T.);
#14272=EDGE_CURVE('',#11421,#11423,#6128,.T.);
#14273=EDGE_CURVE('',#11423,#11424,#6129,.T.);
#14274=EDGE_CURVE('',#11424,#11422,#6130,.T.);
#14275=EDGE_CURVE('',#11425,#11426,#6131,.T.);
#14276=EDGE_CURVE('',#11426,#11427,#6132,.T.);
#14277=EDGE_CURVE('',#11428,#11427,#6133,.T.);
#14278=EDGE_CURVE('',#11425,#11428,#6134,.T.);
#14279=EDGE_CURVE('',#11419,#11421,#6135,.T.);
#14280=EDGE_CURVE('',#11422,#11426,#6136,.T.);
#14281=EDGE_CURVE('',#11425,#11420,#6137,.T.);
#14282=EDGE_CURVE('',#11310,#11429,#6138,.T.);
#14283=EDGE_CURVE('',#11430,#11309,#6139,.T.);
#14284=EDGE_CURVE('',#11429,#11430,#9806,.T.);
#14285=EDGE_CURVE('',#11423,#11418,#6140,.T.);
#14286=EDGE_CURVE('',#11428,#11417,#6141,.T.);
#14287=EDGE_CURVE('',#11427,#11424,#6142,.T.);
#14288=EDGE_CURVE('',#11431,#11311,#6143,.T.);
#14289=EDGE_CURVE('',#11432,#11431,#9807,.T.);
#14290=EDGE_CURVE('',#11312,#11432,#6144,.T.);
#14291=EDGE_CURVE('',#11433,#11434,#6145,.T.);
#14292=EDGE_CURVE('',#11434,#11435,#6146,.T.);
#14293=EDGE_CURVE('',#11435,#11436,#6147,.T.);
#14294=EDGE_CURVE('',#11436,#11437,#6148,.T.);
#14295=EDGE_CURVE('',#11437,#11438,#6149,.T.);
#14296=EDGE_CURVE('',#11438,#11439,#6150,.T.);
#14297=EDGE_CURVE('',#11439,#11440,#6151,.T.);
#14298=EDGE_CURVE('',#11440,#11433,#6152,.T.);
#14299=EDGE_CURVE('',#11435,#11409,#6153,.T.);
#14300=EDGE_CURVE('',#11410,#11436,#6154,.T.);
#14301=EDGE_CURVE('',#11415,#11438,#6155,.T.);
#14302=EDGE_CURVE('',#11437,#11416,#6156,.T.);
#14303=EDGE_CURVE('',#11413,#11440,#6157,.T.);
#14304=EDGE_CURVE('',#11439,#11414,#6158,.T.);
#14305=EDGE_CURVE('',#11411,#11434,#6159,.T.);
#14306=EDGE_CURVE('',#11433,#11412,#6160,.T.);
#14307=EDGE_CURVE('',#11429,#11431,#6161,.T.);
#14308=EDGE_CURVE('',#11430,#11432,#6162,.T.);
#14309=EDGE_CURVE('',#11441,#11441,#9808,.T.);
#14310=EDGE_CURVE('',#11441,#11442,#6163,.T.);
#14311=EDGE_CURVE('',#11442,#11442,#9809,.T.);
#14312=EDGE_CURVE('',#11443,#11444,#9810,.T.);
#14313=EDGE_CURVE('',#11445,#11443,#114,.T.);
#14314=EDGE_CURVE('',#11446,#11445,#9811,.T.);
#14315=EDGE_CURVE('',#11447,#11446,#115,.T.);
#14316=EDGE_CURVE('',#11448,#11447,#9812,.T.);
#14317=EDGE_CURVE('',#11448,#11449,#6164,.T.);
#14318=EDGE_CURVE('',#11449,#11449,#9813,.T.);
#14319=EDGE_CURVE('',#11450,#11448,#9814,.T.);
#14320=EDGE_CURVE('',#11451,#11450,#116,.T.);
#14321=EDGE_CURVE('',#11452,#11451,#9815,.T.);
#14322=EDGE_CURVE('',#11444,#11452,#117,.T.);
#14323=EDGE_CURVE('',#11453,#11453,#9816,.T.);
#14324=EDGE_CURVE('',#11453,#11454,#6165,.T.);
#14325=EDGE_CURVE('',#11454,#11454,#9817,.T.);
#14326=EDGE_CURVE('',#11455,#11456,#9818,.T.);
#14327=EDGE_CURVE('',#11457,#11455,#118,.T.);
#14328=EDGE_CURVE('',#11458,#11457,#9819,.T.);
#14329=EDGE_CURVE('',#11459,#11458,#119,.T.);
#14330=EDGE_CURVE('',#11460,#11459,#9820,.T.);
#14331=EDGE_CURVE('',#11460,#11461,#6166,.T.);
#14332=EDGE_CURVE('',#11461,#11461,#9821,.T.);
#14333=EDGE_CURVE('',#11462,#11460,#9822,.T.);
#14334=EDGE_CURVE('',#11463,#11462,#120,.T.);
#14335=EDGE_CURVE('',#11464,#11463,#9823,.T.);
#14336=EDGE_CURVE('',#11456,#11464,#121,.T.);
#14337=EDGE_CURVE('',#11465,#11465,#9824,.T.);
#14338=EDGE_CURVE('',#11465,#11466,#6167,.T.);
#14339=EDGE_CURVE('',#11466,#11466,#9825,.T.);
#14340=EDGE_CURVE('',#11467,#11468,#9826,.T.);
#14341=EDGE_CURVE('',#11469,#11467,#122,.T.);
#14342=EDGE_CURVE('',#11470,#11469,#9827,.T.);
#14343=EDGE_CURVE('',#11471,#11470,#123,.T.);
#14344=EDGE_CURVE('',#11472,#11471,#9828,.T.);
#14345=EDGE_CURVE('',#11472,#11473,#6168,.T.);
#14346=EDGE_CURVE('',#11473,#11473,#9829,.T.);
#14347=EDGE_CURVE('',#11474,#11472,#9830,.T.);
#14348=EDGE_CURVE('',#11475,#11474,#124,.T.);
#14349=EDGE_CURVE('',#11476,#11475,#9831,.T.);
#14350=EDGE_CURVE('',#11468,#11476,#125,.T.);
#14351=EDGE_CURVE('',#11477,#11477,#9832,.T.);
#14352=EDGE_CURVE('',#11477,#11478,#6169,.T.);
#14353=EDGE_CURVE('',#11478,#11478,#9833,.T.);
#14354=EDGE_CURVE('',#11479,#11480,#9834,.T.);
#14355=EDGE_CURVE('',#11481,#11479,#126,.T.);
#14356=EDGE_CURVE('',#11482,#11481,#9835,.T.);
#14357=EDGE_CURVE('',#11483,#11482,#127,.T.);
#14358=EDGE_CURVE('',#11484,#11483,#9836,.T.);
#14359=EDGE_CURVE('',#11484,#11485,#6170,.T.);
#14360=EDGE_CURVE('',#11485,#11485,#9837,.T.);
#14361=EDGE_CURVE('',#11486,#11484,#9838,.T.);
#14362=EDGE_CURVE('',#11487,#11486,#128,.T.);
#14363=EDGE_CURVE('',#11488,#11487,#9839,.T.);
#14364=EDGE_CURVE('',#11480,#11488,#129,.T.);
#14365=EDGE_CURVE('',#11489,#11489,#9840,.T.);
#14366=EDGE_CURVE('',#11489,#11490,#6171,.T.);
#14367=EDGE_CURVE('',#11490,#11490,#9841,.T.);
#14368=EDGE_CURVE('',#11491,#11492,#9842,.T.);
#14369=EDGE_CURVE('',#11493,#11491,#130,.T.);
#14370=EDGE_CURVE('',#11494,#11493,#9843,.T.);
#14371=EDGE_CURVE('',#11495,#11494,#131,.T.);
#14372=EDGE_CURVE('',#11496,#11495,#9844,.T.);
#14373=EDGE_CURVE('',#11496,#11497,#6172,.T.);
#14374=EDGE_CURVE('',#11497,#11497,#9845,.T.);
#14375=EDGE_CURVE('',#11498,#11496,#9846,.T.);
#14376=EDGE_CURVE('',#11499,#11498,#132,.T.);
#14377=EDGE_CURVE('',#11500,#11499,#9847,.T.);
#14378=EDGE_CURVE('',#11492,#11500,#133,.T.);
#14379=EDGE_CURVE('',#11501,#11501,#9848,.T.);
#14380=EDGE_CURVE('',#11501,#11502,#6173,.T.);
#14381=EDGE_CURVE('',#11502,#11502,#9849,.T.);
#14382=EDGE_CURVE('',#11503,#11504,#9850,.T.);
#14383=EDGE_CURVE('',#11505,#11503,#134,.T.);
#14384=EDGE_CURVE('',#11506,#11505,#9851,.T.);
#14385=EDGE_CURVE('',#11507,#11506,#135,.T.);
#14386=EDGE_CURVE('',#11508,#11507,#9852,.T.);
#14387=EDGE_CURVE('',#11508,#11509,#6174,.T.);
#14388=EDGE_CURVE('',#11509,#11509,#9853,.T.);
#14389=EDGE_CURVE('',#11510,#11508,#9854,.T.);
#14390=EDGE_CURVE('',#11511,#11510,#136,.T.);
#14391=EDGE_CURVE('',#11512,#11511,#9855,.T.);
#14392=EDGE_CURVE('',#11504,#11512,#137,.T.);
#14393=EDGE_CURVE('',#11513,#11513,#9856,.T.);
#14394=EDGE_CURVE('',#11513,#11514,#6175,.T.);
#14395=EDGE_CURVE('',#11514,#11514,#9857,.T.);
#14396=EDGE_CURVE('',#11515,#11516,#9858,.T.);
#14397=EDGE_CURVE('',#11517,#11515,#138,.T.);
#14398=EDGE_CURVE('',#11518,#11517,#9859,.T.);
#14399=EDGE_CURVE('',#11519,#11518,#139,.T.);
#14400=EDGE_CURVE('',#11520,#11519,#9860,.T.);
#14401=EDGE_CURVE('',#11520,#11521,#6176,.T.);
#14402=EDGE_CURVE('',#11521,#11521,#9861,.T.);
#14403=EDGE_CURVE('',#11522,#11520,#9862,.T.);
#14404=EDGE_CURVE('',#11523,#11522,#140,.T.);
#14405=EDGE_CURVE('',#11524,#11523,#9863,.T.);
#14406=EDGE_CURVE('',#11516,#11524,#141,.T.);
#14407=EDGE_CURVE('',#11525,#11525,#9864,.T.);
#14408=EDGE_CURVE('',#11525,#11526,#6177,.T.);
#14409=EDGE_CURVE('',#11526,#11526,#9865,.T.);
#14410=EDGE_CURVE('',#11527,#11528,#9866,.T.);
#14411=EDGE_CURVE('',#11529,#11527,#142,.T.);
#14412=EDGE_CURVE('',#11530,#11529,#9867,.T.);
#14413=EDGE_CURVE('',#11531,#11530,#143,.T.);
#14414=EDGE_CURVE('',#11532,#11531,#9868,.T.);
#14415=EDGE_CURVE('',#11532,#11533,#6178,.T.);
#14416=EDGE_CURVE('',#11533,#11533,#9869,.T.);
#14417=EDGE_CURVE('',#11534,#11532,#9870,.T.);
#14418=EDGE_CURVE('',#11535,#11534,#144,.T.);
#14419=EDGE_CURVE('',#11536,#11535,#9871,.T.);
#14420=EDGE_CURVE('',#11528,#11536,#145,.T.);
#14421=EDGE_CURVE('',#11537,#11447,#6179,.T.);
#14422=EDGE_CURVE('',#11538,#11446,#6180,.T.);
#14423=EDGE_CURVE('',#11537,#11538,#6181,.T.);
#14424=EDGE_CURVE('',#11443,#11459,#6182,.T.);
#14425=EDGE_CURVE('',#11444,#11462,#6183,.T.);
#14426=EDGE_CURVE('',#11452,#11463,#6184,.T.);
#14427=EDGE_CURVE('',#11445,#11458,#6185,.T.);
#14428=EDGE_CURVE('',#11457,#11470,#6186,.T.);
#14429=EDGE_CURVE('',#11469,#11482,#6187,.T.);
#14430=EDGE_CURVE('',#11481,#11494,#6188,.T.);
#14431=EDGE_CURVE('',#11493,#11506,#6189,.T.);
#14432=EDGE_CURVE('',#11505,#11518,#6190,.T.);
#14433=EDGE_CURVE('',#11517,#11530,#6191,.T.);
#14434=EDGE_CURVE('',#11529,#11539,#6192,.T.);
#14435=EDGE_CURVE('',#11540,#11539,#6193,.T.);
#14436=EDGE_CURVE('',#11541,#11540,#6194,.T.);
#14437=EDGE_CURVE('',#11541,#11538,#6195,.T.);
#14438=EDGE_CURVE('',#11542,#11451,#6196,.T.);
#14439=EDGE_CURVE('',#11542,#11543,#6197,.T.);
#14440=EDGE_CURVE('',#11543,#11544,#6198,.T.);
#14441=EDGE_CURVE('',#11545,#11544,#6199,.T.);
#14442=EDGE_CURVE('',#11536,#11545,#6200,.T.);
#14443=EDGE_CURVE('',#11524,#11535,#6201,.T.);
#14444=EDGE_CURVE('',#11512,#11523,#6202,.T.);
#14445=EDGE_CURVE('',#11500,#11511,#6203,.T.);
#14446=EDGE_CURVE('',#11488,#11499,#6204,.T.);
#14447=EDGE_CURVE('',#11476,#11487,#6205,.T.);
#14448=EDGE_CURVE('',#11464,#11475,#6206,.T.);
#14449=EDGE_CURVE('',#11455,#11471,#6207,.T.);
#14450=EDGE_CURVE('',#11456,#11474,#6208,.T.);
#14451=EDGE_CURVE('',#11467,#11483,#6209,.T.);
#14452=EDGE_CURVE('',#11468,#11486,#6210,.T.);
#14453=EDGE_CURVE('',#11480,#11498,#6211,.T.);
#14454=EDGE_CURVE('',#11479,#11495,#6212,.T.);
#14455=EDGE_CURVE('',#11491,#11507,#6213,.T.);
#14456=EDGE_CURVE('',#11492,#11510,#6214,.T.);
#14457=EDGE_CURVE('',#11503,#11519,#6215,.T.);
#14458=EDGE_CURVE('',#11504,#11522,#6216,.T.);
#14459=EDGE_CURVE('',#11515,#11531,#6217,.T.);
#14460=EDGE_CURVE('',#11516,#11534,#6218,.T.);
#14461=EDGE_CURVE('',#11527,#11546,#6219,.T.);
#14462=EDGE_CURVE('',#11528,#11547,#6220,.T.);
#14463=EDGE_CURVE('',#11547,#11546,#6221,.T.);
#14464=EDGE_CURVE('',#11545,#11547,#6222,.T.);
#14465=EDGE_CURVE('',#11548,#11541,#6223,.T.);
#14466=EDGE_CURVE('',#11549,#11548,#6224,.T.);
#14467=EDGE_CURVE('',#11549,#11550,#9872,.T.);
#14468=EDGE_CURVE('',#11551,#11550,#6225,.T.);
#14469=EDGE_CURVE('',#11551,#11552,#9873,.T.);
#14470=EDGE_CURVE('',#11553,#11552,#6226,.T.);
#14471=EDGE_CURVE('',#11553,#11554,#9874,.T.);
#14472=EDGE_CURVE('',#11555,#11554,#6227,.T.);
#14473=EDGE_CURVE('',#11555,#11556,#9875,.T.);
#14474=EDGE_CURVE('',#11556,#11557,#9876,.T.);
#14475=EDGE_CURVE('',#11557,#11558,#9877,.T.);
#14476=EDGE_CURVE('',#11559,#11558,#6228,.T.);
#14477=EDGE_CURVE('',#11559,#11560,#9878,.T.);
#14478=EDGE_CURVE('',#11561,#11560,#6229,.T.);
#14479=EDGE_CURVE('',#11561,#11562,#9879,.T.);
#14480=EDGE_CURVE('',#11563,#11562,#6230,.T.);
#14481=EDGE_CURVE('',#11563,#11564,#9880,.T.);
#14482=EDGE_CURVE('',#11564,#11565,#9881,.T.);
#14483=EDGE_CURVE('',#11565,#11566,#9882,.T.);
#14484=EDGE_CURVE('',#11567,#11566,#6231,.T.);
#14485=EDGE_CURVE('',#11568,#11567,#6232,.T.);
#14486=EDGE_CURVE('',#11568,#11569,#6233,.T.);
#14487=EDGE_CURVE('',#11569,#11570,#9883,.T.);
#14488=EDGE_CURVE('',#11571,#11570,#9884,.T.);
#14489=EDGE_CURVE('',#11571,#11572,#9885,.T.);
#14490=EDGE_CURVE('',#11572,#11573,#6234,.T.);
#14491=EDGE_CURVE('',#11573,#11574,#9886,.T.);
#14492=EDGE_CURVE('',#11574,#11575,#6235,.T.);
#14493=EDGE_CURVE('',#11575,#11576,#9887,.T.);
#14494=EDGE_CURVE('',#11576,#11577,#6236,.T.);
#14495=EDGE_CURVE('',#11577,#11578,#9888,.T.);
#14496=EDGE_CURVE('',#11579,#11578,#9889,.T.);
#14497=EDGE_CURVE('',#11579,#11580,#9890,.T.);
#14498=EDGE_CURVE('',#11580,#11581,#6237,.T.);
#14499=EDGE_CURVE('',#11581,#11582,#9891,.T.);
#14500=EDGE_CURVE('',#11582,#11583,#6238,.T.);
#14501=EDGE_CURVE('',#11583,#11584,#9892,.T.);
#14502=EDGE_CURVE('',#11584,#11585,#6239,.T.);
#14503=EDGE_CURVE('',#11585,#11586,#9893,.T.);
#14504=EDGE_CURVE('',#11586,#11587,#6240,.T.);
#14505=EDGE_CURVE('',#11587,#11543,#6241,.T.);
#14506=EDGE_CURVE('',#11542,#11588,#6242,.T.);
#14507=EDGE_CURVE('',#11588,#11537,#6243,.T.);
#14508=EDGE_CURVE('',#11546,#11539,#6244,.T.);
#14509=EDGE_CURVE('',#11589,#11544,#6245,.T.);
#14510=EDGE_CURVE('',#11590,#11589,#6246,.T.);
#14511=EDGE_CURVE('',#11590,#11591,#9894,.T.);
#14512=EDGE_CURVE('',#11592,#11591,#6247,.T.);
#14513=EDGE_CURVE('',#11592,#11593,#9895,.T.);
#14514=EDGE_CURVE('',#11594,#11593,#6248,.T.);
#14515=EDGE_CURVE('',#11594,#11595,#9896,.T.);
#14516=EDGE_CURVE('',#11596,#11595,#6249,.T.);
#14517=EDGE_CURVE('',#11596,#11597,#9897,.T.);
#14518=EDGE_CURVE('',#11597,#11598,#9898,.T.);
#14519=EDGE_CURVE('',#11598,#11599,#9899,.T.);
#14520=EDGE_CURVE('',#11600,#11599,#6250,.T.);
#14521=EDGE_CURVE('',#11600,#11601,#9900,.T.);
#14522=EDGE_CURVE('',#11602,#11601,#6251,.T.);
#14523=EDGE_CURVE('',#11602,#11603,#9901,.T.);
#14524=EDGE_CURVE('',#11604,#11603,#6252,.T.);
#14525=EDGE_CURVE('',#11604,#11605,#9902,.T.);
#14526=EDGE_CURVE('',#11605,#11606,#9903,.T.);
#14527=EDGE_CURVE('',#11606,#11607,#9904,.T.);
#14528=EDGE_CURVE('',#11608,#11607,#6253,.T.);
#14529=EDGE_CURVE('',#11608,#11609,#6254,.T.);
#14530=EDGE_CURVE('',#11609,#11610,#6255,.T.);
#14531=EDGE_CURVE('',#11610,#11611,#9905,.T.);
#14532=EDGE_CURVE('',#11612,#11611,#9906,.T.);
#14533=EDGE_CURVE('',#11612,#11613,#9907,.T.);
#14534=EDGE_CURVE('',#11613,#11614,#6256,.T.);
#14535=EDGE_CURVE('',#11614,#11615,#9908,.T.);
#14536=EDGE_CURVE('',#11615,#11616,#6257,.T.);
#14537=EDGE_CURVE('',#11616,#11617,#9909,.T.);
#14538=EDGE_CURVE('',#11617,#11618,#6258,.T.);
#14539=EDGE_CURVE('',#11618,#11619,#9910,.T.);
#14540=EDGE_CURVE('',#11620,#11619,#9911,.T.);
#14541=EDGE_CURVE('',#11620,#11621,#9912,.T.);
#14542=EDGE_CURVE('',#11621,#11622,#6259,.T.);
#14543=EDGE_CURVE('',#11622,#11623,#9913,.T.);
#14544=EDGE_CURVE('',#11623,#11624,#6260,.T.);
#14545=EDGE_CURVE('',#11624,#11625,#9914,.T.);
#14546=EDGE_CURVE('',#11625,#11626,#6261,.T.);
#14547=EDGE_CURVE('',#11626,#11627,#9915,.T.);
#14548=EDGE_CURVE('',#11627,#11628,#6262,.T.);
#14549=EDGE_CURVE('',#11628,#11540,#6263,.T.);
#14550=EDGE_CURVE('',#11595,#11581,#6264,.T.);
#14551=EDGE_CURVE('',#11580,#11596,#6265,.T.);
#14552=EDGE_CURVE('',#11576,#11600,#6266,.T.);
#14553=EDGE_CURVE('',#11599,#11577,#6267,.T.);
#14554=EDGE_CURVE('',#11572,#11604,#6268,.T.);
#14555=EDGE_CURVE('',#11603,#11573,#6269,.T.);
#14556=EDGE_CURVE('',#11607,#11569,#6270,.T.);
#14557=EDGE_CURVE('',#11568,#11608,#6271,.T.);
#14558=EDGE_CURVE('',#11554,#11622,#6272,.T.);
#14559=EDGE_CURVE('',#11621,#11555,#6273,.T.);
#14560=EDGE_CURVE('',#11613,#11563,#6274,.T.);
#14561=EDGE_CURVE('',#11562,#11614,#6275,.T.);
#14562=EDGE_CURVE('',#11567,#11609,#6276,.T.);
#14563=EDGE_CURVE('',#11548,#11628,#6277,.T.);
#14564=EDGE_CURVE('',#11627,#11549,#6278,.T.);
#14565=EDGE_CURVE('',#11550,#11626,#6279,.T.);
#14566=EDGE_CURVE('',#11625,#11551,#6280,.T.);
#14567=EDGE_CURVE('',#11552,#11624,#6281,.T.);
#14568=EDGE_CURVE('',#11623,#11553,#6282,.T.);
#14569=EDGE_CURVE('',#11617,#11559,#6283,.T.);
#14570=EDGE_CURVE('',#11558,#11618,#6284,.T.);
#14571=EDGE_CURVE('',#11615,#11561,#6285,.T.);
#14572=EDGE_CURVE('',#11560,#11616,#6286,.T.);
#14573=EDGE_CURVE('',#11566,#11610,#6287,.T.);
#14574=EDGE_CURVE('',#11564,#11612,#6288,.T.);
#14575=EDGE_CURVE('',#11611,#11565,#6289,.T.);
#14576=EDGE_CURVE('',#11619,#11557,#6290,.T.);
#14577=EDGE_CURVE('',#11556,#11620,#6291,.T.);
#14578=EDGE_CURVE('',#11574,#11602,#6292,.T.);
#14579=EDGE_CURVE('',#11601,#11575,#6293,.T.);
#14580=EDGE_CURVE('',#11593,#11583,#6294,.T.);
#14581=EDGE_CURVE('',#11582,#11594,#6295,.T.);
#14582=EDGE_CURVE('',#11591,#11585,#6296,.T.);
#14583=EDGE_CURVE('',#11584,#11592,#6297,.T.);
#14584=EDGE_CURVE('',#11586,#11590,#6298,.T.);
#14585=EDGE_CURVE('',#11587,#11589,#6299,.T.);
#14586=EDGE_CURVE('',#11605,#11571,#6300,.T.);
#14587=EDGE_CURVE('',#11570,#11606,#6301,.T.);
#14588=EDGE_CURVE('',#11578,#11598,#6302,.T.);
#14589=EDGE_CURVE('',#11597,#11579,#6303,.T.);
#14590=EDGE_CURVE('',#11588,#11450,#6304,.T.);
#14591=EDGE_CURVE('',#11629,#11629,#9916,.T.);
#14592=EDGE_CURVE('',#11629,#11630,#6305,.T.);
#14593=EDGE_CURVE('',#11630,#11630,#9917,.T.);
#14594=EDGE_CURVE('',#11631,#11631,#9918,.T.);
#14595=EDGE_CURVE('',#11631,#11632,#6306,.T.);
#14596=EDGE_CURVE('',#11632,#11632,#9919,.T.);
#14597=EDGE_CURVE('',#11633,#11633,#9920,.T.);
#14598=EDGE_CURVE('',#11633,#11634,#6307,.T.);
#14599=EDGE_CURVE('',#11634,#11634,#9921,.T.);
#14600=EDGE_CURVE('',#11635,#11629,#6308,.T.);
#14601=EDGE_CURVE('',#11636,#11631,#6309,.T.);
#14602=EDGE_CURVE('',#11637,#11637,#9922,.T.);
#14603=EDGE_CURVE('',#11637,#11638,#6310,.T.);
#14604=EDGE_CURVE('',#11638,#11638,#9923,.T.);
#14605=EDGE_CURVE('',#11639,#11639,#9924,.T.);
#14606=EDGE_CURVE('',#11639,#11640,#6311,.T.);
#14607=EDGE_CURVE('',#11640,#11640,#9925,.T.);
#14608=EDGE_CURVE('',#11641,#11641,#9926,.T.);
#14609=EDGE_CURVE('',#11641,#11642,#6312,.T.);
#14610=EDGE_CURVE('',#11642,#11642,#9927,.T.);
#14611=EDGE_CURVE('',#11643,#11643,#9928,.T.);
#14612=EDGE_CURVE('',#11643,#11644,#6313,.T.);
#14613=EDGE_CURVE('',#11644,#11644,#9929,.T.);
#14614=EDGE_CURVE('',#11645,#11645,#9930,.T.);
#14615=EDGE_CURVE('',#11645,#11646,#6314,.T.);
#14616=EDGE_CURVE('',#11646,#11646,#9931,.T.);
#14617=EDGE_CURVE('',#11647,#11647,#9932,.T.);
#14618=EDGE_CURVE('',#11647,#11648,#6315,.T.);
#14619=EDGE_CURVE('',#11648,#11648,#9933,.T.);
#14620=EDGE_CURVE('',#11649,#11649,#9934,.T.);
#14621=EDGE_CURVE('',#11649,#11650,#6316,.T.);
#14622=EDGE_CURVE('',#11650,#11650,#9935,.T.);
#14623=EDGE_CURVE('',#11651,#11651,#9936,.T.);
#14624=EDGE_CURVE('',#11651,#11652,#6317,.T.);
#14625=EDGE_CURVE('',#11652,#11653,#9937,.T.);
#14626=EDGE_CURVE('',#11653,#11654,#6318,.T.);
#14627=EDGE_CURVE('',#11654,#11655,#9938,.T.);
#14628=EDGE_CURVE('',#11652,#11655,#6319,.T.);
#14629=EDGE_CURVE('',#11656,#11645,#6320,.T.);
#14630=EDGE_CURVE('',#11657,#11647,#6321,.T.);
#14631=EDGE_CURVE('',#11658,#11658,#9939,.T.);
#14632=EDGE_CURVE('',#11658,#11659,#6322,.T.);
#14633=EDGE_CURVE('',#11659,#11660,#6323,.T.);
#14634=EDGE_CURVE('',#11660,#11661,#9940,.T.);
#14635=EDGE_CURVE('',#11662,#11661,#6324,.T.);
#14636=EDGE_CURVE('',#11662,#11659,#9941,.T.);
#14637=EDGE_CURVE('',#11663,#11664,#860,.T.);
#14638=EDGE_CURVE('',#11665,#11663,#861,.T.);
#14639=EDGE_CURVE('',#11666,#11665,#862,.T.);
#14640=EDGE_CURVE('',#11666,#11667,#11,.T.);
#14641=EDGE_CURVE('',#11668,#11667,#9942,.T.);
#14642=EDGE_CURVE('',#11667,#11668,#9943,.T.);
#14643=EDGE_CURVE('',#11669,#11666,#863,.T.);
#14644=EDGE_CURVE('',#11670,#11669,#864,.T.);
#14645=EDGE_CURVE('',#11664,#11670,#865,.T.);
#14646=EDGE_CURVE('',#11671,#11671,#9944,.T.);
#14647=EDGE_CURVE('',#11671,#11668,#6325,.T.);
#14648=EDGE_CURVE('',#11672,#11672,#9945,.T.);
#14649=EDGE_CURVE('',#11672,#11673,#6326,.T.);
#14650=EDGE_CURVE('',#11673,#11673,#9946,.T.);
#14651=EDGE_CURVE('',#11674,#11675,#146,.T.);
#14652=EDGE_CURVE('',#11676,#11674,#6327,.T.);
#14653=EDGE_CURVE('',#11676,#11677,#6328,.T.);
#14654=EDGE_CURVE('',#11677,#11675,#6329,.T.);
#14655=EDGE_CURVE('',#11678,#11674,#147,.T.);
#14656=EDGE_CURVE('',#11678,#11679,#6330,.T.);
#14657=EDGE_CURVE('',#11680,#11679,#148,.T.);
#14658=EDGE_CURVE('',#11674,#11680,#6331,.T.);
#14659=EDGE_CURVE('',#11681,#11682,#149,.T.);
#14660=EDGE_CURVE('',#11681,#11683,#6332,.T.);
#14661=EDGE_CURVE('',#11684,#11683,#150,.T.);
#14662=EDGE_CURVE('',#11682,#11684,#6333,.T.);
#14663=EDGE_CURVE('',#11683,#11685,#151,.T.);
#14664=EDGE_CURVE('',#11683,#11686,#6334,.T.);
#14665=EDGE_CURVE('',#11687,#11686,#6335,.T.);
#14666=EDGE_CURVE('',#11685,#11687,#6336,.T.);
#14667=EDGE_CURVE('',#11688,#11689,#6337,.T.);
#14668=EDGE_CURVE('',#11688,#11690,#6338,.T.);
#14669=EDGE_CURVE('',#11690,#11691,#6339,.T.);
#14670=EDGE_CURVE('',#11691,#11689,#6340,.T.);
#14671=EDGE_CURVE('',#11692,#11693,#6341,.T.);
#14672=EDGE_CURVE('',#11692,#11694,#6342,.T.);
#14673=EDGE_CURVE('',#11694,#11695,#6343,.T.);
#14674=EDGE_CURVE('',#11695,#11693,#6344,.T.);
#14675=EDGE_CURVE('',#11696,#11697,#6345,.T.);
#14676=EDGE_CURVE('',#11696,#11698,#6346,.T.);
#14677=EDGE_CURVE('',#11698,#11699,#6347,.T.);
#14678=EDGE_CURVE('',#11699,#11697,#6348,.T.);
#14679=EDGE_CURVE('',#11700,#11701,#6349,.T.);
#14680=EDGE_CURVE('',#11700,#11702,#6350,.T.);
#14681=EDGE_CURVE('',#11702,#11703,#6351,.T.);
#14682=EDGE_CURVE('',#11703,#11701,#6352,.T.);
#14683=EDGE_CURVE('',#11704,#11705,#6353,.T.);
#14684=EDGE_CURVE('',#11704,#11706,#6354,.T.);
#14685=EDGE_CURVE('',#11706,#11707,#6355,.T.);
#14686=EDGE_CURVE('',#11707,#11705,#6356,.T.);
#14687=EDGE_CURVE('',#11708,#11709,#6357,.T.);
#14688=EDGE_CURVE('',#11708,#11710,#6358,.T.);
#14689=EDGE_CURVE('',#11710,#11711,#6359,.T.);
#14690=EDGE_CURVE('',#11711,#11709,#6360,.T.);
#14691=EDGE_CURVE('',#11712,#11713,#6361,.T.);
#14692=EDGE_CURVE('',#11712,#11714,#6362,.T.);
#14693=EDGE_CURVE('',#11714,#11715,#6363,.T.);
#14694=EDGE_CURVE('',#11715,#11713,#6364,.T.);
#14695=EDGE_CURVE('',#11716,#11717,#6365,.T.);
#14696=EDGE_CURVE('',#11716,#11718,#6366,.T.);
#14697=EDGE_CURVE('',#11718,#11719,#6367,.T.);
#14698=EDGE_CURVE('',#11719,#11717,#6368,.T.);
#14699=EDGE_CURVE('',#11720,#11721,#6369,.T.);
#14700=EDGE_CURVE('',#11722,#11720,#6370,.T.);
#14701=EDGE_CURVE('',#11722,#11723,#6371,.T.);
#14702=EDGE_CURVE('',#11723,#11721,#6372,.T.);
#14703=EDGE_CURVE('',#11724,#11720,#6373,.T.);
#14704=EDGE_CURVE('',#11725,#11724,#6374,.T.);
#14705=EDGE_CURVE('',#11725,#11722,#6375,.T.);
#14706=EDGE_CURVE('',#11726,#11727,#6376,.T.);
#14707=EDGE_CURVE('',#11728,#11726,#6377,.T.);
#14708=EDGE_CURVE('',#11728,#11729,#6378,.T.);
#14709=EDGE_CURVE('',#11729,#11727,#6379,.T.);
#14710=EDGE_CURVE('',#11730,#11726,#6380,.T.);
#14711=EDGE_CURVE('',#11730,#11731,#6381,.T.);
#14712=EDGE_CURVE('',#11731,#11728,#6382,.T.);
#14713=EDGE_CURVE('',#11732,#11733,#6383,.T.);
#14714=EDGE_CURVE('',#11732,#11734,#6384,.T.);
#14715=EDGE_CURVE('',#11734,#11735,#6385,.T.);
#14716=EDGE_CURVE('',#11735,#11733,#6386,.T.);
#14717=EDGE_CURVE('',#11736,#11737,#6387,.T.);
#14718=EDGE_CURVE('',#11736,#11738,#6388,.T.);
#14719=EDGE_CURVE('',#11738,#11739,#6389,.T.);
#14720=EDGE_CURVE('',#11739,#11737,#6390,.T.);
#14721=EDGE_CURVE('',#11740,#11741,#6391,.T.);
#14722=EDGE_CURVE('',#11740,#11742,#6392,.T.);
#14723=EDGE_CURVE('',#11742,#11743,#6393,.T.);
#14724=EDGE_CURVE('',#11743,#11741,#6394,.T.);
#14725=EDGE_CURVE('',#11744,#11745,#6395,.T.);
#14726=EDGE_CURVE('',#11746,#11744,#6396,.T.);
#14727=EDGE_CURVE('',#11746,#11747,#6397,.T.);
#14728=EDGE_CURVE('',#11747,#11745,#6398,.T.);
#14729=EDGE_CURVE('',#11701,#11744,#6399,.T.);
#14730=EDGE_CURVE('',#11703,#11746,#6400,.T.);
#14731=EDGE_CURVE('',#11748,#11749,#9947,.T.);
#14732=EDGE_CURVE('',#11748,#11750,#6401,.T.);
#14733=EDGE_CURVE('',#11750,#11751,#9948,.T.);
#14734=EDGE_CURVE('',#11751,#11749,#6402,.T.);
#14735=EDGE_CURVE('',#11752,#11753,#9949,.T.);
#14736=EDGE_CURVE('',#11752,#11754,#6403,.T.);
#14737=EDGE_CURVE('',#11754,#11755,#9950,.T.);
#14738=EDGE_CURVE('',#11755,#11753,#6404,.T.);
#14739=EDGE_CURVE('',#11756,#11757,#9951,.T.);
#14740=EDGE_CURVE('',#11756,#11758,#6405,.T.);
#14741=EDGE_CURVE('',#11758,#11759,#9952,.T.);
#14742=EDGE_CURVE('',#11759,#11757,#6406,.T.);
#14743=EDGE_CURVE('',#11760,#11761,#9953,.T.);
#14744=EDGE_CURVE('',#11760,#11762,#6407,.T.);
#14745=EDGE_CURVE('',#11762,#11763,#9954,.T.);
#14746=EDGE_CURVE('',#11763,#11761,#6408,.T.);
#14747=EDGE_CURVE('',#11733,#11730,#9955,.T.);
#14748=EDGE_CURVE('',#11731,#11735,#9956,.T.);
#14749=EDGE_CURVE('',#11721,#11716,#9957,.T.);
#14750=EDGE_CURVE('',#11718,#11723,#9958,.T.);
#14751=EDGE_CURVE('',#11741,#11736,#9959,.T.);
#14752=EDGE_CURVE('',#11738,#11743,#9960,.T.);
#14753=EDGE_CURVE('',#11693,#11740,#9961,.T.);
#14754=EDGE_CURVE('',#11742,#11695,#9962,.T.);
#14755=EDGE_CURVE('',#11757,#11692,#9963,.T.);
#14756=EDGE_CURVE('',#11694,#11759,#9964,.T.);
#14757=EDGE_CURVE('',#11745,#11756,#9965,.T.);
#14758=EDGE_CURVE('',#11758,#11747,#9966,.T.);
#14759=EDGE_CURVE('',#11737,#11760,#9967,.T.);
#14760=EDGE_CURVE('',#11762,#11739,#9968,.T.);
#14761=EDGE_CURVE('',#11761,#11688,#9969,.T.);
#14762=EDGE_CURVE('',#11690,#11763,#9970,.T.);
#14763=EDGE_CURVE('',#11689,#11732,#9971,.T.);
#14764=EDGE_CURVE('',#11734,#11691,#9972,.T.);
#14765=EDGE_CURVE('',#11717,#11712,#9973,.T.);
#14766=EDGE_CURVE('',#11714,#11719,#9974,.T.);
#14767=EDGE_CURVE('',#11713,#11752,#9975,.T.);
#14768=EDGE_CURVE('',#11754,#11715,#9976,.T.);
#14769=EDGE_CURVE('',#11753,#11696,#9977,.T.);
#14770=EDGE_CURVE('',#11698,#11755,#9978,.T.);
#14771=EDGE_CURVE('',#11697,#11708,#9979,.T.);
#14772=EDGE_CURVE('',#11710,#11699,#9980,.T.);
#14773=EDGE_CURVE('',#11709,#11704,#9981,.T.);
#14774=EDGE_CURVE('',#11706,#11711,#9982,.T.);
#14775=EDGE_CURVE('',#11705,#11748,#9983,.T.);
#14776=EDGE_CURVE('',#11750,#11707,#9984,.T.);
#14777=EDGE_CURVE('',#11749,#11700,#9985,.T.);
#14778=EDGE_CURVE('',#11702,#11751,#9986,.T.);
#14779=EDGE_CURVE('',#11764,#11765,#6409,.T.);
#14780=EDGE_CURVE('',#11766,#11765,#6410,.T.);
#14781=EDGE_CURVE('',#11767,#11766,#6411,.T.);
#14782=EDGE_CURVE('',#11764,#11767,#6412,.T.);
#14783=EDGE_CURVE('',#11725,#11768,#6413,.T.);
#14784=EDGE_CURVE('',#11768,#11769,#6414,.T.);
#14785=EDGE_CURVE('',#11769,#11764,#6415,.T.);
#14786=EDGE_CURVE('',#11767,#11770,#6416,.T.);
#14787=EDGE_CURVE('',#11770,#11771,#6417,.T.);
#14788=EDGE_CURVE('',#11771,#11729,#6418,.T.);
#14789=EDGE_CURVE('',#11769,#11772,#6419,.T.);
#14790=EDGE_CURVE('',#11765,#11772,#6420,.T.);
#14791=EDGE_CURVE('',#11768,#11773,#6421,.T.);
#14792=EDGE_CURVE('',#11772,#11773,#6422,.T.);
#14793=EDGE_CURVE('',#11773,#11724,#6423,.T.);
#14794=EDGE_CURVE('',#11771,#11774,#6424,.T.);
#14795=EDGE_CURVE('',#11727,#11774,#6425,.T.);
#14796=EDGE_CURVE('',#11770,#11775,#6426,.T.);
#14797=EDGE_CURVE('',#11774,#11775,#6427,.T.);
#14798=EDGE_CURVE('',#11775,#11766,#6428,.T.);
#14799=EDGE_CURVE('',#11776,#11664,#6429,.T.);
#14800=EDGE_CURVE('',#11777,#11670,#6430,.T.);
#14801=EDGE_CURVE('',#11776,#11777,#6431,.T.);
#14802=EDGE_CURVE('',#11778,#11776,#6432,.T.);
#14803=EDGE_CURVE('',#11778,#11663,#6433,.T.);
#14804=EDGE_CURVE('',#11779,#11665,#6434,.T.);
#14805=EDGE_CURVE('',#11779,#11778,#6435,.T.);
#14806=EDGE_CURVE('',#11780,#11666,#6436,.T.);
#14807=EDGE_CURVE('',#11780,#11779,#6437,.T.);
#14808=EDGE_CURVE('',#11781,#11669,#6438,.T.);
#14809=EDGE_CURVE('',#11781,#11780,#6439,.T.);
#14810=EDGE_CURVE('',#11777,#11781,#6440,.T.);
#14811=EDGE_CURVE('',#11782,#11783,#6441,.T.);
#14812=EDGE_CURVE('',#11784,#11782,#9987,.T.);
#14813=EDGE_CURVE('',#11785,#11784,#6442,.T.);
#14814=EDGE_CURVE('',#11786,#11785,#9988,.T.);
#14815=EDGE_CURVE('',#11787,#11786,#6443,.T.);
#14816=EDGE_CURVE('',#11788,#11787,#9989,.T.);
#14817=EDGE_CURVE('',#11789,#11788,#9990,.T.);
#14818=EDGE_CURVE('',#11790,#11789,#9991,.T.);
#14819=EDGE_CURVE('',#11791,#11790,#6444,.T.);
#14820=EDGE_CURVE('',#11792,#11791,#9992,.T.);
#14821=EDGE_CURVE('',#11793,#11792,#6445,.T.);
#14822=EDGE_CURVE('',#11794,#11793,#9993,.T.);
#14823=EDGE_CURVE('',#11795,#11794,#6446,.T.);
#14824=EDGE_CURVE('',#11796,#11795,#9994,.T.);
#14825=EDGE_CURVE('',#11797,#11796,#9995,.T.);
#14826=EDGE_CURVE('',#11798,#11797,#9996,.T.);
#14827=EDGE_CURVE('',#11799,#11798,#6447,.T.);
#14828=EDGE_CURVE('',#11800,#11799,#6448,.T.);
#14829=EDGE_CURVE('',#11801,#11800,#6449,.T.);
#14830=EDGE_CURVE('',#11802,#11801,#9997,.T.);
#14831=EDGE_CURVE('',#11803,#11802,#9998,.T.);
#14832=EDGE_CURVE('',#11804,#11803,#9999,.T.);
#14833=EDGE_CURVE('',#11805,#11804,#6450,.T.);
#14834=EDGE_CURVE('',#11806,#11805,#10000,.T.);
#14835=EDGE_CURVE('',#11807,#11806,#6451,.T.);
#14836=EDGE_CURVE('',#11808,#11807,#10001,.T.);
#14837=EDGE_CURVE('',#11809,#11808,#6452,.T.);
#14838=EDGE_CURVE('',#11810,#11809,#10002,.T.);
#14839=EDGE_CURVE('',#11811,#11810,#10003,.T.);
#14840=EDGE_CURVE('',#11812,#11811,#10004,.T.);
#14841=EDGE_CURVE('',#11813,#11812,#6453,.T.);
#14842=EDGE_CURVE('',#11814,#11813,#10005,.T.);
#14843=EDGE_CURVE('',#11815,#11814,#6454,.T.);
#14844=EDGE_CURVE('',#11816,#11815,#10006,.T.);
#14845=EDGE_CURVE('',#11817,#11816,#6455,.T.);
#14846=EDGE_CURVE('',#11818,#11817,#6456,.T.);
#14847=EDGE_CURVE('',#11819,#11818,#6457,.T.);
#14848=EDGE_CURVE('',#11820,#11819,#6458,.T.);
#14849=EDGE_CURVE('',#11821,#11820,#6459,.T.);
#14850=EDGE_CURVE('',#11822,#11821,#6460,.T.);
#14851=EDGE_CURVE('',#11823,#11822,#6461,.T.);
#14852=EDGE_CURVE('',#11824,#11823,#6462,.T.);
#14853=EDGE_CURVE('',#11825,#11824,#6463,.T.);
#14854=EDGE_CURVE('',#11783,#11825,#6464,.T.);
#14855=EDGE_CURVE('',#11826,#11827,#6465,.T.);
#14856=EDGE_CURVE('',#11782,#11826,#6466,.T.);
#14857=EDGE_CURVE('',#11783,#11827,#6467,.T.);
#14858=EDGE_CURVE('',#11828,#11826,#10007,.T.);
#14859=EDGE_CURVE('',#11784,#11828,#6468,.T.);
#14860=EDGE_CURVE('',#11829,#11828,#6469,.T.);
#14861=EDGE_CURVE('',#11785,#11829,#6470,.T.);
#14862=EDGE_CURVE('',#11830,#11829,#10008,.T.);
#14863=EDGE_CURVE('',#11786,#11830,#6471,.T.);
#14864=EDGE_CURVE('',#11831,#11830,#6472,.T.);
#14865=EDGE_CURVE('',#11787,#11831,#6473,.T.);
#14866=EDGE_CURVE('',#11832,#11831,#10009,.T.);
#14867=EDGE_CURVE('',#11788,#11832,#6474,.T.);
#14868=EDGE_CURVE('',#11833,#11832,#10010,.T.);
#14869=EDGE_CURVE('',#11789,#11833,#6475,.T.);
#14870=EDGE_CURVE('',#11834,#11833,#10011,.T.);
#14871=EDGE_CURVE('',#11790,#11834,#6476,.T.);
#14872=EDGE_CURVE('',#11835,#11834,#6477,.T.);
#14873=EDGE_CURVE('',#11791,#11835,#6478,.T.);
#14874=EDGE_CURVE('',#11836,#11835,#10012,.T.);
#14875=EDGE_CURVE('',#11792,#11836,#6479,.T.);
#14876=EDGE_CURVE('',#11837,#11836,#6480,.T.);
#14877=EDGE_CURVE('',#11793,#11837,#6481,.T.);
#14878=EDGE_CURVE('',#11838,#11837,#10013,.T.);
#14879=EDGE_CURVE('',#11794,#11838,#6482,.T.);
#14880=EDGE_CURVE('',#11839,#11838,#6483,.T.);
#14881=EDGE_CURVE('',#11795,#11839,#6484,.T.);
#14882=EDGE_CURVE('',#11840,#11839,#10014,.T.);
#14883=EDGE_CURVE('',#11796,#11840,#6485,.T.);
#14884=EDGE_CURVE('',#11841,#11840,#10015,.T.);
#14885=EDGE_CURVE('',#11797,#11841,#6486,.T.);
#14886=EDGE_CURVE('',#11842,#11841,#10016,.T.);
#14887=EDGE_CURVE('',#11798,#11842,#6487,.T.);
#14888=EDGE_CURVE('',#11843,#11842,#6488,.T.);
#14889=EDGE_CURVE('',#11799,#11843,#6489,.T.);
#14890=EDGE_CURVE('',#11844,#11843,#6490,.T.);
#14891=EDGE_CURVE('',#11800,#11844,#6491,.T.);
#14892=EDGE_CURVE('',#11845,#11844,#6492,.T.);
#14893=EDGE_CURVE('',#11801,#11845,#6493,.T.);
#14894=EDGE_CURVE('',#11846,#11845,#10017,.T.);
#14895=EDGE_CURVE('',#11802,#11846,#6494,.T.);
#14896=EDGE_CURVE('',#11847,#11846,#10018,.T.);
#14897=EDGE_CURVE('',#11803,#11847,#6495,.T.);
#14898=EDGE_CURVE('',#11848,#11847,#10019,.T.);
#14899=EDGE_CURVE('',#11804,#11848,#6496,.T.);
#14900=EDGE_CURVE('',#11849,#11848,#6497,.T.);
#14901=EDGE_CURVE('',#11805,#11849,#6498,.T.);
#14902=EDGE_CURVE('',#11850,#11849,#10020,.T.);
#14903=EDGE_CURVE('',#11806,#11850,#6499,.T.);
#14904=EDGE_CURVE('',#11851,#11850,#6500,.T.);
#14905=EDGE_CURVE('',#11807,#11851,#6501,.T.);
#14906=EDGE_CURVE('',#11852,#11851,#10021,.T.);
#14907=EDGE_CURVE('',#11808,#11852,#6502,.T.);
#14908=EDGE_CURVE('',#11853,#11852,#6503,.T.);
#14909=EDGE_CURVE('',#11809,#11853,#6504,.T.);
#14910=EDGE_CURVE('',#11854,#11853,#10022,.T.);
#14911=EDGE_CURVE('',#11810,#11854,#6505,.T.);
#14912=EDGE_CURVE('',#11855,#11854,#10023,.T.);
#14913=EDGE_CURVE('',#11811,#11855,#6506,.T.);
#14914=EDGE_CURVE('',#11856,#11855,#10024,.T.);
#14915=EDGE_CURVE('',#11812,#11856,#6507,.T.);
#14916=EDGE_CURVE('',#11857,#11856,#6508,.T.);
#14917=EDGE_CURVE('',#11813,#11857,#6509,.T.);
#14918=EDGE_CURVE('',#11858,#11857,#10025,.T.);
#14919=EDGE_CURVE('',#11814,#11858,#6510,.T.);
#14920=EDGE_CURVE('',#11859,#11858,#6511,.T.);
#14921=EDGE_CURVE('',#11815,#11859,#6512,.T.);
#14922=EDGE_CURVE('',#11860,#11859,#10026,.T.);
#14923=EDGE_CURVE('',#11816,#11860,#6513,.T.);
#14924=EDGE_CURVE('',#11861,#11860,#6514,.T.);
#14925=EDGE_CURVE('',#11817,#11861,#6515,.T.);
#14926=EDGE_CURVE('',#11862,#11861,#6516,.T.);
#14927=EDGE_CURVE('',#11818,#11862,#6517,.T.);
#14928=EDGE_CURVE('',#11863,#11862,#6518,.T.);
#14929=EDGE_CURVE('',#11819,#11863,#6519,.T.);
#14930=EDGE_CURVE('',#11864,#11863,#6520,.T.);
#14931=EDGE_CURVE('',#11820,#11864,#6521,.T.);
#14932=EDGE_CURVE('',#11865,#11864,#6522,.T.);
#14933=EDGE_CURVE('',#11821,#11865,#6523,.T.);
#14934=EDGE_CURVE('',#11866,#11865,#6524,.T.);
#14935=EDGE_CURVE('',#11822,#11866,#6525,.T.);
#14936=EDGE_CURVE('',#11867,#11866,#6526,.T.);
#14937=EDGE_CURVE('',#11823,#11867,#6527,.T.);
#14938=EDGE_CURVE('',#11868,#11867,#6528,.T.);
#14939=EDGE_CURVE('',#11824,#11868,#6529,.T.);
#14940=EDGE_CURVE('',#11869,#11868,#6530,.T.);
#14941=EDGE_CURVE('',#11825,#11869,#6531,.T.);
#14942=EDGE_CURVE('',#11827,#11869,#6532,.T.);
#14943=EDGE_CURVE('',#11662,#11870,#6533,.T.);
#14944=EDGE_CURVE('',#11870,#11871,#10027,.T.);
#14945=EDGE_CURVE('',#11871,#11659,#6534,.T.);
#14946=EDGE_CURVE('',#11872,#11873,#6535,.T.);
#14947=EDGE_CURVE('',#11874,#11872,#6536,.T.);
#14948=EDGE_CURVE('',#11875,#11874,#10028,.T.);
#14949=EDGE_CURVE('',#11876,#11875,#6537,.T.);
#14950=EDGE_CURVE('',#11877,#11876,#6538,.T.);
#14951=EDGE_CURVE('',#11878,#11877,#6539,.T.);
#14952=EDGE_CURVE('',#11879,#11878,#6540,.T.);
#14953=EDGE_CURVE('',#11880,#11879,#6541,.T.);
#14954=EDGE_CURVE('',#11880,#11881,#6542,.T.);
#14955=EDGE_CURVE('',#11881,#11882,#6543,.T.);
#14956=EDGE_CURVE('',#11882,#11883,#10029,.T.);
#14957=EDGE_CURVE('',#11883,#11884,#6544,.T.);
#14958=EDGE_CURVE('',#11884,#11885,#10030,.T.);
#14959=EDGE_CURVE('',#11885,#11886,#6545,.T.);
#14960=EDGE_CURVE('',#11886,#11887,#10031,.T.);
#14961=EDGE_CURVE('',#11887,#11888,#10032,.T.);
#14962=EDGE_CURVE('',#11888,#11889,#10033,.T.);
#14963=EDGE_CURVE('',#11889,#11890,#6546,.T.);
#14964=EDGE_CURVE('',#11890,#11891,#10034,.T.);
#14965=EDGE_CURVE('',#11891,#11892,#6547,.T.);
#14966=EDGE_CURVE('',#11892,#11893,#10035,.T.);
#14967=EDGE_CURVE('',#11893,#11894,#6548,.T.);
#14968=EDGE_CURVE('',#11894,#11895,#10036,.T.);
#14969=EDGE_CURVE('',#11895,#11896,#10037,.T.);
#14970=EDGE_CURVE('',#11896,#11897,#10038,.T.);
#14971=EDGE_CURVE('',#11897,#11898,#6549,.T.);
#14972=EDGE_CURVE('',#11898,#11899,#6550,.T.);
#14973=EDGE_CURVE('',#11899,#11900,#6551,.T.);
#14974=EDGE_CURVE('',#11900,#11901,#10039,.T.);
#14975=EDGE_CURVE('',#11901,#11902,#10040,.T.);
#14976=EDGE_CURVE('',#11902,#11903,#10041,.T.);
#14977=EDGE_CURVE('',#11903,#11904,#6552,.T.);
#14978=EDGE_CURVE('',#11904,#11905,#10042,.T.);
#14979=EDGE_CURVE('',#11905,#11906,#6553,.T.);
#14980=EDGE_CURVE('',#11906,#11907,#10043,.T.);
#14981=EDGE_CURVE('',#11907,#11908,#6554,.T.);
#14982=EDGE_CURVE('',#11908,#11909,#10044,.T.);
#14983=EDGE_CURVE('',#11909,#11910,#10045,.T.);
#14984=EDGE_CURVE('',#11910,#11911,#10046,.T.);
#14985=EDGE_CURVE('',#11911,#11912,#6555,.T.);
#14986=EDGE_CURVE('',#11912,#11913,#10047,.T.);
#14987=EDGE_CURVE('',#11913,#11914,#6556,.T.);
#14988=EDGE_CURVE('',#11914,#11915,#10048,.T.);
#14989=EDGE_CURVE('',#11915,#11916,#6557,.T.);
#14990=EDGE_CURVE('',#11916,#11917,#6558,.T.);
#14991=EDGE_CURVE('',#11918,#11917,#6559,.T.);
#14992=EDGE_CURVE('',#11919,#11918,#6560,.T.);
#14993=EDGE_CURVE('',#11873,#11919,#6561,.T.);
#14994=EDGE_CURVE('',#11920,#11660,#6562,.T.);
#14995=EDGE_CURVE('',#11871,#11920,#6563,.T.);
#14996=EDGE_CURVE('',#11661,#11921,#6564,.T.);
#14997=EDGE_CURVE('',#11870,#11921,#6565,.T.);
#14998=EDGE_CURVE('',#11921,#11920,#10049,.T.);
#14999=EDGE_CURVE('',#11652,#11922,#6566,.T.);
#15000=EDGE_CURVE('',#11922,#11923,#10050,.T.);
#15001=EDGE_CURVE('',#11923,#11653,#6567,.T.);
#15002=EDGE_CURVE('',#11924,#11925,#6568,.T.);
#15003=EDGE_CURVE('',#11925,#11917,#6569,.T.);
#15004=EDGE_CURVE('',#11924,#11916,#6570,.T.);
#15005=EDGE_CURVE('',#11925,#11926,#6571,.T.);
#15006=EDGE_CURVE('',#11926,#11918,#6572,.T.);
#15007=EDGE_CURVE('',#11926,#11927,#6573,.T.);
#15008=EDGE_CURVE('',#11927,#11919,#6574,.T.);
#15009=EDGE_CURVE('',#11927,#11928,#6575,.T.);
#15010=EDGE_CURVE('',#11928,#11873,#6576,.T.);
#15011=EDGE_CURVE('',#11929,#11930,#6577,.T.);
#15012=EDGE_CURVE('',#11929,#11872,#6578,.T.);
#15013=EDGE_CURVE('',#11928,#11931,#6579,.T.);
#15014=EDGE_CURVE('',#11931,#11877,#6580,.T.);
#15015=EDGE_CURVE('',#11930,#11876,#6581,.T.);
#15016=EDGE_CURVE('',#11931,#11932,#6582,.T.);
#15017=EDGE_CURVE('',#11932,#11878,#6583,.T.);
#15018=EDGE_CURVE('',#11932,#11933,#6584,.T.);
#15019=EDGE_CURVE('',#11933,#11879,#6585,.T.);
#15020=EDGE_CURVE('',#11933,#11934,#6586,.T.);
#15021=EDGE_CURVE('',#11934,#11880,#6587,.T.);
#15022=EDGE_CURVE('',#11934,#11935,#6588,.T.);
#15023=EDGE_CURVE('',#11935,#11881,#6589,.T.);
#15024=EDGE_CURVE('',#11935,#11936,#6590,.T.);
#15025=EDGE_CURVE('',#11936,#11882,#6591,.T.);
#15026=EDGE_CURVE('',#11936,#11937,#10051,.T.);
#15027=EDGE_CURVE('',#11883,#11937,#6592,.T.);
#15028=EDGE_CURVE('',#11937,#11938,#6593,.T.);
#15029=EDGE_CURVE('',#11938,#11884,#6594,.T.);
#15030=EDGE_CURVE('',#11938,#11939,#10052,.T.);
#15031=EDGE_CURVE('',#11885,#11939,#6595,.T.);
#15032=EDGE_CURVE('',#11939,#11940,#6596,.T.);
#15033=EDGE_CURVE('',#11940,#11886,#6597,.T.);
#15034=EDGE_CURVE('',#11940,#11941,#10053,.T.);
#15035=EDGE_CURVE('',#11887,#11941,#6598,.T.);
#15036=EDGE_CURVE('',#11941,#11942,#10054,.T.);
#15037=EDGE_CURVE('',#11942,#11888,#6599,.T.);
#15038=EDGE_CURVE('',#11942,#11943,#10055,.T.);
#15039=EDGE_CURVE('',#11889,#11943,#6600,.T.);
#15040=EDGE_CURVE('',#11943,#11944,#6601,.T.);
#15041=EDGE_CURVE('',#11944,#11890,#6602,.T.);
#15042=EDGE_CURVE('',#11944,#11945,#10056,.T.);
#15043=EDGE_CURVE('',#11891,#11945,#6603,.T.);
#15044=EDGE_CURVE('',#11945,#11946,#6604,.T.);
#15045=EDGE_CURVE('',#11946,#11892,#6605,.T.);
#15046=EDGE_CURVE('',#11946,#11947,#10057,.T.);
#15047=EDGE_CURVE('',#11893,#11947,#6606,.T.);
#15048=EDGE_CURVE('',#11947,#11948,#6607,.T.);
#15049=EDGE_CURVE('',#11948,#11894,#6608,.T.);
#15050=EDGE_CURVE('',#11948,#11949,#10058,.T.);
#15051=EDGE_CURVE('',#11895,#11949,#6609,.T.);
#15052=EDGE_CURVE('',#11949,#11950,#10059,.T.);
#15053=EDGE_CURVE('',#11950,#11896,#6610,.T.);
#15054=EDGE_CURVE('',#11950,#11951,#10060,.T.);
#15055=EDGE_CURVE('',#11897,#11951,#6611,.T.);
#15056=EDGE_CURVE('',#11951,#11952,#6612,.T.);
#15057=EDGE_CURVE('',#11952,#11898,#6613,.T.);
#15058=EDGE_CURVE('',#11952,#11953,#6614,.T.);
#15059=EDGE_CURVE('',#11953,#11899,#6615,.T.);
#15060=EDGE_CURVE('',#11953,#11954,#6616,.T.);
#15061=EDGE_CURVE('',#11954,#11900,#6617,.T.);
#15062=EDGE_CURVE('',#11954,#11955,#10061,.T.);
#15063=EDGE_CURVE('',#11901,#11955,#6618,.T.);
#15064=EDGE_CURVE('',#11955,#11956,#10062,.T.);
#15065=EDGE_CURVE('',#11956,#11902,#6619,.T.);
#15066=EDGE_CURVE('',#11956,#11957,#10063,.T.);
#15067=EDGE_CURVE('',#11903,#11957,#6620,.T.);
#15068=EDGE_CURVE('',#11957,#11958,#6621,.T.);
#15069=EDGE_CURVE('',#11958,#11904,#6622,.T.);
#15070=EDGE_CURVE('',#11958,#11959,#10064,.T.);
#15071=EDGE_CURVE('',#11905,#11959,#6623,.T.);
#15072=EDGE_CURVE('',#11959,#11960,#6624,.T.);
#15073=EDGE_CURVE('',#11960,#11906,#6625,.T.);
#15074=EDGE_CURVE('',#11960,#11961,#10065,.T.);
#15075=EDGE_CURVE('',#11907,#11961,#6626,.T.);
#15076=EDGE_CURVE('',#11961,#11962,#6627,.T.);
#15077=EDGE_CURVE('',#11962,#11908,#6628,.T.);
#15078=EDGE_CURVE('',#11962,#11963,#10066,.T.);
#15079=EDGE_CURVE('',#11909,#11963,#6629,.T.);
#15080=EDGE_CURVE('',#11963,#11964,#10067,.T.);
#15081=EDGE_CURVE('',#11964,#11910,#6630,.T.);
#15082=EDGE_CURVE('',#11964,#11965,#10068,.T.);
#15083=EDGE_CURVE('',#11911,#11965,#6631,.T.);
#15084=EDGE_CURVE('',#11965,#11966,#6632,.T.);
#15085=EDGE_CURVE('',#11966,#11912,#6633,.T.);
#15086=EDGE_CURVE('',#11966,#11967,#10069,.T.);
#15087=EDGE_CURVE('',#11913,#11967,#6634,.T.);
#15088=EDGE_CURVE('',#11967,#11968,#6635,.T.);
#15089=EDGE_CURVE('',#11968,#11914,#6636,.T.);
#15090=EDGE_CURVE('',#11968,#11969,#10070,.T.);
#15091=EDGE_CURVE('',#11915,#11969,#6637,.T.);
#15092=EDGE_CURVE('',#11969,#11924,#6638,.T.);
#15093=EDGE_CURVE('',#11970,#11971,#6639,.T.);
#15094=EDGE_CURVE('',#11971,#11972,#6640,.T.);
#15095=EDGE_CURVE('',#11972,#11973,#6641,.T.);
#15096=EDGE_CURVE('',#11973,#11970,#6642,.T.);
#15097=EDGE_CURVE('',#11974,#11975,#6643,.T.);
#15098=EDGE_CURVE('',#11975,#11976,#6644,.T.);
#15099=EDGE_CURVE('',#11976,#11977,#6645,.T.);
#15100=EDGE_CURVE('',#11974,#11977,#6646,.T.);
#15101=EDGE_CURVE('',#11978,#11654,#6647,.T.);
#15102=EDGE_CURVE('',#11923,#11978,#6648,.T.);
#15103=EDGE_CURVE('',#11655,#11979,#6649,.T.);
#15104=EDGE_CURVE('',#11922,#11979,#6650,.T.);
#15105=EDGE_CURVE('',#11979,#11978,#10071,.T.);
#15106=EDGE_CURVE('',#11971,#11980,#10072,.T.);
#15107=EDGE_CURVE('',#11981,#11970,#10073,.T.);
#15108=EDGE_CURVE('',#11980,#11981,#6651,.T.);
#15109=EDGE_CURVE('',#11982,#11980,#6652,.T.);
#15110=EDGE_CURVE('',#11982,#11983,#6653,.T.);
#15111=EDGE_CURVE('',#11983,#11984,#6654,.T.);
#15112=EDGE_CURVE('',#11972,#11984,#6655,.T.);
#15113=EDGE_CURVE('',#11982,#11985,#6656,.T.);
#15114=EDGE_CURVE('',#11985,#11986,#6657,.T.);
#15115=EDGE_CURVE('',#11983,#11986,#6658,.T.);
#15116=EDGE_CURVE('',#11987,#11988,#6659,.T.);
#15117=EDGE_CURVE('',#11988,#11989,#6660,.T.);
#15118=EDGE_CURVE('',#11989,#11990,#6661,.T.);
#15119=EDGE_CURVE('',#11987,#11990,#6662,.T.);
#15120=EDGE_CURVE('',#11991,#11990,#6663,.T.);
#15121=EDGE_CURVE('',#11991,#11976,#10074,.T.);
#15122=EDGE_CURVE('',#11992,#11975,#6664,.T.);
#15123=EDGE_CURVE('',#11992,#11987,#6665,.T.);
#15124=EDGE_CURVE('',#11993,#11991,#6666,.T.);
#15125=EDGE_CURVE('',#11993,#11977,#10075,.T.);
#15126=EDGE_CURVE('',#11994,#11995,#6667,.T.);
#15127=EDGE_CURVE('',#11995,#11996,#6668,.T.);
#15128=EDGE_CURVE('',#11996,#11997,#6669,.T.);
#15129=EDGE_CURVE('',#11997,#11998,#6670,.T.);
#15130=EDGE_CURVE('',#11998,#11999,#6671,.T.);
#15131=EDGE_CURVE('',#11999,#12000,#6672,.T.);
#15132=EDGE_CURVE('',#12000,#12001,#6673,.T.);
#15133=EDGE_CURVE('',#12001,#12002,#6674,.T.);
#15134=EDGE_CURVE('',#12002,#12003,#6675,.T.);
#15135=EDGE_CURVE('',#12003,#12004,#6676,.T.);
#15136=EDGE_CURVE('',#12004,#12005,#10076,.T.);
#15137=EDGE_CURVE('',#12005,#12006,#6677,.T.);
#15138=EDGE_CURVE('',#12006,#12007,#10077,.T.);
#15139=EDGE_CURVE('',#12007,#12008,#6678,.T.);
#15140=EDGE_CURVE('',#12008,#12009,#10078,.T.);
#15141=EDGE_CURVE('',#12009,#12010,#10079,.T.);
#15142=EDGE_CURVE('',#12010,#12011,#10080,.T.);
#15143=EDGE_CURVE('',#12011,#12012,#6679,.T.);
#15144=EDGE_CURVE('',#12012,#12013,#10081,.T.);
#15145=EDGE_CURVE('',#12013,#12014,#6680,.T.);
#15146=EDGE_CURVE('',#12014,#12015,#10082,.T.);
#15147=EDGE_CURVE('',#12015,#12016,#6681,.T.);
#15148=EDGE_CURVE('',#12016,#12017,#10083,.T.);
#15149=EDGE_CURVE('',#12017,#12018,#10084,.T.);
#15150=EDGE_CURVE('',#12018,#12019,#10085,.T.);
#15151=EDGE_CURVE('',#12019,#12020,#6682,.T.);
#15152=EDGE_CURVE('',#12020,#12021,#6683,.T.);
#15153=EDGE_CURVE('',#12021,#12022,#6684,.T.);
#15154=EDGE_CURVE('',#12022,#12023,#10086,.T.);
#15155=EDGE_CURVE('',#12023,#12024,#10087,.T.);
#15156=EDGE_CURVE('',#12024,#12025,#10088,.T.);
#15157=EDGE_CURVE('',#12025,#12026,#6685,.T.);
#15158=EDGE_CURVE('',#12026,#12027,#10089,.T.);
#15159=EDGE_CURVE('',#12027,#12028,#6686,.T.);
#15160=EDGE_CURVE('',#12028,#12029,#10090,.T.);
#15161=EDGE_CURVE('',#12029,#12030,#6687,.T.);
#15162=EDGE_CURVE('',#12030,#12031,#10091,.T.);
#15163=EDGE_CURVE('',#12031,#12032,#10092,.T.);
#15164=EDGE_CURVE('',#12032,#12033,#10093,.T.);
#15165=EDGE_CURVE('',#12033,#12034,#6688,.T.);
#15166=EDGE_CURVE('',#12034,#12035,#10094,.T.);
#15167=EDGE_CURVE('',#12035,#12036,#6689,.T.);
#15168=EDGE_CURVE('',#12036,#12037,#10095,.T.);
#15169=EDGE_CURVE('',#12037,#11994,#6690,.T.);
#15170=EDGE_CURVE('',#11992,#12038,#6691,.T.);
#15171=EDGE_CURVE('',#12038,#11974,#6692,.T.);
#15172=EDGE_CURVE('',#12039,#11984,#6693,.T.);
#15173=EDGE_CURVE('',#12039,#11973,#6694,.T.);
#15174=EDGE_CURVE('',#12040,#12041,#6695,.T.);
#15175=EDGE_CURVE('',#11981,#12041,#6696,.T.);
#15176=EDGE_CURVE('',#12039,#12040,#6697,.T.);
#15177=EDGE_CURVE('',#12040,#12042,#6698,.T.);
#15178=EDGE_CURVE('',#12042,#12043,#6699,.T.);
#15179=EDGE_CURVE('',#12043,#12041,#6700,.T.);
#15180=EDGE_CURVE('',#12044,#12038,#6701,.T.);
#15181=EDGE_CURVE('',#11993,#12045,#6702,.T.);
#15182=EDGE_CURVE('',#12045,#12044,#6703,.T.);
#15183=EDGE_CURVE('',#12045,#12046,#6704,.T.);
#15184=EDGE_CURVE('',#12046,#12047,#6705,.T.);
#15185=EDGE_CURVE('',#12044,#12047,#6706,.T.);
#15186=EDGE_CURVE('',#11682,#12043,#152,.T.);
#15187=EDGE_CURVE('',#11985,#11684,#153,.T.);
#15188=EDGE_CURVE('',#12048,#11988,#10096,.T.);
#15189=EDGE_CURVE('',#12049,#11992,#6707,.T.);
#15190=EDGE_CURVE('',#12049,#12050,#6708,.T.);
#15191=EDGE_CURVE('',#12048,#12050,#6709,.T.);
#15192=EDGE_CURVE('',#12051,#12052,#6710,.T.);
#15193=EDGE_CURVE('',#12052,#12048,#6711,.T.);
#15194=EDGE_CURVE('',#12050,#12051,#6712,.T.);
#15195=EDGE_CURVE('',#11685,#12053,#154,.T.);
#15196=EDGE_CURVE('',#12054,#11687,#6713,.T.);
#15197=EDGE_CURVE('',#12053,#12054,#6714,.T.);
#15198=EDGE_CURVE('',#12055,#12056,#6715,.T.);
#15199=EDGE_CURVE('',#12055,#12053,#6716,.T.);
#15200=EDGE_CURVE('',#12054,#12056,#6717,.T.);
#15201=EDGE_CURVE('',#12056,#12057,#6718,.T.);
#15202=EDGE_CURVE('',#11984,#12057,#6719,.T.);
#15203=EDGE_CURVE('',#11986,#12055,#10097,.T.);
#15204=EDGE_CURVE('',#12052,#12058,#155,.T.);
#15205=EDGE_CURVE('',#12059,#12051,#6720,.T.);
#15206=EDGE_CURVE('',#12058,#12059,#6721,.T.);
#15207=EDGE_CURVE('',#12046,#11678,#156,.T.);
#15208=EDGE_CURVE('',#11679,#11989,#157,.T.);
#15209=EDGE_CURVE('',#12060,#12061,#6722,.T.);
#15210=EDGE_CURVE('',#11995,#12061,#6723,.T.);
#15211=EDGE_CURVE('',#11994,#12060,#6724,.T.);
#15212=EDGE_CURVE('',#12061,#12062,#6725,.T.);
#15213=EDGE_CURVE('',#11996,#12062,#6726,.T.);
#15214=EDGE_CURVE('',#12062,#12063,#6727,.T.);
#15215=EDGE_CURVE('',#11997,#12063,#6728,.T.);
#15216=EDGE_CURVE('',#12063,#12064,#6729,.T.);
#15217=EDGE_CURVE('',#11998,#12064,#6730,.T.);
#15218=EDGE_CURVE('',#12064,#12065,#6731,.T.);
#15219=EDGE_CURVE('',#11999,#12065,#6732,.T.);
#15220=EDGE_CURVE('',#12065,#12066,#6733,.T.);
#15221=EDGE_CURVE('',#12000,#12066,#6734,.T.);
#15222=EDGE_CURVE('',#12066,#12067,#6735,.T.);
#15223=EDGE_CURVE('',#12001,#12067,#6736,.T.);
#15224=EDGE_CURVE('',#12067,#12068,#6737,.T.);
#15225=EDGE_CURVE('',#12002,#12068,#6738,.T.);
#15226=EDGE_CURVE('',#12068,#12069,#6739,.T.);
#15227=EDGE_CURVE('',#12003,#12069,#6740,.T.);
#15228=EDGE_CURVE('',#12069,#12070,#6741,.T.);
#15229=EDGE_CURVE('',#12004,#12070,#6742,.T.);
#15230=EDGE_CURVE('',#12070,#12071,#10098,.T.);
#15231=EDGE_CURVE('',#12005,#12071,#6743,.T.);
#15232=EDGE_CURVE('',#12071,#12072,#6744,.T.);
#15233=EDGE_CURVE('',#12006,#12072,#6745,.T.);
#15234=EDGE_CURVE('',#12072,#12073,#10099,.T.);
#15235=EDGE_CURVE('',#12007,#12073,#6746,.T.);
#15236=EDGE_CURVE('',#12073,#12074,#6747,.T.);
#15237=EDGE_CURVE('',#12008,#12074,#6748,.T.);
#15238=EDGE_CURVE('',#12074,#12075,#10100,.T.);
#15239=EDGE_CURVE('',#12009,#12075,#6749,.T.);
#15240=EDGE_CURVE('',#12075,#12076,#10101,.T.);
#15241=EDGE_CURVE('',#12010,#12076,#6750,.T.);
#15242=EDGE_CURVE('',#12076,#12077,#10102,.T.);
#15243=EDGE_CURVE('',#12011,#12077,#6751,.T.);
#15244=EDGE_CURVE('',#12077,#12078,#6752,.T.);
#15245=EDGE_CURVE('',#12012,#12078,#6753,.T.);
#15246=EDGE_CURVE('',#12078,#12079,#10103,.T.);
#15247=EDGE_CURVE('',#12013,#12079,#6754,.T.);
#15248=EDGE_CURVE('',#12079,#12080,#6755,.T.);
#15249=EDGE_CURVE('',#12014,#12080,#6756,.T.);
#15250=EDGE_CURVE('',#12080,#12081,#10104,.T.);
#15251=EDGE_CURVE('',#12015,#12081,#6757,.T.);
#15252=EDGE_CURVE('',#12081,#12082,#6758,.T.);
#15253=EDGE_CURVE('',#12016,#12082,#6759,.T.);
#15254=EDGE_CURVE('',#12082,#12083,#10105,.T.);
#15255=EDGE_CURVE('',#12017,#12083,#6760,.T.);
#15256=EDGE_CURVE('',#12083,#12084,#10106,.T.);
#15257=EDGE_CURVE('',#12018,#12084,#6761,.T.);
#15258=EDGE_CURVE('',#12084,#12085,#10107,.T.);
#15259=EDGE_CURVE('',#12019,#12085,#6762,.T.);
#15260=EDGE_CURVE('',#12085,#12086,#6763,.T.);
#15261=EDGE_CURVE('',#12020,#12086,#6764,.T.);
#15262=EDGE_CURVE('',#12086,#12087,#6765,.T.);
#15263=EDGE_CURVE('',#12021,#12087,#6766,.T.);
#15264=EDGE_CURVE('',#12087,#12088,#6767,.T.);
#15265=EDGE_CURVE('',#12022,#12088,#6768,.T.);
#15266=EDGE_CURVE('',#12088,#12089,#10108,.T.);
#15267=EDGE_CURVE('',#12023,#12089,#6769,.T.);
#15268=EDGE_CURVE('',#12089,#12090,#10109,.T.);
#15269=EDGE_CURVE('',#12024,#12090,#6770,.T.);
#15270=EDGE_CURVE('',#12090,#12091,#10110,.T.);
#15271=EDGE_CURVE('',#12025,#12091,#6771,.T.);
#15272=EDGE_CURVE('',#12091,#12092,#6772,.T.);
#15273=EDGE_CURVE('',#12026,#12092,#6773,.T.);
#15274=EDGE_CURVE('',#12092,#12093,#10111,.T.);
#15275=EDGE_CURVE('',#12027,#12093,#6774,.T.);
#15276=EDGE_CURVE('',#12093,#12094,#6775,.T.);
#15277=EDGE_CURVE('',#12028,#12094,#6776,.T.);
#15278=EDGE_CURVE('',#12094,#12095,#10112,.T.);
#15279=EDGE_CURVE('',#12029,#12095,#6777,.T.);
#15280=EDGE_CURVE('',#12095,#12096,#6778,.T.);
#15281=EDGE_CURVE('',#12030,#12096,#6779,.T.);
#15282=EDGE_CURVE('',#12096,#12097,#10113,.T.);
#15283=EDGE_CURVE('',#12031,#12097,#6780,.T.);
#15284=EDGE_CURVE('',#12097,#12098,#10114,.T.);
#15285=EDGE_CURVE('',#12032,#12098,#6781,.T.);
#15286=EDGE_CURVE('',#12098,#12099,#10115,.T.);
#15287=EDGE_CURVE('',#12033,#12099,#6782,.T.);
#15288=EDGE_CURVE('',#12099,#12100,#6783,.T.);
#15289=EDGE_CURVE('',#12034,#12100,#6784,.T.);
#15290=EDGE_CURVE('',#12100,#12101,#10116,.T.);
#15291=EDGE_CURVE('',#12035,#12101,#6785,.T.);
#15292=EDGE_CURVE('',#12101,#12102,#6786,.T.);
#15293=EDGE_CURVE('',#12036,#12102,#6787,.T.);
#15294=EDGE_CURVE('',#12102,#12103,#10117,.T.);
#15295=EDGE_CURVE('',#12037,#12103,#6788,.T.);
#15296=EDGE_CURVE('',#12103,#12060,#6789,.T.);
#15297=EDGE_CURVE('',#12104,#12105,#6790,.T.);
#15298=EDGE_CURVE('',#12105,#12106,#6791,.T.);
#15299=EDGE_CURVE('',#12106,#12107,#6792,.T.);
#15300=EDGE_CURVE('',#12107,#12104,#6793,.T.);
#15301=EDGE_CURVE('',#12108,#12105,#6794,.T.);
#15302=EDGE_CURVE('',#12108,#12109,#6795,.T.);
#15303=EDGE_CURVE('',#12106,#12109,#6796,.T.);
#15304=EDGE_CURVE('',#12110,#12108,#6797,.T.);
#15305=EDGE_CURVE('',#12111,#12110,#6798,.T.);
#15306=EDGE_CURVE('',#12109,#12111,#6799,.T.);
#15307=EDGE_CURVE('',#12112,#12110,#6800,.T.);
#15308=EDGE_CURVE('',#12113,#12112,#6801,.T.);
#15309=EDGE_CURVE('',#12111,#12113,#6802,.T.);
#15310=EDGE_CURVE('',#12114,#12112,#6803,.T.);
#15311=EDGE_CURVE('',#12115,#12114,#6804,.T.);
#15312=EDGE_CURVE('',#12113,#12115,#6805,.T.);
#15313=EDGE_CURVE('',#12116,#12117,#6806,.T.);
#15314=EDGE_CURVE('',#12118,#12116,#6807,.T.);
#15315=EDGE_CURVE('',#12119,#12118,#6808,.T.);
#15316=EDGE_CURVE('',#12119,#12117,#6809,.T.);
#15317=EDGE_CURVE('',#12120,#12116,#6810,.T.);
#15318=EDGE_CURVE('',#12121,#12120,#6811,.T.);
#15319=EDGE_CURVE('',#12118,#12121,#6812,.T.);
#15320=EDGE_CURVE('',#12122,#12120,#6813,.T.);
#15321=EDGE_CURVE('',#12123,#12122,#6814,.T.);
#15322=EDGE_CURVE('',#12121,#12123,#6815,.T.);
#15323=EDGE_CURVE('',#12123,#12107,#6816,.T.);
#15324=EDGE_CURVE('',#12104,#12122,#6817,.T.);
#15325=EDGE_CURVE('',#12049,#12124,#6818,.T.);
#15326=EDGE_CURVE('',#12038,#12125,#6819,.T.);
#15327=EDGE_CURVE('',#12125,#12126,#6820,.T.);
#15328=EDGE_CURVE('',#12126,#12124,#6821,.T.);
#15329=EDGE_CURVE('',#12126,#12127,#6822,.T.);
#15330=EDGE_CURVE('',#12127,#12128,#6823,.T.);
#15331=EDGE_CURVE('',#12124,#12128,#6824,.T.);
#15332=EDGE_CURVE('',#12129,#12130,#6825,.T.);
#15333=EDGE_CURVE('',#12128,#12130,#6826,.T.);
#15334=EDGE_CURVE('',#12127,#12129,#6827,.T.);
#15335=EDGE_CURVE('',#12131,#12132,#6828,.T.);
#15336=EDGE_CURVE('',#12132,#12130,#6829,.T.);
#15337=EDGE_CURVE('',#12131,#12129,#6830,.T.);
#15338=EDGE_CURVE('',#12133,#12134,#6831,.T.);
#15339=EDGE_CURVE('',#12134,#12132,#6832,.T.);
#15340=EDGE_CURVE('',#12133,#12131,#6833,.T.);
#15341=EDGE_CURVE('',#12135,#12136,#6834,.T.);
#15342=EDGE_CURVE('',#12136,#12134,#6835,.T.);
#15343=EDGE_CURVE('',#12135,#12133,#6836,.T.);
#15344=EDGE_CURVE('',#12135,#12137,#6837,.T.);
#15345=EDGE_CURVE('',#12137,#12138,#6838,.T.);
#15346=EDGE_CURVE('',#12136,#12138,#6839,.T.);
#15347=EDGE_CURVE('',#12139,#12140,#6840,.T.);
#15348=EDGE_CURVE('',#12140,#12138,#6841,.T.);
#15349=EDGE_CURVE('',#12139,#12137,#6842,.T.);
#15350=EDGE_CURVE('',#12141,#12142,#6843,.T.);
#15351=EDGE_CURVE('',#12142,#12140,#6844,.T.);
#15352=EDGE_CURVE('',#12141,#12139,#6845,.T.);
#15353=EDGE_CURVE('',#12143,#12144,#6846,.T.);
#15354=EDGE_CURVE('',#12144,#12142,#6847,.T.);
#15355=EDGE_CURVE('',#12143,#12141,#6848,.T.);
#15356=EDGE_CURVE('',#12143,#12145,#6849,.T.);
#15357=EDGE_CURVE('',#12145,#12146,#6850,.T.);
#15358=EDGE_CURVE('',#12144,#12146,#6851,.T.);
#15359=EDGE_CURVE('',#12145,#12147,#6852,.T.);
#15360=EDGE_CURVE('',#12147,#12148,#6853,.T.);
#15361=EDGE_CURVE('',#12146,#12148,#6854,.T.);
#15362=EDGE_CURVE('',#12147,#12149,#6855,.T.);
#15363=EDGE_CURVE('',#12149,#12150,#6856,.T.);
#15364=EDGE_CURVE('',#12148,#12150,#6857,.T.);
#15365=EDGE_CURVE('',#12149,#12151,#6858,.T.);
#15366=EDGE_CURVE('',#12151,#12152,#6859,.T.);
#15367=EDGE_CURVE('',#12150,#12152,#6860,.T.);
#15368=EDGE_CURVE('',#12151,#12153,#6861,.T.);
#15369=EDGE_CURVE('',#12153,#12039,#6862,.T.);
#15370=EDGE_CURVE('',#12152,#12057,#6863,.T.);
#15371=EDGE_CURVE('',#12154,#12042,#10118,.T.);
#15372=EDGE_CURVE('',#12153,#12155,#6864,.T.);
#15373=EDGE_CURVE('',#12154,#12155,#6865,.T.);
#15374=EDGE_CURVE('',#12156,#12157,#6866,.T.);
#15375=EDGE_CURVE('',#12157,#12154,#6867,.T.);
#15376=EDGE_CURVE('',#12155,#12156,#6868,.T.);
#15377=EDGE_CURVE('',#12157,#12158,#158,.T.);
#15378=EDGE_CURVE('',#12156,#12159,#6869,.T.);
#15379=EDGE_CURVE('',#12159,#12158,#6870,.T.);
#15380=EDGE_CURVE('',#11675,#12160,#159,.T.);
#15381=EDGE_CURVE('',#11677,#12161,#6871,.T.);
#15382=EDGE_CURVE('',#12160,#12161,#6872,.T.);
#15383=EDGE_CURVE('',#12162,#12163,#6873,.T.);
#15384=EDGE_CURVE('',#12162,#12160,#6874,.T.);
#15385=EDGE_CURVE('',#12161,#12163,#6875,.T.);
#15386=EDGE_CURVE('',#12163,#12125,#6876,.T.);
#15387=EDGE_CURVE('',#12047,#12162,#10119,.T.);
#15388=EDGE_CURVE('',#12158,#11681,#160,.T.);
#15389=EDGE_CURVE('',#12159,#12164,#6877,.T.);
#15390=EDGE_CURVE('',#12164,#11681,#6878,.T.);
#15391=EDGE_CURVE('',#12117,#12165,#6879,.T.);
#15392=EDGE_CURVE('',#12166,#12119,#6880,.T.);
#15393=EDGE_CURVE('',#12166,#12165,#6881,.T.);
#15394=EDGE_CURVE('',#12167,#12114,#6882,.T.);
#15395=EDGE_CURVE('',#12168,#12167,#6883,.T.);
#15396=EDGE_CURVE('',#12115,#12168,#6884,.T.);
#15397=EDGE_CURVE('',#11686,#12166,#6885,.T.);
#15398=EDGE_CURVE('',#12168,#12169,#6886,.T.);
#15399=EDGE_CURVE('',#12169,#12059,#6887,.T.);
#15400=EDGE_CURVE('',#12058,#11680,#161,.T.);
#15401=EDGE_CURVE('',#11680,#12169,#6888,.T.);
#15402=EDGE_CURVE('',#12165,#12170,#6889,.T.);
#15403=EDGE_CURVE('',#12170,#12171,#6890,.T.);
#15404=EDGE_CURVE('',#12171,#12172,#10120,.T.);
#15405=EDGE_CURVE('',#12172,#12173,#6891,.T.);
#15406=EDGE_CURVE('',#12173,#12174,#10121,.T.);
#15407=EDGE_CURVE('',#12174,#12175,#6892,.T.);
#15408=EDGE_CURVE('',#12175,#12176,#10122,.T.);
#15409=EDGE_CURVE('',#12176,#12177,#10123,.T.);
#15410=EDGE_CURVE('',#12177,#12178,#10124,.T.);
#15411=EDGE_CURVE('',#12178,#12179,#6893,.T.);
#15412=EDGE_CURVE('',#12179,#12180,#10125,.T.);
#15413=EDGE_CURVE('',#12180,#12181,#6894,.T.);
#15414=EDGE_CURVE('',#12181,#12182,#10126,.T.);
#15415=EDGE_CURVE('',#12182,#12183,#6895,.T.);
#15416=EDGE_CURVE('',#12183,#12184,#10127,.T.);
#15417=EDGE_CURVE('',#12184,#12185,#10128,.T.);
#15418=EDGE_CURVE('',#12185,#12186,#10129,.T.);
#15419=EDGE_CURVE('',#12186,#12187,#6896,.T.);
#15420=EDGE_CURVE('',#12187,#12188,#6897,.T.);
#15421=EDGE_CURVE('',#12188,#12189,#6898,.T.);
#15422=EDGE_CURVE('',#12189,#12190,#10130,.T.);
#15423=EDGE_CURVE('',#12190,#12191,#10131,.T.);
#15424=EDGE_CURVE('',#12191,#12192,#10132,.T.);
#15425=EDGE_CURVE('',#12192,#12193,#6899,.T.);
#15426=EDGE_CURVE('',#12193,#12194,#10133,.T.);
#15427=EDGE_CURVE('',#12194,#12195,#6900,.T.);
#15428=EDGE_CURVE('',#12195,#12196,#10134,.T.);
#15429=EDGE_CURVE('',#12196,#12197,#6901,.T.);
#15430=EDGE_CURVE('',#12197,#12198,#10135,.T.);
#15431=EDGE_CURVE('',#12198,#12199,#10136,.T.);
#15432=EDGE_CURVE('',#12199,#12200,#10137,.T.);
#15433=EDGE_CURVE('',#12200,#12201,#6902,.T.);
#15434=EDGE_CURVE('',#12201,#12202,#10138,.T.);
#15435=EDGE_CURVE('',#12202,#12203,#6903,.T.);
#15436=EDGE_CURVE('',#12203,#12204,#10139,.T.);
#15437=EDGE_CURVE('',#12204,#12205,#6904,.T.);
#15438=EDGE_CURVE('',#12205,#12167,#6905,.T.);
#15439=EDGE_CURVE('',#12206,#11676,#6906,.T.);
#15440=EDGE_CURVE('',#12207,#12206,#6907,.T.);
#15441=EDGE_CURVE('',#12208,#12207,#6908,.T.);
#15442=EDGE_CURVE('',#12209,#12208,#6909,.T.);
#15443=EDGE_CURVE('',#12210,#12209,#6910,.T.);
#15444=EDGE_CURVE('',#12210,#12211,#6911,.T.);
#15445=EDGE_CURVE('',#12212,#12211,#6912,.T.);
#15446=EDGE_CURVE('',#12212,#12213,#6913,.T.);
#15447=EDGE_CURVE('',#12214,#12213,#6914,.T.);
#15448=EDGE_CURVE('',#12215,#12214,#6915,.T.);
#15449=EDGE_CURVE('',#12216,#12215,#6916,.T.);
#15450=EDGE_CURVE('',#12217,#12216,#6917,.T.);
#15451=EDGE_CURVE('',#12164,#12217,#6918,.T.);
#15452=EDGE_CURVE('',#12218,#12219,#6919,.T.);
#15453=EDGE_CURVE('',#12218,#12213,#6920,.T.);
#15454=EDGE_CURVE('',#12219,#12212,#6921,.T.);
#15455=EDGE_CURVE('',#12220,#12221,#6922,.T.);
#15456=EDGE_CURVE('',#12221,#12209,#6923,.T.);
#15457=EDGE_CURVE('',#12220,#12208,#6924,.T.);
#15458=EDGE_CURVE('',#12222,#12220,#6925,.T.);
#15459=EDGE_CURVE('',#12222,#12207,#6926,.T.);
#15460=EDGE_CURVE('',#12223,#12222,#6927,.T.);
#15461=EDGE_CURVE('',#12223,#12206,#6928,.T.);
#15462=EDGE_CURVE('',#12221,#12224,#6929,.T.);
#15463=EDGE_CURVE('',#12210,#12224,#6930,.T.);
#15464=EDGE_CURVE('',#12225,#12203,#6931,.T.);
#15465=EDGE_CURVE('',#12225,#12226,#10140,.T.);
#15466=EDGE_CURVE('',#12204,#12226,#6932,.T.);
#15467=EDGE_CURVE('',#12227,#12201,#6933,.T.);
#15468=EDGE_CURVE('',#12227,#12228,#10141,.T.);
#15469=EDGE_CURVE('',#12202,#12228,#6934,.T.);
#15470=EDGE_CURVE('',#12228,#12225,#6935,.T.);
#15471=EDGE_CURVE('',#12226,#12229,#6936,.T.);
#15472=EDGE_CURVE('',#12229,#12205,#6937,.T.);
#15473=EDGE_CURVE('',#12229,#12223,#6938,.T.);
#15474=EDGE_CURVE('',#12230,#12231,#10142,.T.);
#15475=EDGE_CURVE('',#12200,#12231,#6939,.T.);
#15476=EDGE_CURVE('',#12230,#12199,#6940,.T.);
#15477=EDGE_CURVE('',#12232,#12233,#10143,.T.);
#15478=EDGE_CURVE('',#12198,#12233,#6941,.T.);
#15479=EDGE_CURVE('',#12232,#12197,#6942,.T.);
#15480=EDGE_CURVE('',#12233,#12230,#10144,.T.);
#15481=EDGE_CURVE('',#12234,#12235,#10145,.T.);
#15482=EDGE_CURVE('',#12196,#12235,#6943,.T.);
#15483=EDGE_CURVE('',#12234,#12195,#6944,.T.);
#15484=EDGE_CURVE('',#12236,#12237,#10146,.T.);
#15485=EDGE_CURVE('',#12194,#12237,#6945,.T.);
#15486=EDGE_CURVE('',#12236,#12193,#6946,.T.);
#15487=EDGE_CURVE('',#12237,#12234,#6947,.T.);
#15488=EDGE_CURVE('',#12235,#12232,#6948,.T.);
#15489=EDGE_CURVE('',#12238,#12239,#10147,.T.);
#15490=EDGE_CURVE('',#12192,#12239,#6949,.T.);
#15491=EDGE_CURVE('',#12238,#12191,#6950,.T.);
#15492=EDGE_CURVE('',#12240,#12241,#10148,.T.);
#15493=EDGE_CURVE('',#12190,#12241,#6951,.T.);
#15494=EDGE_CURVE('',#12240,#12189,#6952,.T.);
#15495=EDGE_CURVE('',#12241,#12238,#10149,.T.);
#15496=EDGE_CURVE('',#12242,#12187,#6953,.T.);
#15497=EDGE_CURVE('',#12242,#12243,#6954,.T.);
#15498=EDGE_CURVE('',#12243,#12188,#6955,.T.);
#15499=EDGE_CURVE('',#12243,#12240,#6956,.T.);
#15500=EDGE_CURVE('',#12244,#12245,#10150,.T.);
#15501=EDGE_CURVE('',#12186,#12245,#6957,.T.);
#15502=EDGE_CURVE('',#12244,#12185,#6958,.T.);
#15503=EDGE_CURVE('',#12246,#12247,#10151,.T.);
#15504=EDGE_CURVE('',#12184,#12247,#6959,.T.);
#15505=EDGE_CURVE('',#12246,#12183,#6960,.T.);
#15506=EDGE_CURVE('',#12247,#12244,#10152,.T.);
#15507=EDGE_CURVE('',#12248,#12249,#10153,.T.);
#15508=EDGE_CURVE('',#12182,#12249,#6961,.T.);
#15509=EDGE_CURVE('',#12248,#12181,#6962,.T.);
#15510=EDGE_CURVE('',#12250,#12251,#10154,.T.);
#15511=EDGE_CURVE('',#12180,#12251,#6963,.T.);
#15512=EDGE_CURVE('',#12250,#12179,#6964,.T.);
#15513=EDGE_CURVE('',#12251,#12248,#6965,.T.);
#15514=EDGE_CURVE('',#12249,#12246,#6966,.T.);
#15515=EDGE_CURVE('',#12245,#12242,#6967,.T.);
#15516=EDGE_CURVE('',#12252,#12253,#10155,.T.);
#15517=EDGE_CURVE('',#12178,#12253,#6968,.T.);
#15518=EDGE_CURVE('',#12252,#12177,#6969,.T.);
#15519=EDGE_CURVE('',#12254,#12255,#10156,.T.);
#15520=EDGE_CURVE('',#12176,#12255,#6970,.T.);
#15521=EDGE_CURVE('',#12254,#12175,#6971,.T.);
#15522=EDGE_CURVE('',#12255,#12252,#10157,.T.);
#15523=EDGE_CURVE('',#12256,#12173,#6972,.T.);
#15524=EDGE_CURVE('',#12256,#12257,#10158,.T.);
#15525=EDGE_CURVE('',#12174,#12257,#6973,.T.);
#15526=EDGE_CURVE('',#12258,#12171,#6974,.T.);
#15527=EDGE_CURVE('',#12258,#12259,#10159,.T.);
#15528=EDGE_CURVE('',#12172,#12259,#6975,.T.);
#15529=EDGE_CURVE('',#12260,#12261,#6976,.T.);
#15530=EDGE_CURVE('',#12261,#12217,#6977,.T.);
#15531=EDGE_CURVE('',#12260,#12216,#6978,.T.);
#15532=EDGE_CURVE('',#12262,#12260,#6979,.T.);
#15533=EDGE_CURVE('',#12262,#12215,#6980,.T.);
#15534=EDGE_CURVE('',#12263,#12262,#6981,.T.);
#15535=EDGE_CURVE('',#12263,#12214,#6982,.T.);
#15536=EDGE_CURVE('',#12218,#12263,#6983,.T.);
#15537=EDGE_CURVE('',#12261,#12264,#6984,.T.);
#15538=EDGE_CURVE('',#12264,#12170,#6985,.T.);
#15539=EDGE_CURVE('',#12264,#12258,#6986,.T.);
#15540=EDGE_CURVE('',#12259,#12256,#6987,.T.);
#15541=EDGE_CURVE('',#12257,#12254,#6988,.T.);
#15542=EDGE_CURVE('',#12253,#12250,#6989,.T.);
#15543=EDGE_CURVE('',#12239,#12236,#6990,.T.);
#15544=EDGE_CURVE('',#12231,#12227,#6991,.T.);
#15545=EDGE_CURVE('',#12265,#12224,#6992,.T.);
#15546=EDGE_CURVE('',#12211,#12265,#6993,.T.);
#15547=EDGE_CURVE('',#12265,#12219,#6994,.T.);
#15548=EDGE_CURVE('',#12266,#11929,#6995,.T.);
#15549=EDGE_CURVE('',#12266,#11874,#6996,.T.);
#15550=EDGE_CURVE('',#12267,#12266,#10160,.T.);
#15551=EDGE_CURVE('',#12267,#11875,#6997,.T.);
#15552=EDGE_CURVE('',#11930,#12267,#6998,.T.);
#15553=EDGE_CURVE('',#12268,#12268,#10161,.T.);
#15554=EDGE_CURVE('',#12268,#12269,#10162,.T.);
#15555=EDGE_CURVE('',#12269,#12269,#10163,.T.);
#15556=EDGE_CURVE('',#12269,#12270,#10164,.T.);
#15557=EDGE_CURVE('',#12270,#12270,#10165,.T.);
#15558=EDGE_CURVE('',#12270,#12271,#6999,.T.);
#15559=EDGE_CURVE('',#12271,#12271,#10166,.T.);
#15560=EDGE_CURVE('',#12272,#12272,#10167,.T.);
#15561=EDGE_CURVE('',#12273,#12274,#10168,.T.);
#15562=EDGE_CURVE('',#12275,#12274,#12,.T.);
#15563=EDGE_CURVE('',#12273,#12275,#13,.T.);
#15564=EDGE_CURVE('',#12276,#12277,#10169,.T.);
#15565=EDGE_CURVE('',#12278,#12277,#14,.T.);
#15566=EDGE_CURVE('',#12276,#12278,#15,.T.);
#15567=EDGE_CURVE('',#12279,#12280,#10170,.T.);
#15568=EDGE_CURVE('',#12281,#12279,#866,.F.);
#15569=EDGE_CURVE('',#12281,#12282,#7000,.T.);
#15570=EDGE_CURVE('',#12282,#12282,#10171,.T.);
#15571=EDGE_CURVE('',#12280,#12281,#867,.F.);
#15572=EDGE_CURVE('',#12280,#12283,#10172,.T.);
#15573=EDGE_CURVE('',#12284,#12279,#10173,.T.);
#15574=EDGE_CURVE('',#12283,#12284,#10174,.T.);
#15575=EDGE_CURVE('',#12283,#12285,#7001,.T.);
#15576=EDGE_CURVE('',#12285,#12286,#10175,.T.);
#15577=EDGE_CURVE('',#12286,#12287,#10176,.T.);
#15578=EDGE_CURVE('',#12287,#12288,#10177,.T.);
#15579=EDGE_CURVE('',#12288,#12289,#10178,.T.);
#15580=EDGE_CURVE('',#12289,#12290,#10179,.T.);
#15581=EDGE_CURVE('',#12290,#12285,#10180,.T.);
#15582=EDGE_CURVE('',#12284,#12291,#10181,.T.);
#15583=EDGE_CURVE('',#12274,#12292,#10182,.T.);
#15584=EDGE_CURVE('',#12293,#12273,#10183,.T.);
#15585=EDGE_CURVE('',#12294,#12293,#10184,.T.);
#15586=EDGE_CURVE('',#12295,#12294,#10185,.T.);
#15587=EDGE_CURVE('',#12292,#12295,#10186,.T.);
#15588=EDGE_CURVE('',#12277,#12296,#10187,.T.);
#15589=EDGE_CURVE('',#12297,#12276,#10188,.T.);
#15590=EDGE_CURVE('',#12298,#12297,#10189,.T.);
#15591=EDGE_CURVE('',#12299,#12298,#10190,.T.);
#15592=EDGE_CURVE('',#12299,#12296,#10191,.T.);
#15593=EDGE_CURVE('',#12300,#12288,#7002,.T.);
#15594=EDGE_CURVE('',#12289,#12300,#7003,.T.);
#15595=EDGE_CURVE('',#12301,#12289,#7004,.T.);
#15596=EDGE_CURVE('',#12290,#12301,#7005,.T.);
#15597=EDGE_CURVE('',#12302,#12290,#7006,.T.);
#15598=EDGE_CURVE('',#12285,#12302,#7007,.T.);
#15599=EDGE_CURVE('',#12303,#12285,#7008,.T.);
#15600=EDGE_CURVE('',#12286,#12303,#7009,.T.);
#15601=EDGE_CURVE('',#12304,#12286,#7010,.T.);
#15602=EDGE_CURVE('',#12287,#12304,#7011,.T.);
#15603=EDGE_CURVE('',#12305,#12287,#7012,.T.);
#15604=EDGE_CURVE('',#12288,#12305,#7013,.T.);
#15605=EDGE_CURVE('',#12306,#12307,#7014,.T.);
#15606=EDGE_CURVE('',#12302,#12306,#7015,.T.);
#15607=EDGE_CURVE('',#12301,#12307,#7016,.T.);
#15608=EDGE_CURVE('',#12308,#12306,#7017,.T.);
#15609=EDGE_CURVE('',#12303,#12308,#7018,.T.);
#15610=EDGE_CURVE('',#12309,#12308,#7019,.T.);
#15611=EDGE_CURVE('',#12304,#12309,#7020,.T.);
#15612=EDGE_CURVE('',#12310,#12309,#7021,.T.);
#15613=EDGE_CURVE('',#12305,#12310,#7022,.T.);
#15614=EDGE_CURVE('',#12311,#12310,#7023,.T.);
#15615=EDGE_CURVE('',#12300,#12311,#7024,.T.);
#15616=EDGE_CURVE('',#12307,#12311,#7025,.T.);
#15617=EDGE_CURVE('',#12297,#12312,#16,.T.);
#15618=EDGE_CURVE('',#12312,#12276,#17,.T.);
#15619=EDGE_CURVE('',#12298,#12313,#18,.T.);
#15620=EDGE_CURVE('',#12313,#12297,#19,.T.);
#15621=EDGE_CURVE('',#12314,#12298,#20,.T.);
#15622=EDGE_CURVE('',#12299,#12314,#21,.T.);
#15623=EDGE_CURVE('',#12315,#12299,#22,.T.);
#15624=EDGE_CURVE('',#12296,#12315,#23,.T.);
#15625=EDGE_CURVE('',#12316,#12296,#24,.T.);
#15626=EDGE_CURVE('',#12277,#12316,#25,.T.);
#15627=EDGE_CURVE('',#12317,#12292,#26,.T.);
#15628=EDGE_CURVE('',#12274,#12317,#27,.T.);
#15629=EDGE_CURVE('',#12318,#12295,#28,.T.);
#15630=EDGE_CURVE('',#12292,#12318,#29,.T.);
#15631=EDGE_CURVE('',#12319,#12294,#30,.T.);
#15632=EDGE_CURVE('',#12295,#12319,#31,.T.);
#15633=EDGE_CURVE('',#12320,#12293,#32,.T.);
#15634=EDGE_CURVE('',#12294,#12320,#33,.T.);
#15635=EDGE_CURVE('',#12321,#12273,#34,.T.);
#15636=EDGE_CURVE('',#12293,#12321,#35,.T.);
#15637=EDGE_CURVE('',#12314,#12275,#7026,.T.);
#15638=EDGE_CURVE('',#12313,#12321,#7027,.T.);
#15639=EDGE_CURVE('',#12312,#12320,#7028,.T.);
#15640=EDGE_CURVE('',#12278,#12319,#7029,.T.);
#15641=EDGE_CURVE('',#12316,#12318,#7030,.T.);
#15642=EDGE_CURVE('',#12315,#12317,#7031,.T.);
#15643=EDGE_CURVE('',#12322,#12322,#10192,.T.);
#15644=EDGE_CURVE('',#12322,#12323,#7032,.T.);
#15645=EDGE_CURVE('',#12323,#12323,#10193,.T.);
#15646=EDGE_CURVE('',#12324,#12322,#7033,.T.);
#15647=EDGE_CURVE('',#12325,#12325,#10194,.T.);
#15648=EDGE_CURVE('',#12325,#12326,#7034,.T.);
#15649=EDGE_CURVE('',#12326,#12326,#10195,.T.);
#15650=EDGE_CURVE('',#12327,#12325,#7035,.T.);
#15651=EDGE_CURVE('',#12328,#12328,#10196,.T.);
#15652=EDGE_CURVE('',#12328,#12329,#7036,.T.);
#15653=EDGE_CURVE('',#12329,#12329,#10197,.T.);
#15654=EDGE_CURVE('',#12330,#12328,#7037,.T.);
#15655=EDGE_CURVE('',#12331,#12331,#10198,.T.);
#15656=EDGE_CURVE('',#12331,#12332,#7038,.T.);
#15657=EDGE_CURVE('',#12332,#12332,#10199,.T.);
#15658=EDGE_CURVE('',#12333,#12331,#7039,.T.);
#15659=EDGE_CURVE('',#12334,#12334,#10200,.T.);
#15660=EDGE_CURVE('',#12334,#12335,#7040,.T.);
#15661=EDGE_CURVE('',#12335,#12335,#10201,.T.);
#15662=EDGE_CURVE('',#12336,#12334,#7041,.T.);
#15663=EDGE_CURVE('',#12337,#12337,#10202,.T.);
#15664=EDGE_CURVE('',#12337,#12338,#7042,.T.);
#15665=EDGE_CURVE('',#12338,#12338,#10203,.T.);
#15666=EDGE_CURVE('',#12339,#12337,#7043,.T.);
#15667=EDGE_CURVE('',#12340,#12340,#10204,.T.);
#15668=EDGE_CURVE('',#12340,#12341,#7044,.T.);
#15669=EDGE_CURVE('',#12341,#12341,#10205,.T.);
#15670=EDGE_CURVE('',#12342,#12340,#7045,.T.);
#15671=EDGE_CURVE('',#12343,#12343,#10206,.T.);
#15672=EDGE_CURVE('',#12343,#12344,#7046,.T.);
#15673=EDGE_CURVE('',#12344,#12344,#10207,.T.);
#15674=EDGE_CURVE('',#12345,#12343,#7047,.T.);
#15675=EDGE_CURVE('',#12346,#12347,#7048,.T.);
#15676=EDGE_CURVE('',#12347,#12348,#7049,.T.);
#15677=EDGE_CURVE('',#12349,#12348,#7050,.T.);
#15678=EDGE_CURVE('',#12346,#12349,#7051,.T.);
#15679=EDGE_CURVE('',#12350,#12348,#7052,.T.);
#15680=EDGE_CURVE('',#12350,#12351,#10208,.T.);
#15681=EDGE_CURVE('',#12352,#12351,#7053,.T.);
#15682=EDGE_CURVE('',#12352,#12353,#10209,.T.);
#15683=EDGE_CURVE('',#12354,#12353,#7054,.T.);
#15684=EDGE_CURVE('',#12354,#12355,#7055,.T.);
#15685=EDGE_CURVE('',#12355,#12356,#7056,.T.);
#15686=EDGE_CURVE('',#12357,#12356,#7057,.T.);
#15687=EDGE_CURVE('',#12349,#12357,#7058,.T.);
#15688=EDGE_CURVE('',#12356,#12358,#7059,.T.);
#15689=EDGE_CURVE('',#12359,#12358,#7060,.T.);
#15690=EDGE_CURVE('',#12357,#12359,#7061,.T.);
#15691=EDGE_CURVE('',#12360,#12361,#7062,.T.);
#15692=EDGE_CURVE('',#12361,#12362,#10210,.T.);
#15693=EDGE_CURVE('',#12362,#12363,#7063,.T.);
#15694=EDGE_CURVE('',#12363,#12364,#10211,.T.);
#15695=EDGE_CURVE('',#12364,#12347,#7064,.T.);
#15696=EDGE_CURVE('',#12359,#12346,#7065,.T.);
#15697=EDGE_CURVE('',#12358,#12365,#7066,.T.);
#15698=EDGE_CURVE('',#12360,#12365,#7067,.T.);
#15699=EDGE_CURVE('',#12360,#12354,#7068,.T.);
#15700=EDGE_CURVE('',#12365,#12355,#7069,.T.);
#15701=EDGE_CURVE('',#12364,#12350,#7070,.T.);
#15702=EDGE_CURVE('',#12362,#12352,#7071,.T.);
#15703=EDGE_CURVE('',#12351,#12363,#7072,.T.);
#15704=EDGE_CURVE('',#12353,#12361,#7073,.T.);
#15705=EDGE_CURVE('',#12366,#12367,#10212,.T.);
#15706=EDGE_CURVE('',#12367,#12366,#10213,.T.);
#15707=EDGE_CURVE('',#12367,#12368,#7074,.T.);
#15708=EDGE_CURVE('',#12368,#12368,#10214,.T.);
#15709=EDGE_CURVE('',#12369,#12370,#7075,.T.);
#15710=EDGE_CURVE('',#12370,#12371,#10215,.T.);
#15711=EDGE_CURVE('',#12371,#12372,#10216,.T.);
#15712=EDGE_CURVE('',#12372,#12373,#10217,.T.);
#15713=EDGE_CURVE('',#12373,#12374,#10218,.T.);
#15714=EDGE_CURVE('',#12374,#12375,#10219,.T.);
#15715=EDGE_CURVE('',#12375,#12376,#10220,.T.);
#15716=EDGE_CURVE('',#12376,#12370,#10221,.T.);
#15717=EDGE_CURVE('',#12366,#12377,#7076,.T.);
#15718=EDGE_CURVE('',#12377,#12377,#10222,.T.);
#15719=EDGE_CURVE('',#12378,#12378,#10223,.T.);
#15720=EDGE_CURVE('',#12378,#12379,#7077,.T.);
#15721=EDGE_CURVE('',#12379,#12379,#10224,.T.);
#15722=EDGE_CURVE('',#12380,#12380,#10225,.T.);
#15723=EDGE_CURVE('',#12380,#12381,#7078,.T.);
#15724=EDGE_CURVE('',#12381,#12381,#10226,.T.);
#15725=EDGE_CURVE('',#12382,#12383,#7079,.T.);
#15726=EDGE_CURVE('',#12384,#12382,#7080,.T.);
#15727=EDGE_CURVE('',#12385,#12384,#7081,.T.);
#15728=EDGE_CURVE('',#12386,#12385,#7082,.T.);
#15729=EDGE_CURVE('',#12387,#12386,#7083,.T.);
#15730=EDGE_CURVE('',#12383,#12387,#7084,.T.);
#15731=EDGE_CURVE('',#12388,#12375,#7085,.T.);
#15732=EDGE_CURVE('',#12388,#12384,#7086,.T.);
#15733=EDGE_CURVE('',#12389,#12382,#7087,.T.);
#15734=EDGE_CURVE('',#12375,#12389,#7088,.T.);
#15735=EDGE_CURVE('',#12390,#12374,#7089,.T.);
#15736=EDGE_CURVE('',#12390,#12385,#7090,.T.);
#15737=EDGE_CURVE('',#12374,#12388,#7091,.T.);
#15738=EDGE_CURVE('',#12391,#12373,#7092,.T.);
#15739=EDGE_CURVE('',#12391,#12386,#7093,.T.);
#15740=EDGE_CURVE('',#12373,#12390,#7094,.T.);
#15741=EDGE_CURVE('',#12392,#12372,#7095,.T.);
#15742=EDGE_CURVE('',#12392,#12387,#7096,.T.);
#15743=EDGE_CURVE('',#12372,#12391,#7097,.T.);
#15744=EDGE_CURVE('',#12393,#12371,#7098,.T.);
#15745=EDGE_CURVE('',#12393,#12383,#7099,.T.);
#15746=EDGE_CURVE('',#12371,#12392,#7100,.T.);
#15747=EDGE_CURVE('',#12389,#12376,#7101,.T.);
#15748=EDGE_CURVE('',#12376,#12393,#7102,.T.);
#15749=EDGE_CURVE('',#12394,#12394,#10227,.T.);
#15750=EDGE_CURVE('',#12394,#12395,#7103,.T.);
#15751=EDGE_CURVE('',#12395,#12395,#10228,.T.);
#15752=EDGE_CURVE('',#12396,#12396,#10229,.T.);
#15753=EDGE_CURVE('',#12396,#12397,#7104,.T.);
#15754=EDGE_CURVE('',#12397,#12397,#10230,.T.);
#15755=EDGE_CURVE('',#12398,#12399,#10231,.T.);
#15756=EDGE_CURVE('',#12400,#12399,#7105,.T.);
#15757=EDGE_CURVE('',#12401,#12400,#10232,.T.);
#15758=EDGE_CURVE('',#12401,#12398,#7106,.T.);
#15759=EDGE_CURVE('',#12402,#12403,#10233,.T.);
#15760=EDGE_CURVE('',#12404,#12402,#7107,.T.);
#15761=EDGE_CURVE('',#12404,#12405,#10234,.T.);
#15762=EDGE_CURVE('',#12405,#12403,#7108,.T.);
#15763=EDGE_CURVE('',#12400,#12405,#7109,.T.);
#15764=EDGE_CURVE('',#12404,#12401,#7110,.T.);
#15765=EDGE_CURVE('',#12399,#12403,#7111,.T.);
#15766=EDGE_CURVE('',#12402,#12398,#7112,.T.);
#15767=EDGE_CURVE('',#12406,#12406,#10235,.T.);
#15768=EDGE_CURVE('',#12406,#12407,#7113,.T.);
#15769=EDGE_CURVE('',#12407,#12407,#10236,.T.);
#15770=EDGE_CURVE('',#12407,#12408,#7114,.T.);
#15771=EDGE_CURVE('',#12408,#12408,#10237,.T.);
#15772=EDGE_CURVE('',#12409,#12410,#10238,.T.);
#15773=EDGE_CURVE('',#12410,#12411,#7115,.T.);
#15774=EDGE_CURVE('',#12411,#12411,#10239,.T.);
#15775=EDGE_CURVE('',#12410,#12409,#10240,.T.);
#15776=EDGE_CURVE('',#12409,#12412,#7116,.T.);
#15777=EDGE_CURVE('',#12412,#12412,#10241,.T.);
#15778=EDGE_CURVE('',#12413,#12414,#7117,.T.);
#15779=EDGE_CURVE('',#12415,#12413,#7118,.T.);
#15780=EDGE_CURVE('',#12416,#12415,#7119,.T.);
#15781=EDGE_CURVE('',#12417,#12416,#7120,.T.);
#15782=EDGE_CURVE('',#12418,#12417,#7121,.T.);
#15783=EDGE_CURVE('',#12414,#12418,#7122,.T.);
#15784=EDGE_CURVE('',#12419,#12414,#7123,.T.);
#15785=EDGE_CURVE('',#12420,#12419,#7124,.T.);
#15786=EDGE_CURVE('',#12420,#12413,#7125,.T.);
#15787=EDGE_CURVE('',#12421,#12420,#7126,.T.);
#15788=EDGE_CURVE('',#12421,#12415,#7127,.T.);
#15789=EDGE_CURVE('',#12422,#12421,#7128,.T.);
#15790=EDGE_CURVE('',#12422,#12416,#7129,.T.);
#15791=EDGE_CURVE('',#12423,#12422,#7130,.T.);
#15792=EDGE_CURVE('',#12423,#12417,#7131,.T.);
#15793=EDGE_CURVE('',#12424,#12423,#7132,.T.);
#15794=EDGE_CURVE('',#12424,#12418,#7133,.T.);
#15795=EDGE_CURVE('',#12419,#12424,#7134,.T.);
#15796=EDGE_CURVE('',#12425,#12426,#10242,.T.);
#15797=EDGE_CURVE('',#12426,#12425,#10243,.T.);
#15798=EDGE_CURVE('',#12426,#12427,#7135,.T.);
#15799=EDGE_CURVE('',#12427,#12427,#10244,.T.);
#15800=EDGE_CURVE('',#12428,#12429,#7136,.T.);
#15801=EDGE_CURVE('',#12429,#12430,#10245,.T.);
#15802=EDGE_CURVE('',#12430,#12431,#10246,.T.);
#15803=EDGE_CURVE('',#12431,#12432,#10247,.T.);
#15804=EDGE_CURVE('',#12432,#12433,#10248,.T.);
#15805=EDGE_CURVE('',#12433,#12434,#10249,.T.);
#15806=EDGE_CURVE('',#12434,#12435,#10250,.T.);
#15807=EDGE_CURVE('',#12435,#12429,#10251,.T.);
#15808=EDGE_CURVE('',#12425,#12436,#7137,.T.);
#15809=EDGE_CURVE('',#12436,#12436,#10252,.T.);
#15810=EDGE_CURVE('',#12437,#12437,#10253,.T.);
#15811=EDGE_CURVE('',#12437,#12438,#7138,.T.);
#15812=EDGE_CURVE('',#12438,#12438,#10254,.T.);
#15813=EDGE_CURVE('',#12439,#12439,#10255,.T.);
#15814=EDGE_CURVE('',#12439,#12440,#7139,.T.);
#15815=EDGE_CURVE('',#12440,#12440,#10256,.T.);
#15816=EDGE_CURVE('',#12441,#12442,#7140,.T.);
#15817=EDGE_CURVE('',#12443,#12441,#7141,.T.);
#15818=EDGE_CURVE('',#12444,#12443,#7142,.T.);
#15819=EDGE_CURVE('',#12445,#12444,#7143,.T.);
#15820=EDGE_CURVE('',#12446,#12445,#7144,.T.);
#15821=EDGE_CURVE('',#12442,#12446,#7145,.T.);
#15822=EDGE_CURVE('',#12447,#12434,#7146,.T.);
#15823=EDGE_CURVE('',#12447,#12443,#7147,.T.);
#15824=EDGE_CURVE('',#12448,#12441,#7148,.T.);
#15825=EDGE_CURVE('',#12434,#12448,#7149,.T.);
#15826=EDGE_CURVE('',#12449,#12433,#7150,.T.);
#15827=EDGE_CURVE('',#12449,#12444,#7151,.T.);
#15828=EDGE_CURVE('',#12433,#12447,#7152,.T.);
#15829=EDGE_CURVE('',#12450,#12432,#7153,.T.);
#15830=EDGE_CURVE('',#12450,#12445,#7154,.T.);
#15831=EDGE_CURVE('',#12432,#12449,#7155,.T.);
#15832=EDGE_CURVE('',#12451,#12431,#7156,.T.);
#15833=EDGE_CURVE('',#12451,#12446,#7157,.T.);
#15834=EDGE_CURVE('',#12431,#12450,#7158,.T.);
#15835=EDGE_CURVE('',#12452,#12430,#7159,.T.);
#15836=EDGE_CURVE('',#12452,#12442,#7160,.T.);
#15837=EDGE_CURVE('',#12430,#12451,#7161,.T.);
#15838=EDGE_CURVE('',#12448,#12435,#7162,.T.);
#15839=EDGE_CURVE('',#12435,#12452,#7163,.T.);
#15840=EDGE_CURVE('',#12453,#12453,#10257,.T.);
#15841=EDGE_CURVE('',#12453,#12454,#7164,.T.);
#15842=EDGE_CURVE('',#12454,#12454,#10258,.T.);
#15843=EDGE_CURVE('',#12455,#12455,#10259,.T.);
#15844=EDGE_CURVE('',#12455,#12456,#7165,.T.);
#15845=EDGE_CURVE('',#12456,#12456,#10260,.T.);
#15846=EDGE_CURVE('',#12457,#12458,#10261,.T.);
#15847=EDGE_CURVE('',#12459,#12458,#7166,.T.);
#15848=EDGE_CURVE('',#12460,#12459,#10262,.T.);
#15849=EDGE_CURVE('',#12460,#12457,#7167,.T.);
#15850=EDGE_CURVE('',#12461,#12462,#10263,.T.);
#15851=EDGE_CURVE('',#12463,#12461,#7168,.T.);
#15852=EDGE_CURVE('',#12463,#12464,#10264,.T.);
#15853=EDGE_CURVE('',#12464,#12462,#7169,.T.);
#15854=EDGE_CURVE('',#12459,#12464,#7170,.T.);
#15855=EDGE_CURVE('',#12463,#12460,#7171,.T.);
#15856=EDGE_CURVE('',#12458,#12462,#7172,.T.);
#15857=EDGE_CURVE('',#12461,#12457,#7173,.T.);
#15858=EDGE_CURVE('',#12465,#12465,#10265,.T.);
#15859=EDGE_CURVE('',#12465,#12466,#7174,.T.);
#15860=EDGE_CURVE('',#12466,#12466,#10266,.T.);
#15861=EDGE_CURVE('',#12466,#12467,#7175,.T.);
#15862=EDGE_CURVE('',#12467,#12467,#10267,.T.);
#15863=EDGE_CURVE('',#12468,#12469,#10268,.T.);
#15864=EDGE_CURVE('',#12469,#12470,#7176,.T.);
#15865=EDGE_CURVE('',#12470,#12470,#10269,.T.);
#15866=EDGE_CURVE('',#12469,#12468,#10270,.T.);
#15867=EDGE_CURVE('',#12468,#12471,#7177,.T.);
#15868=EDGE_CURVE('',#12471,#12471,#10271,.T.);
#15869=EDGE_CURVE('',#12472,#12473,#7178,.T.);
#15870=EDGE_CURVE('',#12474,#12472,#7179,.T.);
#15871=EDGE_CURVE('',#12475,#12474,#7180,.T.);
#15872=EDGE_CURVE('',#12476,#12475,#7181,.T.);
#15873=EDGE_CURVE('',#12477,#12476,#7182,.T.);
#15874=EDGE_CURVE('',#12473,#12477,#7183,.T.);
#15875=EDGE_CURVE('',#12478,#12473,#7184,.T.);
#15876=EDGE_CURVE('',#12479,#12478,#7185,.T.);
#15877=EDGE_CURVE('',#12479,#12472,#7186,.T.);
#15878=EDGE_CURVE('',#12480,#12479,#7187,.T.);
#15879=EDGE_CURVE('',#12480,#12474,#7188,.T.);
#15880=EDGE_CURVE('',#12481,#12480,#7189,.T.);
#15881=EDGE_CURVE('',#12481,#12475,#7190,.T.);
#15882=EDGE_CURVE('',#12482,#12481,#7191,.T.);
#15883=EDGE_CURVE('',#12482,#12476,#7192,.T.);
#15884=EDGE_CURVE('',#12483,#12482,#7193,.T.);
#15885=EDGE_CURVE('',#12483,#12477,#7194,.T.);
#15886=EDGE_CURVE('',#12478,#12483,#7195,.T.);
#15887=EDGE_CURVE('',#12484,#12484,#10272,.T.);
#15888=EDGE_CURVE('',#12484,#12485,#7196,.T.);
#15889=EDGE_CURVE('',#12485,#12485,#10273,.T.);
#15890=EDGE_CURVE('',#12485,#12486,#7197,.T.);
#15891=EDGE_CURVE('',#12486,#12486,#10274,.T.);
#15892=EDGE_CURVE('',#12487,#12488,#10275,.T.);
#15893=EDGE_CURVE('',#12488,#12489,#7198,.T.);
#15894=EDGE_CURVE('',#12489,#12489,#10276,.T.);
#15895=EDGE_CURVE('',#12488,#12487,#10277,.T.);
#15896=EDGE_CURVE('',#12487,#12490,#7199,.T.);
#15897=EDGE_CURVE('',#12490,#12490,#10278,.T.);
#15898=EDGE_CURVE('',#12491,#12492,#7200,.T.);
#15899=EDGE_CURVE('',#12493,#12491,#7201,.T.);
#15900=EDGE_CURVE('',#12494,#12493,#7202,.T.);
#15901=EDGE_CURVE('',#12495,#12494,#7203,.T.);
#15902=EDGE_CURVE('',#12496,#12495,#7204,.T.);
#15903=EDGE_CURVE('',#12492,#12496,#7205,.T.);
#15904=EDGE_CURVE('',#12497,#12492,#7206,.T.);
#15905=EDGE_CURVE('',#12498,#12497,#7207,.T.);
#15906=EDGE_CURVE('',#12498,#12491,#7208,.T.);
#15907=EDGE_CURVE('',#12499,#12498,#7209,.T.);
#15908=EDGE_CURVE('',#12499,#12493,#7210,.T.);
#15909=EDGE_CURVE('',#12500,#12499,#7211,.T.);
#15910=EDGE_CURVE('',#12500,#12494,#7212,.T.);
#15911=EDGE_CURVE('',#12501,#12500,#7213,.T.);
#15912=EDGE_CURVE('',#12501,#12495,#7214,.T.);
#15913=EDGE_CURVE('',#12502,#12501,#7215,.T.);
#15914=EDGE_CURVE('',#12502,#12496,#7216,.T.);
#15915=EDGE_CURVE('',#12497,#12502,#7217,.T.);
#15916=ORIENTED_EDGE('',*,*,#12503,.F.);
#15917=ORIENTED_EDGE('',*,*,#12504,.T.);
#15918=ORIENTED_EDGE('',*,*,#12505,.T.);
#15919=ORIENTED_EDGE('',*,*,#12504,.F.);
#15920=ORIENTED_EDGE('',*,*,#12506,.F.);
#15921=ORIENTED_EDGE('',*,*,#12507,.T.);
#15922=ORIENTED_EDGE('',*,*,#12508,.T.);
#15923=ORIENTED_EDGE('',*,*,#12507,.F.);
#15924=ORIENTED_EDGE('',*,*,#12509,.F.);
#15925=ORIENTED_EDGE('',*,*,#12510,.T.);
#15926=ORIENTED_EDGE('',*,*,#12511,.T.);
#15927=ORIENTED_EDGE('',*,*,#12510,.F.);
#15928=ORIENTED_EDGE('',*,*,#12512,.F.);
#15929=ORIENTED_EDGE('',*,*,#12513,.T.);
#15930=ORIENTED_EDGE('',*,*,#12514,.T.);
#15931=ORIENTED_EDGE('',*,*,#12513,.F.);
#15932=ORIENTED_EDGE('',*,*,#12515,.F.);
#15933=ORIENTED_EDGE('',*,*,#12516,.T.);
#15934=ORIENTED_EDGE('',*,*,#12517,.T.);
#15935=ORIENTED_EDGE('',*,*,#12516,.F.);
#15936=ORIENTED_EDGE('',*,*,#12518,.F.);
#15937=ORIENTED_EDGE('',*,*,#12519,.T.);
#15938=ORIENTED_EDGE('',*,*,#12520,.T.);
#15939=ORIENTED_EDGE('',*,*,#12519,.F.);
#15940=ORIENTED_EDGE('',*,*,#12521,.F.);
#15941=ORIENTED_EDGE('',*,*,#12522,.T.);
#15942=ORIENTED_EDGE('',*,*,#12523,.T.);
#15943=ORIENTED_EDGE('',*,*,#12522,.F.);
#15944=ORIENTED_EDGE('',*,*,#12524,.F.);
#15945=ORIENTED_EDGE('',*,*,#12525,.T.);
#15946=ORIENTED_EDGE('',*,*,#12526,.T.);
#15947=ORIENTED_EDGE('',*,*,#12525,.F.);
#15948=ORIENTED_EDGE('',*,*,#12527,.F.);
#15949=ORIENTED_EDGE('',*,*,#12528,.T.);
#15950=ORIENTED_EDGE('',*,*,#12529,.T.);
#15951=ORIENTED_EDGE('',*,*,#12528,.F.);
#15952=ORIENTED_EDGE('',*,*,#12530,.T.);
#15953=ORIENTED_EDGE('',*,*,#12527,.T.);
#15954=ORIENTED_EDGE('',*,*,#12530,.F.);
#15955=ORIENTED_EDGE('',*,*,#12531,.F.);
#15956=ORIENTED_EDGE('',*,*,#12532,.T.);
#15957=ORIENTED_EDGE('',*,*,#12533,.T.);
#15958=ORIENTED_EDGE('',*,*,#12532,.F.);
#15959=ORIENTED_EDGE('',*,*,#12534,.T.);
#15960=ORIENTED_EDGE('',*,*,#12531,.T.);
#15961=ORIENTED_EDGE('',*,*,#12534,.F.);
#15962=ORIENTED_EDGE('',*,*,#12535,.F.);
#15963=ORIENTED_EDGE('',*,*,#12536,.T.);
#15964=ORIENTED_EDGE('',*,*,#12537,.T.);
#15965=ORIENTED_EDGE('',*,*,#12536,.F.);
#15966=ORIENTED_EDGE('',*,*,#12538,.T.);
#15967=ORIENTED_EDGE('',*,*,#12535,.T.);
#15968=ORIENTED_EDGE('',*,*,#12538,.F.);
#15969=ORIENTED_EDGE('',*,*,#12539,.F.);
#15970=ORIENTED_EDGE('',*,*,#12540,.T.);
#15971=ORIENTED_EDGE('',*,*,#12541,.T.);
#15972=ORIENTED_EDGE('',*,*,#12540,.F.);
#15973=ORIENTED_EDGE('',*,*,#12542,.T.);
#15974=ORIENTED_EDGE('',*,*,#12539,.T.);
#15975=ORIENTED_EDGE('',*,*,#12542,.F.);
#15976=ORIENTED_EDGE('',*,*,#12543,.T.);
#15977=ORIENTED_EDGE('',*,*,#12544,.T.);
#15978=ORIENTED_EDGE('',*,*,#12545,.F.);
#15979=ORIENTED_EDGE('',*,*,#12546,.T.);
#15980=ORIENTED_EDGE('',*,*,#12547,.T.);
#15981=ORIENTED_EDGE('',*,*,#12548,.F.);
#15982=ORIENTED_EDGE('',*,*,#12549,.F.);
#15983=ORIENTED_EDGE('',*,*,#12550,.T.);
#15984=ORIENTED_EDGE('',*,*,#12551,.T.);
#15985=ORIENTED_EDGE('',*,*,#12552,.F.);
#15986=ORIENTED_EDGE('',*,*,#12553,.F.);
#15987=ORIENTED_EDGE('',*,*,#12548,.T.);
#15988=ORIENTED_EDGE('',*,*,#12529,.F.);
#15989=ORIENTED_EDGE('',*,*,#12533,.F.);
#15990=ORIENTED_EDGE('',*,*,#12537,.F.);
#15991=ORIENTED_EDGE('',*,*,#12541,.F.);
#15992=ORIENTED_EDGE('',*,*,#12554,.T.);
#15993=ORIENTED_EDGE('',*,*,#12546,.F.);
#15994=ORIENTED_EDGE('',*,*,#12555,.F.);
#15995=ORIENTED_EDGE('',*,*,#12552,.T.);
#15996=ORIENTED_EDGE('',*,*,#12556,.F.);
#15997=ORIENTED_EDGE('',*,*,#12557,.F.);
#15998=ORIENTED_EDGE('',*,*,#12558,.T.);
#15999=ORIENTED_EDGE('',*,*,#12550,.F.);
#16000=ORIENTED_EDGE('',*,*,#12545,.T.);
#16001=ORIENTED_EDGE('',*,*,#12559,.F.);
#16002=ORIENTED_EDGE('',*,*,#12560,.F.);
#16003=ORIENTED_EDGE('',*,*,#12561,.F.);
#16004=ORIENTED_EDGE('',*,*,#12556,.T.);
#16005=ORIENTED_EDGE('',*,*,#12549,.T.);
#16006=ORIENTED_EDGE('',*,*,#12553,.T.);
#16007=ORIENTED_EDGE('',*,*,#12555,.T.);
#16008=ORIENTED_EDGE('',*,*,#12505,.F.);
#16009=ORIENTED_EDGE('',*,*,#12508,.F.);
#16010=ORIENTED_EDGE('',*,*,#12511,.F.);
#16011=ORIENTED_EDGE('',*,*,#12514,.F.);
#16012=ORIENTED_EDGE('',*,*,#12517,.F.);
#16013=ORIENTED_EDGE('',*,*,#12520,.F.);
#16014=ORIENTED_EDGE('',*,*,#12523,.F.);
#16015=ORIENTED_EDGE('',*,*,#12526,.F.);
#16016=ORIENTED_EDGE('',*,*,#12562,.T.);
#16017=ORIENTED_EDGE('',*,*,#12543,.F.);
#16018=ORIENTED_EDGE('',*,*,#12554,.F.);
#16019=ORIENTED_EDGE('',*,*,#12551,.F.);
#16020=ORIENTED_EDGE('',*,*,#12547,.F.);
#16021=ORIENTED_EDGE('',*,*,#12558,.F.);
#16022=ORIENTED_EDGE('',*,*,#12563,.T.);
#16023=ORIENTED_EDGE('',*,*,#12564,.T.);
#16024=ORIENTED_EDGE('',*,*,#12503,.T.);
#16025=ORIENTED_EDGE('',*,*,#12506,.T.);
#16026=ORIENTED_EDGE('',*,*,#12509,.T.);
#16027=ORIENTED_EDGE('',*,*,#12512,.T.);
#16028=ORIENTED_EDGE('',*,*,#12515,.T.);
#16029=ORIENTED_EDGE('',*,*,#12518,.T.);
#16030=ORIENTED_EDGE('',*,*,#12521,.T.);
#16031=ORIENTED_EDGE('',*,*,#12524,.T.);
#16032=ORIENTED_EDGE('',*,*,#12559,.T.);
#16033=ORIENTED_EDGE('',*,*,#12544,.F.);
#16034=ORIENTED_EDGE('',*,*,#12562,.F.);
#16035=ORIENTED_EDGE('',*,*,#12565,.T.);
#16036=ORIENTED_EDGE('',*,*,#12560,.T.);
#16037=ORIENTED_EDGE('',*,*,#12565,.F.);
#16038=ORIENTED_EDGE('',*,*,#12564,.F.);
#16039=ORIENTED_EDGE('',*,*,#12566,.T.);
#16040=ORIENTED_EDGE('',*,*,#12561,.T.);
#16041=ORIENTED_EDGE('',*,*,#12566,.F.);
#16042=ORIENTED_EDGE('',*,*,#12563,.F.);
#16043=ORIENTED_EDGE('',*,*,#12557,.T.);
#16044=ORIENTED_EDGE('',*,*,#12567,.F.);
#16045=ORIENTED_EDGE('',*,*,#12568,.T.);
#16046=ORIENTED_EDGE('',*,*,#12569,.T.);
#16047=ORIENTED_EDGE('',*,*,#12570,.T.);
#16048=ORIENTED_EDGE('',*,*,#12571,.T.);
#16049=ORIENTED_EDGE('',*,*,#12572,.T.);
#16050=ORIENTED_EDGE('',*,*,#12573,.T.);
#16051=ORIENTED_EDGE('',*,*,#12568,.F.);
#16052=ORIENTED_EDGE('',*,*,#12574,.F.);
#16053=ORIENTED_EDGE('',*,*,#12575,.T.);
#16054=ORIENTED_EDGE('',*,*,#12567,.T.);
#16055=ORIENTED_EDGE('',*,*,#12575,.F.);
#16056=ORIENTED_EDGE('',*,*,#12576,.F.);
#16057=ORIENTED_EDGE('',*,*,#12577,.T.);
#16058=ORIENTED_EDGE('',*,*,#12578,.T.);
#16059=ORIENTED_EDGE('',*,*,#12577,.F.);
#16060=ORIENTED_EDGE('',*,*,#12579,.F.);
#16061=ORIENTED_EDGE('',*,*,#12580,.T.);
#16062=ORIENTED_EDGE('',*,*,#12576,.T.);
#16063=ORIENTED_EDGE('',*,*,#12580,.F.);
#16064=ORIENTED_EDGE('',*,*,#12581,.F.);
#16065=ORIENTED_EDGE('',*,*,#12582,.T.);
#16066=ORIENTED_EDGE('',*,*,#12579,.T.);
#16067=ORIENTED_EDGE('',*,*,#12582,.F.);
#16068=ORIENTED_EDGE('',*,*,#12583,.F.);
#16069=ORIENTED_EDGE('',*,*,#12584,.T.);
#16070=ORIENTED_EDGE('',*,*,#12585,.T.);
#16071=ORIENTED_EDGE('',*,*,#12584,.F.);
#16072=ORIENTED_EDGE('',*,*,#12586,.F.);
#16073=ORIENTED_EDGE('',*,*,#12587,.F.);
#16074=ORIENTED_EDGE('',*,*,#12588,.T.);
#16075=ORIENTED_EDGE('',*,*,#12583,.T.);
#16076=ORIENTED_EDGE('',*,*,#12588,.F.);
#16077=ORIENTED_EDGE('',*,*,#12586,.T.);
#16078=ORIENTED_EDGE('',*,*,#12587,.T.);
#16079=ORIENTED_EDGE('',*,*,#12589,.T.);
#16080=ORIENTED_EDGE('',*,*,#12590,.F.);
#16081=ORIENTED_EDGE('',*,*,#12589,.F.);
#16082=ORIENTED_EDGE('',*,*,#12591,.F.);
#16083=ORIENTED_EDGE('',*,*,#12592,.T.);
#16084=ORIENTED_EDGE('',*,*,#12593,.T.);
#16085=ORIENTED_EDGE('',*,*,#12592,.F.);
#16086=ORIENTED_EDGE('',*,*,#12594,.F.);
#16087=ORIENTED_EDGE('',*,*,#12595,.T.);
#16088=ORIENTED_EDGE('',*,*,#12591,.T.);
#16089=ORIENTED_EDGE('',*,*,#12595,.F.);
#16090=ORIENTED_EDGE('',*,*,#12596,.F.);
#16091=ORIENTED_EDGE('',*,*,#12597,.T.);
#16092=ORIENTED_EDGE('',*,*,#12598,.T.);
#16093=ORIENTED_EDGE('',*,*,#12597,.F.);
#16094=ORIENTED_EDGE('',*,*,#12599,.F.);
#16095=ORIENTED_EDGE('',*,*,#12600,.F.);
#16096=ORIENTED_EDGE('',*,*,#12601,.T.);
#16097=ORIENTED_EDGE('',*,*,#12602,.T.);
#16098=ORIENTED_EDGE('',*,*,#12601,.F.);
#16099=ORIENTED_EDGE('',*,*,#12599,.T.);
#16100=ORIENTED_EDGE('',*,*,#12600,.T.);
#16101=ORIENTED_EDGE('',*,*,#12603,.T.);
#16102=ORIENTED_EDGE('',*,*,#12604,.F.);
#16103=ORIENTED_EDGE('',*,*,#12603,.F.);
#16104=ORIENTED_EDGE('',*,*,#12602,.F.);
#16105=ORIENTED_EDGE('',*,*,#12596,.T.);
#16106=ORIENTED_EDGE('',*,*,#12594,.T.);
#16107=ORIENTED_EDGE('',*,*,#12598,.F.);
#16108=ORIENTED_EDGE('',*,*,#12590,.T.);
#16109=ORIENTED_EDGE('',*,*,#12593,.F.);
#16110=ORIENTED_EDGE('',*,*,#12585,.F.);
#16111=ORIENTED_EDGE('',*,*,#12581,.T.);
#16112=ORIENTED_EDGE('',*,*,#12578,.F.);
#16113=ORIENTED_EDGE('',*,*,#12574,.T.);
#16114=ORIENTED_EDGE('',*,*,#12573,.F.);
#16115=ORIENTED_EDGE('',*,*,#12605,.T.);
#16116=ORIENTED_EDGE('',*,*,#12606,.T.);
#16117=ORIENTED_EDGE('',*,*,#12607,.T.);
#16118=ORIENTED_EDGE('',*,*,#12569,.F.);
#16119=ORIENTED_EDGE('',*,*,#12606,.F.);
#16120=ORIENTED_EDGE('',*,*,#12608,.F.);
#16121=ORIENTED_EDGE('',*,*,#12609,.F.);
#16122=ORIENTED_EDGE('',*,*,#12610,.T.);
#16123=ORIENTED_EDGE('',*,*,#12604,.T.);
#16124=ORIENTED_EDGE('',*,*,#12572,.F.);
#16125=ORIENTED_EDGE('',*,*,#12611,.T.);
#16126=ORIENTED_EDGE('',*,*,#12612,.T.);
#16127=ORIENTED_EDGE('',*,*,#12608,.T.);
#16128=ORIENTED_EDGE('',*,*,#12605,.F.);
#16129=ORIENTED_EDGE('',*,*,#12613,.F.);
#16130=ORIENTED_EDGE('',*,*,#12614,.T.);
#16131=ORIENTED_EDGE('',*,*,#12570,.F.);
#16132=ORIENTED_EDGE('',*,*,#12607,.F.);
#16133=ORIENTED_EDGE('',*,*,#12610,.F.);
#16134=ORIENTED_EDGE('',*,*,#12615,.T.);
#16135=ORIENTED_EDGE('',*,*,#12613,.T.);
#16136=ORIENTED_EDGE('',*,*,#12609,.T.);
#16137=ORIENTED_EDGE('',*,*,#12612,.F.);
#16138=ORIENTED_EDGE('',*,*,#12611,.F.);
#16139=ORIENTED_EDGE('',*,*,#12571,.F.);
#16140=ORIENTED_EDGE('',*,*,#12614,.F.);
#16141=ORIENTED_EDGE('',*,*,#12615,.F.);
#16142=ORIENTED_EDGE('',*,*,#12616,.F.);
#16143=ORIENTED_EDGE('',*,*,#12617,.T.);
#16144=ORIENTED_EDGE('',*,*,#12618,.F.);
#16145=ORIENTED_EDGE('',*,*,#12617,.F.);
#16146=ORIENTED_EDGE('',*,*,#12619,.F.);
#16147=ORIENTED_EDGE('',*,*,#12620,.T.);
#16148=ORIENTED_EDGE('',*,*,#12621,.T.);
#16149=ORIENTED_EDGE('',*,*,#12620,.F.);
#16150=ORIENTED_EDGE('',*,*,#12622,.F.);
#16151=ORIENTED_EDGE('',*,*,#12623,.T.);
#16152=ORIENTED_EDGE('',*,*,#12624,.T.);
#16153=ORIENTED_EDGE('',*,*,#12623,.F.);
#16154=ORIENTED_EDGE('',*,*,#12625,.F.);
#16155=ORIENTED_EDGE('',*,*,#12626,.T.);
#16156=ORIENTED_EDGE('',*,*,#12627,.T.);
#16157=ORIENTED_EDGE('',*,*,#12626,.F.);
#16158=ORIENTED_EDGE('',*,*,#12628,.F.);
#16159=ORIENTED_EDGE('',*,*,#12629,.T.);
#16160=ORIENTED_EDGE('',*,*,#12630,.T.);
#16161=ORIENTED_EDGE('',*,*,#12629,.F.);
#16162=ORIENTED_EDGE('',*,*,#12631,.F.);
#16163=ORIENTED_EDGE('',*,*,#12632,.T.);
#16164=ORIENTED_EDGE('',*,*,#12633,.T.);
#16165=ORIENTED_EDGE('',*,*,#12632,.F.);
#16166=ORIENTED_EDGE('',*,*,#12634,.F.);
#16167=ORIENTED_EDGE('',*,*,#12635,.T.);
#16168=ORIENTED_EDGE('',*,*,#12636,.T.);
#16169=ORIENTED_EDGE('',*,*,#12635,.F.);
#16170=ORIENTED_EDGE('',*,*,#12637,.F.);
#16171=ORIENTED_EDGE('',*,*,#12638,.T.);
#16172=ORIENTED_EDGE('',*,*,#12639,.T.);
#16173=ORIENTED_EDGE('',*,*,#12638,.F.);
#16174=ORIENTED_EDGE('',*,*,#12640,.F.);
#16175=ORIENTED_EDGE('',*,*,#12641,.T.);
#16176=ORIENTED_EDGE('',*,*,#12642,.T.);
#16177=ORIENTED_EDGE('',*,*,#12641,.F.);
#16178=ORIENTED_EDGE('',*,*,#12643,.F.);
#16179=ORIENTED_EDGE('',*,*,#12644,.T.);
#16180=ORIENTED_EDGE('',*,*,#12645,.T.);
#16181=ORIENTED_EDGE('',*,*,#12644,.F.);
#16182=ORIENTED_EDGE('',*,*,#12646,.F.);
#16183=ORIENTED_EDGE('',*,*,#12647,.T.);
#16184=ORIENTED_EDGE('',*,*,#12648,.T.);
#16185=ORIENTED_EDGE('',*,*,#12647,.F.);
#16186=ORIENTED_EDGE('',*,*,#12616,.T.);
#16187=ORIENTED_EDGE('',*,*,#12649,.F.);
#16188=ORIENTED_EDGE('',*,*,#12650,.T.);
#16189=ORIENTED_EDGE('',*,*,#12651,.T.);
#16190=ORIENTED_EDGE('',*,*,#12650,.F.);
#16191=ORIENTED_EDGE('',*,*,#12652,.F.);
#16192=ORIENTED_EDGE('',*,*,#12653,.T.);
#16193=ORIENTED_EDGE('',*,*,#12654,.T.);
#16194=ORIENTED_EDGE('',*,*,#12653,.F.);
#16195=ORIENTED_EDGE('',*,*,#12655,.F.);
#16196=ORIENTED_EDGE('',*,*,#12656,.T.);
#16197=ORIENTED_EDGE('',*,*,#12637,.T.);
#16198=ORIENTED_EDGE('',*,*,#12656,.F.);
#16199=ORIENTED_EDGE('',*,*,#12657,.T.);
#16200=ORIENTED_EDGE('',*,*,#12658,.F.);
#16201=ORIENTED_EDGE('',*,*,#12659,.T.);
#16202=ORIENTED_EDGE('',*,*,#12660,.F.);
#16203=ORIENTED_EDGE('',*,*,#12621,.F.);
#16204=ORIENTED_EDGE('',*,*,#12624,.F.);
#16205=ORIENTED_EDGE('',*,*,#12627,.F.);
#16206=ORIENTED_EDGE('',*,*,#12630,.F.);
#16207=ORIENTED_EDGE('',*,*,#12633,.F.);
#16208=ORIENTED_EDGE('',*,*,#12636,.F.);
#16209=ORIENTED_EDGE('',*,*,#12640,.T.);
#16210=ORIENTED_EDGE('',*,*,#12661,.F.);
#16211=ORIENTED_EDGE('',*,*,#12662,.F.);
#16212=ORIENTED_EDGE('',*,*,#12663,.F.);
#16213=ORIENTED_EDGE('',*,*,#12658,.T.);
#16214=ORIENTED_EDGE('',*,*,#12664,.F.);
#16215=ORIENTED_EDGE('',*,*,#12660,.T.);
#16216=ORIENTED_EDGE('',*,*,#12665,.F.);
#16217=ORIENTED_EDGE('',*,*,#12666,.F.);
#16218=ORIENTED_EDGE('',*,*,#12667,.F.);
#16219=ORIENTED_EDGE('',*,*,#12668,.F.);
#16220=ORIENTED_EDGE('',*,*,#12669,.F.);
#16221=ORIENTED_EDGE('',*,*,#12666,.T.);
#16222=ORIENTED_EDGE('',*,*,#12618,.T.);
#16223=ORIENTED_EDGE('',*,*,#12670,.F.);
#16224=ORIENTED_EDGE('',*,*,#12662,.T.);
#16225=ORIENTED_EDGE('',*,*,#12671,.F.);
#16226=ORIENTED_EDGE('',*,*,#12672,.F.);
#16227=ORIENTED_EDGE('',*,*,#12673,.F.);
#16228=ORIENTED_EDGE('',*,*,#12674,.F.);
#16229=ORIENTED_EDGE('',*,*,#12675,.F.);
#16230=ORIENTED_EDGE('',*,*,#12672,.T.);
#16231=ORIENTED_EDGE('',*,*,#12676,.F.);
#16232=ORIENTED_EDGE('',*,*,#12668,.T.);
#16233=ORIENTED_EDGE('',*,*,#12677,.F.);
#16234=ORIENTED_EDGE('',*,*,#12678,.F.);
#16235=ORIENTED_EDGE('',*,*,#12679,.F.);
#16236=ORIENTED_EDGE('',*,*,#12678,.T.);
#16237=ORIENTED_EDGE('',*,*,#12680,.F.);
#16238=ORIENTED_EDGE('',*,*,#12674,.T.);
#16239=ORIENTED_EDGE('',*,*,#12619,.T.);
#16240=ORIENTED_EDGE('',*,*,#12622,.T.);
#16241=ORIENTED_EDGE('',*,*,#12625,.T.);
#16242=ORIENTED_EDGE('',*,*,#12628,.T.);
#16243=ORIENTED_EDGE('',*,*,#12631,.T.);
#16244=ORIENTED_EDGE('',*,*,#12634,.T.);
#16245=ORIENTED_EDGE('',*,*,#12639,.F.);
#16246=ORIENTED_EDGE('',*,*,#12655,.T.);
#16247=ORIENTED_EDGE('',*,*,#12654,.F.);
#16248=ORIENTED_EDGE('',*,*,#12652,.T.);
#16249=ORIENTED_EDGE('',*,*,#12651,.F.);
#16250=ORIENTED_EDGE('',*,*,#12649,.T.);
#16251=ORIENTED_EDGE('',*,*,#12648,.F.);
#16252=ORIENTED_EDGE('',*,*,#12645,.F.);
#16253=ORIENTED_EDGE('',*,*,#12646,.T.);
#16254=ORIENTED_EDGE('',*,*,#12642,.F.);
#16255=ORIENTED_EDGE('',*,*,#12643,.T.);
#16256=ORIENTED_EDGE('',*,*,#12663,.T.);
#16257=ORIENTED_EDGE('',*,*,#12670,.T.);
#16258=ORIENTED_EDGE('',*,*,#12675,.T.);
#16259=ORIENTED_EDGE('',*,*,#12680,.T.);
#16260=ORIENTED_EDGE('',*,*,#12677,.T.);
#16261=ORIENTED_EDGE('',*,*,#12667,.T.);
#16262=ORIENTED_EDGE('',*,*,#12665,.T.);
#16263=ORIENTED_EDGE('',*,*,#12659,.F.);
#16264=ORIENTED_EDGE('',*,*,#12661,.T.);
#16265=ORIENTED_EDGE('',*,*,#12657,.F.);
#16266=ORIENTED_EDGE('',*,*,#12664,.T.);
#16267=ORIENTED_EDGE('',*,*,#12669,.T.);
#16268=ORIENTED_EDGE('',*,*,#12676,.T.);
#16269=ORIENTED_EDGE('',*,*,#12679,.T.);
#16270=ORIENTED_EDGE('',*,*,#12673,.T.);
#16271=ORIENTED_EDGE('',*,*,#12671,.T.);
#16272=ORIENTED_EDGE('',*,*,#12681,.F.);
#16273=ORIENTED_EDGE('',*,*,#12682,.T.);
#16274=ORIENTED_EDGE('',*,*,#12683,.T.);
#16275=ORIENTED_EDGE('',*,*,#12682,.F.);
#16276=ORIENTED_EDGE('',*,*,#12684,.F.);
#16277=ORIENTED_EDGE('',*,*,#12685,.T.);
#16278=ORIENTED_EDGE('',*,*,#12686,.T.);
#16279=ORIENTED_EDGE('',*,*,#12685,.F.);
#16280=ORIENTED_EDGE('',*,*,#12687,.F.);
#16281=ORIENTED_EDGE('',*,*,#12688,.T.);
#16282=ORIENTED_EDGE('',*,*,#12689,.T.);
#16283=ORIENTED_EDGE('',*,*,#12688,.F.);
#16284=ORIENTED_EDGE('',*,*,#12690,.F.);
#16285=ORIENTED_EDGE('',*,*,#12691,.T.);
#16286=ORIENTED_EDGE('',*,*,#12692,.T.);
#16287=ORIENTED_EDGE('',*,*,#12691,.F.);
#16288=ORIENTED_EDGE('',*,*,#12693,.F.);
#16289=ORIENTED_EDGE('',*,*,#12694,.T.);
#16290=ORIENTED_EDGE('',*,*,#12695,.T.);
#16291=ORIENTED_EDGE('',*,*,#12694,.F.);
#16292=ORIENTED_EDGE('',*,*,#12696,.F.);
#16293=ORIENTED_EDGE('',*,*,#12697,.T.);
#16294=ORIENTED_EDGE('',*,*,#12698,.T.);
#16295=ORIENTED_EDGE('',*,*,#12697,.F.);
#16296=ORIENTED_EDGE('',*,*,#12699,.F.);
#16297=ORIENTED_EDGE('',*,*,#12700,.T.);
#16298=ORIENTED_EDGE('',*,*,#12701,.T.);
#16299=ORIENTED_EDGE('',*,*,#12700,.F.);
#16300=ORIENTED_EDGE('',*,*,#12702,.T.);
#16301=ORIENTED_EDGE('',*,*,#12703,.T.);
#16302=ORIENTED_EDGE('',*,*,#12704,.T.);
#16303=ORIENTED_EDGE('',*,*,#12705,.T.);
#16304=ORIENTED_EDGE('',*,*,#12706,.T.);
#16305=ORIENTED_EDGE('',*,*,#12707,.T.);
#16306=ORIENTED_EDGE('',*,*,#12708,.T.);
#16307=ORIENTED_EDGE('',*,*,#12702,.F.);
#16308=ORIENTED_EDGE('',*,*,#12709,.T.);
#16309=ORIENTED_EDGE('',*,*,#12710,.T.);
#16310=ORIENTED_EDGE('',*,*,#12711,.T.);
#16311=ORIENTED_EDGE('',*,*,#12712,.T.);
#16312=ORIENTED_EDGE('',*,*,#12713,.T.);
#16313=ORIENTED_EDGE('',*,*,#12714,.T.);
#16314=ORIENTED_EDGE('',*,*,#12715,.T.);
#16315=ORIENTED_EDGE('',*,*,#12709,.F.);
#16316=ORIENTED_EDGE('',*,*,#12716,.T.);
#16317=ORIENTED_EDGE('',*,*,#12717,.T.);
#16318=ORIENTED_EDGE('',*,*,#12718,.T.);
#16319=ORIENTED_EDGE('',*,*,#12719,.T.);
#16320=ORIENTED_EDGE('',*,*,#12720,.T.);
#16321=ORIENTED_EDGE('',*,*,#12721,.T.);
#16322=ORIENTED_EDGE('',*,*,#12722,.T.);
#16323=ORIENTED_EDGE('',*,*,#12716,.F.);
#16324=ORIENTED_EDGE('',*,*,#12723,.T.);
#16325=ORIENTED_EDGE('',*,*,#12724,.T.);
#16326=ORIENTED_EDGE('',*,*,#12725,.T.);
#16327=ORIENTED_EDGE('',*,*,#12726,.T.);
#16328=ORIENTED_EDGE('',*,*,#12727,.T.);
#16329=ORIENTED_EDGE('',*,*,#12728,.T.);
#16330=ORIENTED_EDGE('',*,*,#12729,.T.);
#16331=ORIENTED_EDGE('',*,*,#12723,.F.);
#16332=ORIENTED_EDGE('',*,*,#12730,.T.);
#16333=ORIENTED_EDGE('',*,*,#12731,.T.);
#16334=ORIENTED_EDGE('',*,*,#12732,.F.);
#16335=ORIENTED_EDGE('',*,*,#12731,.F.);
#16336=ORIENTED_EDGE('',*,*,#12733,.T.);
#16337=ORIENTED_EDGE('',*,*,#12734,.T.);
#16338=ORIENTED_EDGE('',*,*,#12735,.F.);
#16339=ORIENTED_EDGE('',*,*,#12734,.F.);
#16340=ORIENTED_EDGE('',*,*,#12736,.T.);
#16341=ORIENTED_EDGE('',*,*,#12737,.T.);
#16342=ORIENTED_EDGE('',*,*,#12738,.F.);
#16343=ORIENTED_EDGE('',*,*,#12737,.F.);
#16344=ORIENTED_EDGE('',*,*,#12739,.T.);
#16345=ORIENTED_EDGE('',*,*,#12740,.T.);
#16346=ORIENTED_EDGE('',*,*,#12741,.F.);
#16347=ORIENTED_EDGE('',*,*,#12740,.F.);
#16348=ORIENTED_EDGE('',*,*,#12742,.T.);
#16349=ORIENTED_EDGE('',*,*,#12743,.T.);
#16350=ORIENTED_EDGE('',*,*,#12744,.T.);
#16351=ORIENTED_EDGE('',*,*,#12743,.F.);
#16352=ORIENTED_EDGE('',*,*,#12745,.T.);
#16353=ORIENTED_EDGE('',*,*,#12746,.T.);
#16354=ORIENTED_EDGE('',*,*,#12747,.T.);
#16355=ORIENTED_EDGE('',*,*,#12746,.F.);
#16356=ORIENTED_EDGE('',*,*,#12748,.T.);
#16357=ORIENTED_EDGE('',*,*,#12749,.T.);
#16358=ORIENTED_EDGE('',*,*,#12750,.T.);
#16359=ORIENTED_EDGE('',*,*,#12749,.F.);
#16360=ORIENTED_EDGE('',*,*,#12751,.T.);
#16361=ORIENTED_EDGE('',*,*,#12752,.T.);
#16362=ORIENTED_EDGE('',*,*,#12753,.T.);
#16363=ORIENTED_EDGE('',*,*,#12752,.F.);
#16364=ORIENTED_EDGE('',*,*,#12747,.F.);
#16365=ORIENTED_EDGE('',*,*,#12730,.F.);
#16366=ORIENTED_EDGE('',*,*,#12744,.F.);
#16367=ORIENTED_EDGE('',*,*,#12733,.F.);
#16368=ORIENTED_EDGE('',*,*,#12750,.F.);
#16369=ORIENTED_EDGE('',*,*,#12736,.F.);
#16370=ORIENTED_EDGE('',*,*,#12753,.F.);
#16371=ORIENTED_EDGE('',*,*,#12739,.F.);
#16372=ORIENTED_EDGE('',*,*,#12754,.T.);
#16373=ORIENTED_EDGE('',*,*,#12755,.T.);
#16374=ORIENTED_EDGE('',*,*,#12756,.T.);
#16375=ORIENTED_EDGE('',*,*,#12757,.T.);
#16376=ORIENTED_EDGE('',*,*,#12758,.T.);
#16377=ORIENTED_EDGE('',*,*,#12759,.T.);
#16378=ORIENTED_EDGE('',*,*,#12760,.T.);
#16379=ORIENTED_EDGE('',*,*,#12761,.T.);
#16380=ORIENTED_EDGE('',*,*,#12762,.T.);
#16381=ORIENTED_EDGE('',*,*,#12763,.T.);
#16382=ORIENTED_EDGE('',*,*,#12764,.T.);
#16383=ORIENTED_EDGE('',*,*,#12765,.T.);
#16384=ORIENTED_EDGE('',*,*,#12766,.F.);
#16385=ORIENTED_EDGE('',*,*,#12767,.F.);
#16386=ORIENTED_EDGE('',*,*,#12768,.F.);
#16387=ORIENTED_EDGE('',*,*,#12769,.F.);
#16388=ORIENTED_EDGE('',*,*,#12770,.F.);
#16389=ORIENTED_EDGE('',*,*,#12771,.F.);
#16390=ORIENTED_EDGE('',*,*,#12772,.F.);
#16391=ORIENTED_EDGE('',*,*,#12773,.F.);
#16392=ORIENTED_EDGE('',*,*,#12774,.T.);
#16393=ORIENTED_EDGE('',*,*,#12775,.F.);
#16394=ORIENTED_EDGE('',*,*,#12754,.F.);
#16395=ORIENTED_EDGE('',*,*,#12776,.T.);
#16396=ORIENTED_EDGE('',*,*,#12683,.F.);
#16397=ORIENTED_EDGE('',*,*,#12777,.T.);
#16398=ORIENTED_EDGE('',*,*,#12778,.F.);
#16399=ORIENTED_EDGE('',*,*,#12755,.F.);
#16400=ORIENTED_EDGE('',*,*,#12775,.T.);
#16401=ORIENTED_EDGE('',*,*,#12779,.T.);
#16402=ORIENTED_EDGE('',*,*,#12780,.F.);
#16403=ORIENTED_EDGE('',*,*,#12756,.F.);
#16404=ORIENTED_EDGE('',*,*,#12778,.T.);
#16405=ORIENTED_EDGE('',*,*,#12781,.T.);
#16406=ORIENTED_EDGE('',*,*,#12782,.F.);
#16407=ORIENTED_EDGE('',*,*,#12757,.F.);
#16408=ORIENTED_EDGE('',*,*,#12780,.T.);
#16409=ORIENTED_EDGE('',*,*,#12681,.T.);
#16410=ORIENTED_EDGE('',*,*,#12684,.T.);
#16411=ORIENTED_EDGE('',*,*,#12783,.T.);
#16412=ORIENTED_EDGE('',*,*,#12784,.F.);
#16413=ORIENTED_EDGE('',*,*,#12758,.F.);
#16414=ORIENTED_EDGE('',*,*,#12782,.T.);
#16415=ORIENTED_EDGE('',*,*,#12785,.T.);
#16416=ORIENTED_EDGE('',*,*,#12786,.F.);
#16417=ORIENTED_EDGE('',*,*,#12759,.F.);
#16418=ORIENTED_EDGE('',*,*,#12784,.T.);
#16419=ORIENTED_EDGE('',*,*,#12787,.T.);
#16420=ORIENTED_EDGE('',*,*,#12788,.F.);
#16421=ORIENTED_EDGE('',*,*,#12760,.F.);
#16422=ORIENTED_EDGE('',*,*,#12786,.T.);
#16423=ORIENTED_EDGE('',*,*,#12686,.F.);
#16424=ORIENTED_EDGE('',*,*,#12789,.T.);
#16425=ORIENTED_EDGE('',*,*,#12790,.F.);
#16426=ORIENTED_EDGE('',*,*,#12761,.F.);
#16427=ORIENTED_EDGE('',*,*,#12788,.T.);
#16428=ORIENTED_EDGE('',*,*,#12791,.T.);
#16429=ORIENTED_EDGE('',*,*,#12792,.F.);
#16430=ORIENTED_EDGE('',*,*,#12762,.F.);
#16431=ORIENTED_EDGE('',*,*,#12790,.T.);
#16432=ORIENTED_EDGE('',*,*,#12793,.T.);
#16433=ORIENTED_EDGE('',*,*,#12794,.F.);
#16434=ORIENTED_EDGE('',*,*,#12763,.F.);
#16435=ORIENTED_EDGE('',*,*,#12792,.T.);
#16436=ORIENTED_EDGE('',*,*,#12795,.T.);
#16437=ORIENTED_EDGE('',*,*,#12796,.F.);
#16438=ORIENTED_EDGE('',*,*,#12764,.F.);
#16439=ORIENTED_EDGE('',*,*,#12794,.T.);
#16440=ORIENTED_EDGE('',*,*,#12797,.T.);
#16441=ORIENTED_EDGE('',*,*,#12776,.F.);
#16442=ORIENTED_EDGE('',*,*,#12765,.F.);
#16443=ORIENTED_EDGE('',*,*,#12796,.T.);
#16444=ORIENTED_EDGE('',*,*,#12774,.F.);
#16445=ORIENTED_EDGE('',*,*,#12797,.F.);
#16446=ORIENTED_EDGE('',*,*,#12795,.F.);
#16447=ORIENTED_EDGE('',*,*,#12793,.F.);
#16448=ORIENTED_EDGE('',*,*,#12791,.F.);
#16449=ORIENTED_EDGE('',*,*,#12789,.F.);
#16450=ORIENTED_EDGE('',*,*,#12787,.F.);
#16451=ORIENTED_EDGE('',*,*,#12785,.F.);
#16452=ORIENTED_EDGE('',*,*,#12783,.F.);
#16453=ORIENTED_EDGE('',*,*,#12781,.F.);
#16454=ORIENTED_EDGE('',*,*,#12779,.F.);
#16455=ORIENTED_EDGE('',*,*,#12777,.F.);
#16456=ORIENTED_EDGE('',*,*,#12699,.T.);
#16457=ORIENTED_EDGE('',*,*,#12798,.T.);
#16458=ORIENTED_EDGE('',*,*,#12799,.T.);
#16459=ORIENTED_EDGE('',*,*,#12800,.T.);
#16460=ORIENTED_EDGE('',*,*,#12801,.T.);
#16461=ORIENTED_EDGE('',*,*,#12802,.T.);
#16462=ORIENTED_EDGE('',*,*,#12803,.T.);
#16463=ORIENTED_EDGE('',*,*,#12804,.T.);
#16464=ORIENTED_EDGE('',*,*,#12805,.T.);
#16465=ORIENTED_EDGE('',*,*,#12751,.F.);
#16466=ORIENTED_EDGE('',*,*,#12748,.F.);
#16467=ORIENTED_EDGE('',*,*,#12745,.F.);
#16468=ORIENTED_EDGE('',*,*,#12742,.F.);
#16469=ORIENTED_EDGE('',*,*,#12689,.F.);
#16470=ORIENTED_EDGE('',*,*,#12767,.T.);
#16471=ORIENTED_EDGE('',*,*,#12806,.F.);
#16472=ORIENTED_EDGE('',*,*,#12798,.F.);
#16473=ORIENTED_EDGE('',*,*,#12807,.T.);
#16474=ORIENTED_EDGE('',*,*,#12766,.T.);
#16475=ORIENTED_EDGE('',*,*,#12808,.F.);
#16476=ORIENTED_EDGE('',*,*,#12799,.F.);
#16477=ORIENTED_EDGE('',*,*,#12806,.T.);
#16478=ORIENTED_EDGE('',*,*,#12773,.T.);
#16479=ORIENTED_EDGE('',*,*,#12809,.F.);
#16480=ORIENTED_EDGE('',*,*,#12800,.F.);
#16481=ORIENTED_EDGE('',*,*,#12808,.T.);
#16482=ORIENTED_EDGE('',*,*,#12772,.T.);
#16483=ORIENTED_EDGE('',*,*,#12810,.F.);
#16484=ORIENTED_EDGE('',*,*,#12801,.F.);
#16485=ORIENTED_EDGE('',*,*,#12809,.T.);
#16486=ORIENTED_EDGE('',*,*,#12771,.T.);
#16487=ORIENTED_EDGE('',*,*,#12811,.F.);
#16488=ORIENTED_EDGE('',*,*,#12802,.F.);
#16489=ORIENTED_EDGE('',*,*,#12810,.T.);
#16490=ORIENTED_EDGE('',*,*,#12770,.T.);
#16491=ORIENTED_EDGE('',*,*,#12812,.F.);
#16492=ORIENTED_EDGE('',*,*,#12803,.F.);
#16493=ORIENTED_EDGE('',*,*,#12811,.T.);
#16494=ORIENTED_EDGE('',*,*,#12769,.T.);
#16495=ORIENTED_EDGE('',*,*,#12813,.F.);
#16496=ORIENTED_EDGE('',*,*,#12804,.F.);
#16497=ORIENTED_EDGE('',*,*,#12812,.T.);
#16498=ORIENTED_EDGE('',*,*,#12768,.T.);
#16499=ORIENTED_EDGE('',*,*,#12807,.F.);
#16500=ORIENTED_EDGE('',*,*,#12805,.F.);
#16501=ORIENTED_EDGE('',*,*,#12813,.T.);
#16502=ORIENTED_EDGE('',*,*,#12741,.T.);
#16503=ORIENTED_EDGE('',*,*,#12814,.F.);
#16504=ORIENTED_EDGE('',*,*,#12815,.F.);
#16505=ORIENTED_EDGE('',*,*,#12816,.F.);
#16506=ORIENTED_EDGE('',*,*,#12817,.F.);
#16507=ORIENTED_EDGE('',*,*,#12818,.F.);
#16508=ORIENTED_EDGE('',*,*,#12819,.F.);
#16509=ORIENTED_EDGE('',*,*,#12738,.T.);
#16510=ORIENTED_EDGE('',*,*,#12820,.F.);
#16511=ORIENTED_EDGE('',*,*,#12821,.F.);
#16512=ORIENTED_EDGE('',*,*,#12822,.F.);
#16513=ORIENTED_EDGE('',*,*,#12823,.F.);
#16514=ORIENTED_EDGE('',*,*,#12824,.F.);
#16515=ORIENTED_EDGE('',*,*,#12825,.F.);
#16516=ORIENTED_EDGE('',*,*,#12735,.T.);
#16517=ORIENTED_EDGE('',*,*,#12826,.F.);
#16518=ORIENTED_EDGE('',*,*,#12827,.F.);
#16519=ORIENTED_EDGE('',*,*,#12828,.F.);
#16520=ORIENTED_EDGE('',*,*,#12829,.F.);
#16521=ORIENTED_EDGE('',*,*,#12830,.F.);
#16522=ORIENTED_EDGE('',*,*,#12831,.F.);
#16523=ORIENTED_EDGE('',*,*,#12732,.T.);
#16524=ORIENTED_EDGE('',*,*,#12832,.F.);
#16525=ORIENTED_EDGE('',*,*,#12833,.F.);
#16526=ORIENTED_EDGE('',*,*,#12834,.F.);
#16527=ORIENTED_EDGE('',*,*,#12835,.F.);
#16528=ORIENTED_EDGE('',*,*,#12836,.F.);
#16529=ORIENTED_EDGE('',*,*,#12837,.F.);
#16530=ORIENTED_EDGE('',*,*,#12818,.T.);
#16531=ORIENTED_EDGE('',*,*,#12838,.F.);
#16532=ORIENTED_EDGE('',*,*,#12839,.F.);
#16533=ORIENTED_EDGE('',*,*,#12840,.F.);
#16534=ORIENTED_EDGE('',*,*,#12841,.T.);
#16535=ORIENTED_EDGE('',*,*,#12819,.T.);
#16536=ORIENTED_EDGE('',*,*,#12841,.F.);
#16537=ORIENTED_EDGE('',*,*,#12842,.F.);
#16538=ORIENTED_EDGE('',*,*,#12843,.F.);
#16539=ORIENTED_EDGE('',*,*,#12844,.T.);
#16540=ORIENTED_EDGE('',*,*,#12814,.T.);
#16541=ORIENTED_EDGE('',*,*,#12844,.F.);
#16542=ORIENTED_EDGE('',*,*,#12845,.F.);
#16543=ORIENTED_EDGE('',*,*,#12846,.F.);
#16544=ORIENTED_EDGE('',*,*,#12847,.T.);
#16545=ORIENTED_EDGE('',*,*,#12815,.T.);
#16546=ORIENTED_EDGE('',*,*,#12847,.F.);
#16547=ORIENTED_EDGE('',*,*,#12848,.F.);
#16548=ORIENTED_EDGE('',*,*,#12849,.F.);
#16549=ORIENTED_EDGE('',*,*,#12850,.T.);
#16550=ORIENTED_EDGE('',*,*,#12816,.T.);
#16551=ORIENTED_EDGE('',*,*,#12850,.F.);
#16552=ORIENTED_EDGE('',*,*,#12851,.F.);
#16553=ORIENTED_EDGE('',*,*,#12852,.F.);
#16554=ORIENTED_EDGE('',*,*,#12853,.T.);
#16555=ORIENTED_EDGE('',*,*,#12817,.T.);
#16556=ORIENTED_EDGE('',*,*,#12853,.F.);
#16557=ORIENTED_EDGE('',*,*,#12854,.F.);
#16558=ORIENTED_EDGE('',*,*,#12855,.F.);
#16559=ORIENTED_EDGE('',*,*,#12838,.T.);
#16560=ORIENTED_EDGE('',*,*,#12726,.F.);
#16561=ORIENTED_EDGE('',*,*,#12854,.T.);
#16562=ORIENTED_EDGE('',*,*,#12852,.T.);
#16563=ORIENTED_EDGE('',*,*,#12725,.F.);
#16564=ORIENTED_EDGE('',*,*,#12839,.T.);
#16565=ORIENTED_EDGE('',*,*,#12855,.T.);
#16566=ORIENTED_EDGE('',*,*,#12724,.F.);
#16567=ORIENTED_EDGE('',*,*,#12842,.T.);
#16568=ORIENTED_EDGE('',*,*,#12840,.T.);
#16569=ORIENTED_EDGE('',*,*,#12729,.F.);
#16570=ORIENTED_EDGE('',*,*,#12845,.T.);
#16571=ORIENTED_EDGE('',*,*,#12843,.T.);
#16572=ORIENTED_EDGE('',*,*,#12728,.F.);
#16573=ORIENTED_EDGE('',*,*,#12848,.T.);
#16574=ORIENTED_EDGE('',*,*,#12846,.T.);
#16575=ORIENTED_EDGE('',*,*,#12727,.F.);
#16576=ORIENTED_EDGE('',*,*,#12851,.T.);
#16577=ORIENTED_EDGE('',*,*,#12849,.T.);
#16578=ORIENTED_EDGE('',*,*,#12824,.T.);
#16579=ORIENTED_EDGE('',*,*,#12856,.F.);
#16580=ORIENTED_EDGE('',*,*,#12857,.F.);
#16581=ORIENTED_EDGE('',*,*,#12858,.F.);
#16582=ORIENTED_EDGE('',*,*,#12859,.T.);
#16583=ORIENTED_EDGE('',*,*,#12825,.T.);
#16584=ORIENTED_EDGE('',*,*,#12859,.F.);
#16585=ORIENTED_EDGE('',*,*,#12860,.F.);
#16586=ORIENTED_EDGE('',*,*,#12861,.F.);
#16587=ORIENTED_EDGE('',*,*,#12862,.T.);
#16588=ORIENTED_EDGE('',*,*,#12820,.T.);
#16589=ORIENTED_EDGE('',*,*,#12862,.F.);
#16590=ORIENTED_EDGE('',*,*,#12863,.F.);
#16591=ORIENTED_EDGE('',*,*,#12864,.F.);
#16592=ORIENTED_EDGE('',*,*,#12865,.T.);
#16593=ORIENTED_EDGE('',*,*,#12821,.T.);
#16594=ORIENTED_EDGE('',*,*,#12865,.F.);
#16595=ORIENTED_EDGE('',*,*,#12866,.F.);
#16596=ORIENTED_EDGE('',*,*,#12867,.F.);
#16597=ORIENTED_EDGE('',*,*,#12868,.T.);
#16598=ORIENTED_EDGE('',*,*,#12822,.T.);
#16599=ORIENTED_EDGE('',*,*,#12868,.F.);
#16600=ORIENTED_EDGE('',*,*,#12869,.F.);
#16601=ORIENTED_EDGE('',*,*,#12870,.F.);
#16602=ORIENTED_EDGE('',*,*,#12871,.T.);
#16603=ORIENTED_EDGE('',*,*,#12823,.T.);
#16604=ORIENTED_EDGE('',*,*,#12871,.F.);
#16605=ORIENTED_EDGE('',*,*,#12872,.F.);
#16606=ORIENTED_EDGE('',*,*,#12873,.F.);
#16607=ORIENTED_EDGE('',*,*,#12856,.T.);
#16608=ORIENTED_EDGE('',*,*,#12719,.F.);
#16609=ORIENTED_EDGE('',*,*,#12857,.T.);
#16610=ORIENTED_EDGE('',*,*,#12873,.T.);
#16611=ORIENTED_EDGE('',*,*,#12718,.F.);
#16612=ORIENTED_EDGE('',*,*,#12860,.T.);
#16613=ORIENTED_EDGE('',*,*,#12858,.T.);
#16614=ORIENTED_EDGE('',*,*,#12717,.F.);
#16615=ORIENTED_EDGE('',*,*,#12863,.T.);
#16616=ORIENTED_EDGE('',*,*,#12861,.T.);
#16617=ORIENTED_EDGE('',*,*,#12722,.F.);
#16618=ORIENTED_EDGE('',*,*,#12866,.T.);
#16619=ORIENTED_EDGE('',*,*,#12864,.T.);
#16620=ORIENTED_EDGE('',*,*,#12721,.F.);
#16621=ORIENTED_EDGE('',*,*,#12869,.T.);
#16622=ORIENTED_EDGE('',*,*,#12867,.T.);
#16623=ORIENTED_EDGE('',*,*,#12720,.F.);
#16624=ORIENTED_EDGE('',*,*,#12872,.T.);
#16625=ORIENTED_EDGE('',*,*,#12870,.T.);
#16626=ORIENTED_EDGE('',*,*,#12836,.T.);
#16627=ORIENTED_EDGE('',*,*,#12874,.F.);
#16628=ORIENTED_EDGE('',*,*,#12875,.F.);
#16629=ORIENTED_EDGE('',*,*,#12876,.F.);
#16630=ORIENTED_EDGE('',*,*,#12877,.T.);
#16631=ORIENTED_EDGE('',*,*,#12837,.T.);
#16632=ORIENTED_EDGE('',*,*,#12877,.F.);
#16633=ORIENTED_EDGE('',*,*,#12878,.F.);
#16634=ORIENTED_EDGE('',*,*,#12879,.F.);
#16635=ORIENTED_EDGE('',*,*,#12880,.T.);
#16636=ORIENTED_EDGE('',*,*,#12832,.T.);
#16637=ORIENTED_EDGE('',*,*,#12880,.F.);
#16638=ORIENTED_EDGE('',*,*,#12881,.F.);
#16639=ORIENTED_EDGE('',*,*,#12882,.F.);
#16640=ORIENTED_EDGE('',*,*,#12883,.T.);
#16641=ORIENTED_EDGE('',*,*,#12833,.T.);
#16642=ORIENTED_EDGE('',*,*,#12883,.F.);
#16643=ORIENTED_EDGE('',*,*,#12884,.F.);
#16644=ORIENTED_EDGE('',*,*,#12885,.F.);
#16645=ORIENTED_EDGE('',*,*,#12886,.T.);
#16646=ORIENTED_EDGE('',*,*,#12834,.T.);
#16647=ORIENTED_EDGE('',*,*,#12886,.F.);
#16648=ORIENTED_EDGE('',*,*,#12887,.F.);
#16649=ORIENTED_EDGE('',*,*,#12888,.F.);
#16650=ORIENTED_EDGE('',*,*,#12889,.T.);
#16651=ORIENTED_EDGE('',*,*,#12835,.T.);
#16652=ORIENTED_EDGE('',*,*,#12889,.F.);
#16653=ORIENTED_EDGE('',*,*,#12890,.F.);
#16654=ORIENTED_EDGE('',*,*,#12891,.F.);
#16655=ORIENTED_EDGE('',*,*,#12874,.T.);
#16656=ORIENTED_EDGE('',*,*,#12712,.F.);
#16657=ORIENTED_EDGE('',*,*,#12875,.T.);
#16658=ORIENTED_EDGE('',*,*,#12891,.T.);
#16659=ORIENTED_EDGE('',*,*,#12711,.F.);
#16660=ORIENTED_EDGE('',*,*,#12878,.T.);
#16661=ORIENTED_EDGE('',*,*,#12876,.T.);
#16662=ORIENTED_EDGE('',*,*,#12710,.F.);
#16663=ORIENTED_EDGE('',*,*,#12881,.T.);
#16664=ORIENTED_EDGE('',*,*,#12879,.T.);
#16665=ORIENTED_EDGE('',*,*,#12715,.F.);
#16666=ORIENTED_EDGE('',*,*,#12884,.T.);
#16667=ORIENTED_EDGE('',*,*,#12882,.T.);
#16668=ORIENTED_EDGE('',*,*,#12714,.F.);
#16669=ORIENTED_EDGE('',*,*,#12887,.T.);
#16670=ORIENTED_EDGE('',*,*,#12885,.T.);
#16671=ORIENTED_EDGE('',*,*,#12713,.F.);
#16672=ORIENTED_EDGE('',*,*,#12890,.T.);
#16673=ORIENTED_EDGE('',*,*,#12888,.T.);
#16674=ORIENTED_EDGE('',*,*,#12830,.T.);
#16675=ORIENTED_EDGE('',*,*,#12892,.F.);
#16676=ORIENTED_EDGE('',*,*,#12893,.F.);
#16677=ORIENTED_EDGE('',*,*,#12894,.F.);
#16678=ORIENTED_EDGE('',*,*,#12895,.T.);
#16679=ORIENTED_EDGE('',*,*,#12831,.T.);
#16680=ORIENTED_EDGE('',*,*,#12895,.F.);
#16681=ORIENTED_EDGE('',*,*,#12896,.F.);
#16682=ORIENTED_EDGE('',*,*,#12897,.F.);
#16683=ORIENTED_EDGE('',*,*,#12898,.T.);
#16684=ORIENTED_EDGE('',*,*,#12826,.T.);
#16685=ORIENTED_EDGE('',*,*,#12898,.F.);
#16686=ORIENTED_EDGE('',*,*,#12899,.F.);
#16687=ORIENTED_EDGE('',*,*,#12900,.F.);
#16688=ORIENTED_EDGE('',*,*,#12901,.T.);
#16689=ORIENTED_EDGE('',*,*,#12827,.T.);
#16690=ORIENTED_EDGE('',*,*,#12901,.F.);
#16691=ORIENTED_EDGE('',*,*,#12902,.F.);
#16692=ORIENTED_EDGE('',*,*,#12903,.F.);
#16693=ORIENTED_EDGE('',*,*,#12904,.T.);
#16694=ORIENTED_EDGE('',*,*,#12828,.T.);
#16695=ORIENTED_EDGE('',*,*,#12904,.F.);
#16696=ORIENTED_EDGE('',*,*,#12905,.F.);
#16697=ORIENTED_EDGE('',*,*,#12906,.F.);
#16698=ORIENTED_EDGE('',*,*,#12907,.T.);
#16699=ORIENTED_EDGE('',*,*,#12829,.T.);
#16700=ORIENTED_EDGE('',*,*,#12907,.F.);
#16701=ORIENTED_EDGE('',*,*,#12908,.F.);
#16702=ORIENTED_EDGE('',*,*,#12909,.F.);
#16703=ORIENTED_EDGE('',*,*,#12892,.T.);
#16704=ORIENTED_EDGE('',*,*,#12705,.F.);
#16705=ORIENTED_EDGE('',*,*,#12893,.T.);
#16706=ORIENTED_EDGE('',*,*,#12909,.T.);
#16707=ORIENTED_EDGE('',*,*,#12704,.F.);
#16708=ORIENTED_EDGE('',*,*,#12896,.T.);
#16709=ORIENTED_EDGE('',*,*,#12894,.T.);
#16710=ORIENTED_EDGE('',*,*,#12703,.F.);
#16711=ORIENTED_EDGE('',*,*,#12899,.T.);
#16712=ORIENTED_EDGE('',*,*,#12897,.T.);
#16713=ORIENTED_EDGE('',*,*,#12708,.F.);
#16714=ORIENTED_EDGE('',*,*,#12902,.T.);
#16715=ORIENTED_EDGE('',*,*,#12900,.T.);
#16716=ORIENTED_EDGE('',*,*,#12707,.F.);
#16717=ORIENTED_EDGE('',*,*,#12905,.T.);
#16718=ORIENTED_EDGE('',*,*,#12903,.T.);
#16719=ORIENTED_EDGE('',*,*,#12706,.F.);
#16720=ORIENTED_EDGE('',*,*,#12908,.T.);
#16721=ORIENTED_EDGE('',*,*,#12906,.T.);
#16722=ORIENTED_EDGE('',*,*,#12701,.F.);
#16723=ORIENTED_EDGE('',*,*,#12696,.T.);
#16724=ORIENTED_EDGE('',*,*,#12698,.F.);
#16725=ORIENTED_EDGE('',*,*,#12693,.T.);
#16726=ORIENTED_EDGE('',*,*,#12690,.T.);
#16727=ORIENTED_EDGE('',*,*,#12695,.F.);
#16728=ORIENTED_EDGE('',*,*,#12687,.T.);
#16729=ORIENTED_EDGE('',*,*,#12692,.F.);
#16730=ORIENTED_EDGE('',*,*,#12910,.F.);
#16731=ORIENTED_EDGE('',*,*,#12911,.T.);
#16732=ORIENTED_EDGE('',*,*,#12912,.F.);
#16733=ORIENTED_EDGE('',*,*,#12911,.F.);
#16734=ORIENTED_EDGE('',*,*,#12913,.T.);
#16735=ORIENTED_EDGE('',*,*,#12914,.T.);
#16736=ORIENTED_EDGE('',*,*,#12915,.F.);
#16737=ORIENTED_EDGE('',*,*,#12914,.F.);
#16738=ORIENTED_EDGE('',*,*,#12916,.T.);
#16739=ORIENTED_EDGE('',*,*,#12917,.F.);
#16740=ORIENTED_EDGE('',*,*,#12918,.T.);
#16741=ORIENTED_EDGE('',*,*,#12919,.T.);
#16742=ORIENTED_EDGE('',*,*,#12918,.F.);
#16743=ORIENTED_EDGE('',*,*,#12913,.F.);
#16744=ORIENTED_EDGE('',*,*,#12920,.T.);
#16745=ORIENTED_EDGE('',*,*,#12917,.T.);
#16746=ORIENTED_EDGE('',*,*,#12920,.F.);
#16747=ORIENTED_EDGE('',*,*,#12916,.F.);
#16748=ORIENTED_EDGE('',*,*,#12910,.T.);
#16749=ORIENTED_EDGE('',*,*,#12921,.T.);
#16750=ORIENTED_EDGE('',*,*,#12922,.T.);
#16751=ORIENTED_EDGE('',*,*,#12923,.F.);
#16752=ORIENTED_EDGE('',*,*,#12924,.T.);
#16753=ORIENTED_EDGE('',*,*,#12925,.F.);
#16754=ORIENTED_EDGE('',*,*,#12926,.T.);
#16755=ORIENTED_EDGE('',*,*,#12927,.T.);
#16756=ORIENTED_EDGE('',*,*,#12926,.F.);
#16757=ORIENTED_EDGE('',*,*,#12928,.T.);
#16758=ORIENTED_EDGE('',*,*,#12929,.T.);
#16759=ORIENTED_EDGE('',*,*,#12930,.F.);
#16760=ORIENTED_EDGE('',*,*,#12931,.T.);
#16761=ORIENTED_EDGE('',*,*,#12932,.T.);
#16762=ORIENTED_EDGE('',*,*,#12933,.T.);
#16763=ORIENTED_EDGE('',*,*,#12934,.F.);
#16764=ORIENTED_EDGE('',*,*,#12935,.T.);
#16765=ORIENTED_EDGE('',*,*,#12936,.T.);
#16766=ORIENTED_EDGE('',*,*,#12937,.T.);
#16767=ORIENTED_EDGE('',*,*,#12938,.F.);
#16768=ORIENTED_EDGE('',*,*,#12939,.T.);
#16769=ORIENTED_EDGE('',*,*,#12912,.T.);
#16770=ORIENTED_EDGE('',*,*,#12925,.T.);
#16771=ORIENTED_EDGE('',*,*,#12919,.F.);
#16772=ORIENTED_EDGE('',*,*,#12930,.T.);
#16773=ORIENTED_EDGE('',*,*,#12940,.T.);
#16774=ORIENTED_EDGE('',*,*,#12923,.T.);
#16775=ORIENTED_EDGE('',*,*,#12941,.T.);
#16776=ORIENTED_EDGE('',*,*,#12938,.T.);
#16777=ORIENTED_EDGE('',*,*,#12942,.T.);
#16778=ORIENTED_EDGE('',*,*,#12934,.T.);
#16779=ORIENTED_EDGE('',*,*,#12943,.T.);
#16780=ORIENTED_EDGE('',*,*,#12927,.F.);
#16781=ORIENTED_EDGE('',*,*,#12921,.F.);
#16782=ORIENTED_EDGE('',*,*,#12944,.T.);
#16783=ORIENTED_EDGE('',*,*,#12928,.F.);
#16784=ORIENTED_EDGE('',*,*,#12945,.T.);
#16785=ORIENTED_EDGE('',*,*,#12932,.F.);
#16786=ORIENTED_EDGE('',*,*,#12946,.T.);
#16787=ORIENTED_EDGE('',*,*,#12936,.F.);
#16788=ORIENTED_EDGE('',*,*,#12947,.T.);
#16789=ORIENTED_EDGE('',*,*,#12915,.T.);
#16790=ORIENTED_EDGE('',*,*,#12947,.F.);
#16791=ORIENTED_EDGE('',*,*,#12939,.F.);
#16792=ORIENTED_EDGE('',*,*,#12941,.F.);
#16793=ORIENTED_EDGE('',*,*,#12922,.F.);
#16794=ORIENTED_EDGE('',*,*,#12946,.F.);
#16795=ORIENTED_EDGE('',*,*,#12935,.F.);
#16796=ORIENTED_EDGE('',*,*,#12942,.F.);
#16797=ORIENTED_EDGE('',*,*,#12937,.F.);
#16798=ORIENTED_EDGE('',*,*,#12945,.F.);
#16799=ORIENTED_EDGE('',*,*,#12931,.F.);
#16800=ORIENTED_EDGE('',*,*,#12943,.F.);
#16801=ORIENTED_EDGE('',*,*,#12933,.F.);
#16802=ORIENTED_EDGE('',*,*,#12944,.F.);
#16803=ORIENTED_EDGE('',*,*,#12924,.F.);
#16804=ORIENTED_EDGE('',*,*,#12940,.F.);
#16805=ORIENTED_EDGE('',*,*,#12929,.F.);
#16806=ORIENTED_EDGE('',*,*,#12948,.F.);
#16807=ORIENTED_EDGE('',*,*,#12949,.T.);
#16808=ORIENTED_EDGE('',*,*,#12950,.F.);
#16809=ORIENTED_EDGE('',*,*,#12949,.F.);
#16810=ORIENTED_EDGE('',*,*,#12951,.T.);
#16811=ORIENTED_EDGE('',*,*,#12952,.T.);
#16812=ORIENTED_EDGE('',*,*,#12953,.F.);
#16813=ORIENTED_EDGE('',*,*,#12952,.F.);
#16814=ORIENTED_EDGE('',*,*,#12954,.T.);
#16815=ORIENTED_EDGE('',*,*,#12951,.F.);
#16816=ORIENTED_EDGE('',*,*,#12955,.T.);
#16817=ORIENTED_EDGE('',*,*,#12948,.T.);
#16818=ORIENTED_EDGE('',*,*,#12955,.F.);
#16819=ORIENTED_EDGE('',*,*,#12954,.F.);
#16820=ORIENTED_EDGE('',*,*,#12953,.T.);
#16821=ORIENTED_EDGE('',*,*,#12950,.T.);
#16822=ORIENTED_EDGE('',*,*,#12956,.F.);
#16823=ORIENTED_EDGE('',*,*,#12957,.F.);
#16824=ORIENTED_EDGE('',*,*,#12958,.F.);
#16825=ORIENTED_EDGE('',*,*,#12959,.F.);
#16826=ORIENTED_EDGE('',*,*,#12960,.F.);
#16827=ORIENTED_EDGE('',*,*,#12961,.F.);
#16828=ORIENTED_EDGE('',*,*,#12956,.T.);
#16829=ORIENTED_EDGE('',*,*,#12962,.F.);
#16830=ORIENTED_EDGE('',*,*,#12963,.F.);
#16831=ORIENTED_EDGE('',*,*,#12964,.T.);
#16832=ORIENTED_EDGE('',*,*,#12957,.T.);
#16833=ORIENTED_EDGE('',*,*,#12964,.F.);
#16834=ORIENTED_EDGE('',*,*,#12965,.F.);
#16835=ORIENTED_EDGE('',*,*,#12966,.T.);
#16836=ORIENTED_EDGE('',*,*,#12958,.T.);
#16837=ORIENTED_EDGE('',*,*,#12966,.F.);
#16838=ORIENTED_EDGE('',*,*,#12967,.F.);
#16839=ORIENTED_EDGE('',*,*,#12968,.T.);
#16840=ORIENTED_EDGE('',*,*,#12959,.T.);
#16841=ORIENTED_EDGE('',*,*,#12968,.F.);
#16842=ORIENTED_EDGE('',*,*,#12969,.F.);
#16843=ORIENTED_EDGE('',*,*,#12970,.T.);
#16844=ORIENTED_EDGE('',*,*,#12960,.T.);
#16845=ORIENTED_EDGE('',*,*,#12970,.F.);
#16846=ORIENTED_EDGE('',*,*,#12971,.F.);
#16847=ORIENTED_EDGE('',*,*,#12972,.T.);
#16848=ORIENTED_EDGE('',*,*,#12961,.T.);
#16849=ORIENTED_EDGE('',*,*,#12972,.F.);
#16850=ORIENTED_EDGE('',*,*,#12973,.F.);
#16851=ORIENTED_EDGE('',*,*,#12962,.T.);
#16852=ORIENTED_EDGE('',*,*,#12963,.T.);
#16853=ORIENTED_EDGE('',*,*,#12973,.T.);
#16854=ORIENTED_EDGE('',*,*,#12971,.T.);
#16855=ORIENTED_EDGE('',*,*,#12969,.T.);
#16856=ORIENTED_EDGE('',*,*,#12967,.T.);
#16857=ORIENTED_EDGE('',*,*,#12965,.T.);
#16858=ORIENTED_EDGE('',*,*,#12974,.F.);
#16859=ORIENTED_EDGE('',*,*,#12975,.T.);
#16860=ORIENTED_EDGE('',*,*,#12976,.T.);
#16861=ORIENTED_EDGE('',*,*,#12975,.F.);
#16862=ORIENTED_EDGE('',*,*,#12977,.F.);
#16863=ORIENTED_EDGE('',*,*,#12978,.T.);
#16864=ORIENTED_EDGE('',*,*,#12979,.T.);
#16865=ORIENTED_EDGE('',*,*,#12978,.F.);
#16866=ORIENTED_EDGE('',*,*,#12974,.T.);
#16867=ORIENTED_EDGE('',*,*,#12979,.F.);
#16868=ORIENTED_EDGE('',*,*,#12976,.F.);
#16869=ORIENTED_EDGE('',*,*,#12977,.T.);
#16870=ORIENTED_EDGE('',*,*,#12980,.F.);
#16871=ORIENTED_EDGE('',*,*,#12981,.T.);
#16872=ORIENTED_EDGE('',*,*,#12982,.T.);
#16873=ORIENTED_EDGE('',*,*,#12981,.F.);
#16874=ORIENTED_EDGE('',*,*,#12983,.F.);
#16875=ORIENTED_EDGE('',*,*,#12984,.T.);
#16876=ORIENTED_EDGE('',*,*,#12985,.T.);
#16877=ORIENTED_EDGE('',*,*,#12984,.F.);
#16878=ORIENTED_EDGE('',*,*,#12986,.T.);
#16879=ORIENTED_EDGE('',*,*,#12987,.T.);
#16880=ORIENTED_EDGE('',*,*,#12988,.F.);
#16881=ORIENTED_EDGE('',*,*,#12987,.F.);
#16882=ORIENTED_EDGE('',*,*,#12989,.T.);
#16883=ORIENTED_EDGE('',*,*,#12990,.T.);
#16884=ORIENTED_EDGE('',*,*,#12991,.T.);
#16885=ORIENTED_EDGE('',*,*,#12992,.T.);
#16886=ORIENTED_EDGE('',*,*,#12993,.T.);
#16887=ORIENTED_EDGE('',*,*,#12994,.T.);
#16888=ORIENTED_EDGE('',*,*,#12995,.T.);
#16889=ORIENTED_EDGE('',*,*,#12996,.T.);
#16890=ORIENTED_EDGE('',*,*,#12997,.T.);
#16891=ORIENTED_EDGE('',*,*,#12998,.T.);
#16892=ORIENTED_EDGE('',*,*,#12999,.T.);
#16893=ORIENTED_EDGE('',*,*,#13000,.T.);
#16894=ORIENTED_EDGE('',*,*,#12986,.F.);
#16895=ORIENTED_EDGE('',*,*,#13001,.F.);
#16896=ORIENTED_EDGE('',*,*,#13002,.F.);
#16897=ORIENTED_EDGE('',*,*,#13003,.F.);
#16898=ORIENTED_EDGE('',*,*,#13004,.F.);
#16899=ORIENTED_EDGE('',*,*,#13005,.F.);
#16900=ORIENTED_EDGE('',*,*,#13006,.F.);
#16901=ORIENTED_EDGE('',*,*,#13007,.F.);
#16902=ORIENTED_EDGE('',*,*,#13008,.F.);
#16903=ORIENTED_EDGE('',*,*,#13009,.F.);
#16904=ORIENTED_EDGE('',*,*,#13010,.F.);
#16905=ORIENTED_EDGE('',*,*,#13011,.F.);
#16906=ORIENTED_EDGE('',*,*,#13012,.F.);
#16907=ORIENTED_EDGE('',*,*,#12988,.T.);
#16908=ORIENTED_EDGE('',*,*,#13001,.T.);
#16909=ORIENTED_EDGE('',*,*,#13013,.F.);
#16910=ORIENTED_EDGE('',*,*,#12989,.F.);
#16911=ORIENTED_EDGE('',*,*,#13014,.T.);
#16912=ORIENTED_EDGE('',*,*,#12982,.F.);
#16913=ORIENTED_EDGE('',*,*,#13012,.T.);
#16914=ORIENTED_EDGE('',*,*,#13015,.F.);
#16915=ORIENTED_EDGE('',*,*,#12990,.F.);
#16916=ORIENTED_EDGE('',*,*,#13013,.T.);
#16917=ORIENTED_EDGE('',*,*,#13011,.T.);
#16918=ORIENTED_EDGE('',*,*,#13016,.F.);
#16919=ORIENTED_EDGE('',*,*,#12991,.F.);
#16920=ORIENTED_EDGE('',*,*,#13015,.T.);
#16921=ORIENTED_EDGE('',*,*,#13010,.T.);
#16922=ORIENTED_EDGE('',*,*,#13017,.F.);
#16923=ORIENTED_EDGE('',*,*,#12992,.F.);
#16924=ORIENTED_EDGE('',*,*,#13016,.T.);
#16925=ORIENTED_EDGE('',*,*,#12980,.T.);
#16926=ORIENTED_EDGE('',*,*,#12983,.T.);
#16927=ORIENTED_EDGE('',*,*,#13009,.T.);
#16928=ORIENTED_EDGE('',*,*,#13018,.F.);
#16929=ORIENTED_EDGE('',*,*,#12993,.F.);
#16930=ORIENTED_EDGE('',*,*,#13017,.T.);
#16931=ORIENTED_EDGE('',*,*,#13008,.T.);
#16932=ORIENTED_EDGE('',*,*,#13019,.F.);
#16933=ORIENTED_EDGE('',*,*,#12994,.F.);
#16934=ORIENTED_EDGE('',*,*,#13018,.T.);
#16935=ORIENTED_EDGE('',*,*,#13007,.T.);
#16936=ORIENTED_EDGE('',*,*,#13020,.F.);
#16937=ORIENTED_EDGE('',*,*,#12995,.F.);
#16938=ORIENTED_EDGE('',*,*,#13019,.T.);
#16939=ORIENTED_EDGE('',*,*,#12985,.F.);
#16940=ORIENTED_EDGE('',*,*,#13006,.T.);
#16941=ORIENTED_EDGE('',*,*,#13021,.F.);
#16942=ORIENTED_EDGE('',*,*,#12996,.F.);
#16943=ORIENTED_EDGE('',*,*,#13020,.T.);
#16944=ORIENTED_EDGE('',*,*,#13005,.T.);
#16945=ORIENTED_EDGE('',*,*,#13022,.F.);
#16946=ORIENTED_EDGE('',*,*,#12997,.F.);
#16947=ORIENTED_EDGE('',*,*,#13021,.T.);
#16948=ORIENTED_EDGE('',*,*,#13004,.T.);
#16949=ORIENTED_EDGE('',*,*,#13023,.F.);
#16950=ORIENTED_EDGE('',*,*,#12998,.F.);
#16951=ORIENTED_EDGE('',*,*,#13022,.T.);
#16952=ORIENTED_EDGE('',*,*,#13003,.T.);
#16953=ORIENTED_EDGE('',*,*,#13024,.F.);
#16954=ORIENTED_EDGE('',*,*,#12999,.F.);
#16955=ORIENTED_EDGE('',*,*,#13023,.T.);
#16956=ORIENTED_EDGE('',*,*,#13002,.T.);
#16957=ORIENTED_EDGE('',*,*,#13014,.F.);
#16958=ORIENTED_EDGE('',*,*,#13000,.F.);
#16959=ORIENTED_EDGE('',*,*,#13024,.T.);
#16960=ORIENTED_EDGE('',*,*,#13025,.F.);
#16961=ORIENTED_EDGE('',*,*,#13026,.T.);
#16962=ORIENTED_EDGE('',*,*,#13027,.T.);
#16963=ORIENTED_EDGE('',*,*,#13026,.F.);
#16964=ORIENTED_EDGE('',*,*,#13027,.F.);
#16965=ORIENTED_EDGE('',*,*,#13028,.T.);
#16966=ORIENTED_EDGE('',*,*,#13029,.T.);
#16967=ORIENTED_EDGE('',*,*,#13028,.F.);
#16968=ORIENTED_EDGE('',*,*,#13029,.F.);
#16969=ORIENTED_EDGE('',*,*,#13030,.T.);
#16970=ORIENTED_EDGE('',*,*,#13031,.T.);
#16971=ORIENTED_EDGE('',*,*,#13030,.F.);
#16972=ORIENTED_EDGE('',*,*,#13032,.F.);
#16973=ORIENTED_EDGE('',*,*,#13033,.T.);
#16974=ORIENTED_EDGE('',*,*,#13034,.T.);
#16975=ORIENTED_EDGE('',*,*,#13033,.F.);
#16976=ORIENTED_EDGE('',*,*,#13035,.F.);
#16977=ORIENTED_EDGE('',*,*,#13036,.T.);
#16978=ORIENTED_EDGE('',*,*,#13037,.T.);
#16979=ORIENTED_EDGE('',*,*,#13036,.F.);
#16980=ORIENTED_EDGE('',*,*,#13038,.F.);
#16981=ORIENTED_EDGE('',*,*,#13039,.T.);
#16982=ORIENTED_EDGE('',*,*,#13040,.T.);
#16983=ORIENTED_EDGE('',*,*,#13039,.F.);
#16984=ORIENTED_EDGE('',*,*,#13040,.F.);
#16985=ORIENTED_EDGE('',*,*,#13041,.T.);
#16986=ORIENTED_EDGE('',*,*,#13042,.T.);
#16987=ORIENTED_EDGE('',*,*,#13041,.F.);
#16988=ORIENTED_EDGE('',*,*,#13042,.F.);
#16989=ORIENTED_EDGE('',*,*,#13043,.T.);
#16990=ORIENTED_EDGE('',*,*,#13044,.T.);
#16991=ORIENTED_EDGE('',*,*,#13043,.F.);
#16992=ORIENTED_EDGE('',*,*,#13045,.F.);
#16993=ORIENTED_EDGE('',*,*,#13046,.T.);
#16994=ORIENTED_EDGE('',*,*,#13047,.T.);
#16995=ORIENTED_EDGE('',*,*,#13046,.F.);
#16996=ORIENTED_EDGE('',*,*,#13048,.F.);
#16997=ORIENTED_EDGE('',*,*,#13049,.T.);
#16998=ORIENTED_EDGE('',*,*,#13050,.T.);
#16999=ORIENTED_EDGE('',*,*,#13049,.F.);
#17000=ORIENTED_EDGE('',*,*,#13047,.F.);
#17001=ORIENTED_EDGE('',*,*,#13048,.T.);
#17002=ORIENTED_EDGE('',*,*,#13044,.F.);
#17003=ORIENTED_EDGE('',*,*,#13045,.T.);
#17004=ORIENTED_EDGE('',*,*,#13038,.T.);
#17005=ORIENTED_EDGE('',*,*,#13037,.F.);
#17006=ORIENTED_EDGE('',*,*,#13035,.T.);
#17007=ORIENTED_EDGE('',*,*,#13034,.F.);
#17008=ORIENTED_EDGE('',*,*,#13032,.T.);
#17009=ORIENTED_EDGE('',*,*,#13031,.F.);
#17010=ORIENTED_EDGE('',*,*,#13050,.F.);
#17011=ORIENTED_EDGE('',*,*,#13025,.T.);
#17012=ORIENTED_EDGE('',*,*,#13051,.T.);
#17013=ORIENTED_EDGE('',*,*,#13052,.T.);
#17014=ORIENTED_EDGE('',*,*,#13053,.F.);
#17015=ORIENTED_EDGE('',*,*,#13052,.F.);
#17016=ORIENTED_EDGE('',*,*,#13054,.T.);
#17017=ORIENTED_EDGE('',*,*,#13055,.T.);
#17018=ORIENTED_EDGE('',*,*,#13056,.F.);
#17019=ORIENTED_EDGE('',*,*,#13055,.F.);
#17020=ORIENTED_EDGE('',*,*,#13057,.F.);
#17021=ORIENTED_EDGE('',*,*,#13058,.T.);
#17022=ORIENTED_EDGE('',*,*,#13059,.T.);
#17023=ORIENTED_EDGE('',*,*,#13060,.F.);
#17024=ORIENTED_EDGE('',*,*,#13061,.F.);
#17025=ORIENTED_EDGE('',*,*,#13062,.T.);
#17026=ORIENTED_EDGE('',*,*,#13063,.T.);
#17027=ORIENTED_EDGE('',*,*,#13064,.F.);
#17028=ORIENTED_EDGE('',*,*,#13065,.T.);
#17029=ORIENTED_EDGE('',*,*,#13066,.T.);
#17030=ORIENTED_EDGE('',*,*,#13067,.T.);
#17031=ORIENTED_EDGE('',*,*,#13068,.T.);
#17032=ORIENTED_EDGE('',*,*,#13061,.T.);
#17033=ORIENTED_EDGE('',*,*,#13069,.T.);
#17034=ORIENTED_EDGE('',*,*,#13070,.T.);
#17035=ORIENTED_EDGE('',*,*,#13071,.T.);
#17036=ORIENTED_EDGE('',*,*,#13072,.T.);
#17037=ORIENTED_EDGE('',*,*,#13073,.T.);
#17038=ORIENTED_EDGE('',*,*,#13057,.T.);
#17039=ORIENTED_EDGE('',*,*,#13074,.T.);
#17040=ORIENTED_EDGE('',*,*,#13051,.F.);
#17041=ORIENTED_EDGE('',*,*,#13054,.F.);
#17042=ORIENTED_EDGE('',*,*,#13075,.F.);
#17043=ORIENTED_EDGE('',*,*,#13076,.F.);
#17044=ORIENTED_EDGE('',*,*,#13059,.F.);
#17045=ORIENTED_EDGE('',*,*,#13077,.F.);
#17046=ORIENTED_EDGE('',*,*,#13078,.F.);
#17047=ORIENTED_EDGE('',*,*,#13079,.F.);
#17048=ORIENTED_EDGE('',*,*,#13080,.F.);
#17049=ORIENTED_EDGE('',*,*,#13081,.F.);
#17050=ORIENTED_EDGE('',*,*,#13063,.F.);
#17051=ORIENTED_EDGE('',*,*,#13082,.F.);
#17052=ORIENTED_EDGE('',*,*,#13083,.F.);
#17053=ORIENTED_EDGE('',*,*,#13084,.F.);
#17054=ORIENTED_EDGE('',*,*,#13056,.T.);
#17055=ORIENTED_EDGE('',*,*,#13053,.T.);
#17056=ORIENTED_EDGE('',*,*,#13075,.T.);
#17057=ORIENTED_EDGE('',*,*,#13085,.F.);
#17058=ORIENTED_EDGE('',*,*,#13065,.F.);
#17059=ORIENTED_EDGE('',*,*,#13086,.T.);
#17060=ORIENTED_EDGE('',*,*,#13084,.T.);
#17061=ORIENTED_EDGE('',*,*,#13087,.F.);
#17062=ORIENTED_EDGE('',*,*,#13066,.F.);
#17063=ORIENTED_EDGE('',*,*,#13085,.T.);
#17064=ORIENTED_EDGE('',*,*,#13083,.T.);
#17065=ORIENTED_EDGE('',*,*,#13088,.F.);
#17066=ORIENTED_EDGE('',*,*,#13067,.F.);
#17067=ORIENTED_EDGE('',*,*,#13087,.T.);
#17068=ORIENTED_EDGE('',*,*,#13082,.T.);
#17069=ORIENTED_EDGE('',*,*,#13062,.F.);
#17070=ORIENTED_EDGE('',*,*,#13068,.F.);
#17071=ORIENTED_EDGE('',*,*,#13088,.T.);
#17072=ORIENTED_EDGE('',*,*,#13081,.T.);
#17073=ORIENTED_EDGE('',*,*,#13089,.F.);
#17074=ORIENTED_EDGE('',*,*,#13069,.F.);
#17075=ORIENTED_EDGE('',*,*,#13064,.T.);
#17076=ORIENTED_EDGE('',*,*,#13080,.T.);
#17077=ORIENTED_EDGE('',*,*,#13090,.F.);
#17078=ORIENTED_EDGE('',*,*,#13070,.F.);
#17079=ORIENTED_EDGE('',*,*,#13089,.T.);
#17080=ORIENTED_EDGE('',*,*,#13079,.T.);
#17081=ORIENTED_EDGE('',*,*,#13091,.F.);
#17082=ORIENTED_EDGE('',*,*,#13071,.F.);
#17083=ORIENTED_EDGE('',*,*,#13090,.T.);
#17084=ORIENTED_EDGE('',*,*,#13078,.T.);
#17085=ORIENTED_EDGE('',*,*,#13092,.F.);
#17086=ORIENTED_EDGE('',*,*,#13072,.F.);
#17087=ORIENTED_EDGE('',*,*,#13091,.T.);
#17088=ORIENTED_EDGE('',*,*,#13077,.T.);
#17089=ORIENTED_EDGE('',*,*,#13058,.F.);
#17090=ORIENTED_EDGE('',*,*,#13073,.F.);
#17091=ORIENTED_EDGE('',*,*,#13092,.T.);
#17092=ORIENTED_EDGE('',*,*,#13076,.T.);
#17093=ORIENTED_EDGE('',*,*,#13086,.F.);
#17094=ORIENTED_EDGE('',*,*,#13074,.F.);
#17095=ORIENTED_EDGE('',*,*,#13060,.T.);
#17096=ORIENTED_EDGE('',*,*,#13093,.F.);
#17097=ORIENTED_EDGE('',*,*,#13094,.T.);
#17098=ORIENTED_EDGE('',*,*,#13095,.T.);
#17099=ORIENTED_EDGE('',*,*,#13094,.F.);
#17100=ORIENTED_EDGE('',*,*,#13096,.F.);
#17101=ORIENTED_EDGE('',*,*,#13097,.T.);
#17102=ORIENTED_EDGE('',*,*,#13098,.T.);
#17103=ORIENTED_EDGE('',*,*,#13097,.F.);
#17104=ORIENTED_EDGE('',*,*,#13099,.F.);
#17105=ORIENTED_EDGE('',*,*,#13100,.T.);
#17106=ORIENTED_EDGE('',*,*,#13101,.T.);
#17107=ORIENTED_EDGE('',*,*,#13100,.F.);
#17108=ORIENTED_EDGE('',*,*,#13102,.F.);
#17109=ORIENTED_EDGE('',*,*,#13103,.T.);
#17110=ORIENTED_EDGE('',*,*,#13104,.T.);
#17111=ORIENTED_EDGE('',*,*,#13103,.F.);
#17112=ORIENTED_EDGE('',*,*,#13105,.F.);
#17113=ORIENTED_EDGE('',*,*,#13106,.F.);
#17114=ORIENTED_EDGE('',*,*,#13107,.T.);
#17115=ORIENTED_EDGE('',*,*,#13108,.T.);
#17116=ORIENTED_EDGE('',*,*,#13107,.F.);
#17117=ORIENTED_EDGE('',*,*,#13109,.F.);
#17118=ORIENTED_EDGE('',*,*,#13110,.F.);
#17119=ORIENTED_EDGE('',*,*,#13111,.T.);
#17120=ORIENTED_EDGE('',*,*,#13112,.T.);
#17121=ORIENTED_EDGE('',*,*,#13113,.F.);
#17122=ORIENTED_EDGE('',*,*,#13114,.F.);
#17123=ORIENTED_EDGE('',*,*,#13115,.T.);
#17124=ORIENTED_EDGE('',*,*,#13108,.F.);
#17125=ORIENTED_EDGE('',*,*,#13113,.T.);
#17126=ORIENTED_EDGE('',*,*,#13116,.T.);
#17127=ORIENTED_EDGE('',*,*,#13117,.F.);
#17128=ORIENTED_EDGE('',*,*,#13118,.F.);
#17129=ORIENTED_EDGE('',*,*,#13119,.F.);
#17130=ORIENTED_EDGE('',*,*,#13120,.F.);
#17131=ORIENTED_EDGE('',*,*,#13117,.T.);
#17132=ORIENTED_EDGE('',*,*,#13121,.T.);
#17133=ORIENTED_EDGE('',*,*,#13122,.F.);
#17134=ORIENTED_EDGE('',*,*,#13123,.F.);
#17135=ORIENTED_EDGE('',*,*,#13124,.T.);
#17136=ORIENTED_EDGE('',*,*,#13125,.F.);
#17137=ORIENTED_EDGE('',*,*,#13122,.T.);
#17138=ORIENTED_EDGE('',*,*,#13126,.T.);
#17139=ORIENTED_EDGE('',*,*,#13111,.F.);
#17140=ORIENTED_EDGE('',*,*,#13127,.F.);
#17141=ORIENTED_EDGE('',*,*,#13128,.F.);
#17142=ORIENTED_EDGE('',*,*,#13118,.T.);
#17143=ORIENTED_EDGE('',*,*,#13125,.T.);
#17144=ORIENTED_EDGE('',*,*,#13112,.F.);
#17145=ORIENTED_EDGE('',*,*,#13126,.F.);
#17146=ORIENTED_EDGE('',*,*,#13121,.F.);
#17147=ORIENTED_EDGE('',*,*,#13116,.F.);
#17148=ORIENTED_EDGE('',*,*,#13093,.T.);
#17149=ORIENTED_EDGE('',*,*,#13096,.T.);
#17150=ORIENTED_EDGE('',*,*,#13099,.T.);
#17151=ORIENTED_EDGE('',*,*,#13102,.T.);
#17152=ORIENTED_EDGE('',*,*,#13105,.T.);
#17153=ORIENTED_EDGE('',*,*,#13115,.F.);
#17154=ORIENTED_EDGE('',*,*,#13129,.F.);
#17155=ORIENTED_EDGE('',*,*,#13130,.T.);
#17156=ORIENTED_EDGE('',*,*,#13106,.T.);
#17157=ORIENTED_EDGE('',*,*,#13130,.F.);
#17158=ORIENTED_EDGE('',*,*,#13131,.F.);
#17159=ORIENTED_EDGE('',*,*,#13109,.T.);
#17160=ORIENTED_EDGE('',*,*,#13127,.T.);
#17161=ORIENTED_EDGE('',*,*,#13124,.F.);
#17162=ORIENTED_EDGE('',*,*,#13132,.F.);
#17163=ORIENTED_EDGE('',*,*,#13133,.T.);
#17164=ORIENTED_EDGE('',*,*,#13128,.T.);
#17165=ORIENTED_EDGE('',*,*,#13133,.F.);
#17166=ORIENTED_EDGE('',*,*,#13134,.F.);
#17167=ORIENTED_EDGE('',*,*,#13119,.T.);
#17168=ORIENTED_EDGE('',*,*,#13120,.T.);
#17169=ORIENTED_EDGE('',*,*,#13134,.T.);
#17170=ORIENTED_EDGE('',*,*,#13132,.T.);
#17171=ORIENTED_EDGE('',*,*,#13123,.T.);
#17172=ORIENTED_EDGE('',*,*,#13110,.T.);
#17173=ORIENTED_EDGE('',*,*,#13131,.T.);
#17174=ORIENTED_EDGE('',*,*,#13129,.T.);
#17175=ORIENTED_EDGE('',*,*,#13114,.T.);
#17176=ORIENTED_EDGE('',*,*,#13095,.F.);
#17177=ORIENTED_EDGE('',*,*,#13098,.F.);
#17178=ORIENTED_EDGE('',*,*,#13101,.F.);
#17179=ORIENTED_EDGE('',*,*,#13104,.F.);
#17180=ORIENTED_EDGE('',*,*,#13135,.F.);
#17181=ORIENTED_EDGE('',*,*,#13136,.T.);
#17182=ORIENTED_EDGE('',*,*,#13137,.T.);
#17183=ORIENTED_EDGE('',*,*,#13136,.F.);
#17184=ORIENTED_EDGE('',*,*,#13138,.F.);
#17185=ORIENTED_EDGE('',*,*,#13139,.T.);
#17186=ORIENTED_EDGE('',*,*,#13140,.T.);
#17187=ORIENTED_EDGE('',*,*,#13139,.F.);
#17188=ORIENTED_EDGE('',*,*,#13141,.F.);
#17189=ORIENTED_EDGE('',*,*,#13142,.T.);
#17190=ORIENTED_EDGE('',*,*,#13143,.T.);
#17191=ORIENTED_EDGE('',*,*,#13142,.F.);
#17192=ORIENTED_EDGE('',*,*,#13144,.F.);
#17193=ORIENTED_EDGE('',*,*,#13145,.T.);
#17194=ORIENTED_EDGE('',*,*,#13146,.T.);
#17195=ORIENTED_EDGE('',*,*,#13145,.F.);
#17196=ORIENTED_EDGE('',*,*,#13147,.F.);
#17197=ORIENTED_EDGE('',*,*,#13148,.F.);
#17198=ORIENTED_EDGE('',*,*,#13149,.T.);
#17199=ORIENTED_EDGE('',*,*,#13150,.T.);
#17200=ORIENTED_EDGE('',*,*,#13149,.F.);
#17201=ORIENTED_EDGE('',*,*,#13151,.F.);
#17202=ORIENTED_EDGE('',*,*,#13152,.F.);
#17203=ORIENTED_EDGE('',*,*,#13153,.T.);
#17204=ORIENTED_EDGE('',*,*,#13154,.T.);
#17205=ORIENTED_EDGE('',*,*,#13155,.F.);
#17206=ORIENTED_EDGE('',*,*,#13156,.F.);
#17207=ORIENTED_EDGE('',*,*,#13157,.T.);
#17208=ORIENTED_EDGE('',*,*,#13150,.F.);
#17209=ORIENTED_EDGE('',*,*,#13155,.T.);
#17210=ORIENTED_EDGE('',*,*,#13158,.T.);
#17211=ORIENTED_EDGE('',*,*,#13159,.F.);
#17212=ORIENTED_EDGE('',*,*,#13160,.F.);
#17213=ORIENTED_EDGE('',*,*,#13161,.F.);
#17214=ORIENTED_EDGE('',*,*,#13162,.F.);
#17215=ORIENTED_EDGE('',*,*,#13159,.T.);
#17216=ORIENTED_EDGE('',*,*,#13163,.T.);
#17217=ORIENTED_EDGE('',*,*,#13164,.F.);
#17218=ORIENTED_EDGE('',*,*,#13165,.F.);
#17219=ORIENTED_EDGE('',*,*,#13166,.T.);
#17220=ORIENTED_EDGE('',*,*,#13167,.F.);
#17221=ORIENTED_EDGE('',*,*,#13164,.T.);
#17222=ORIENTED_EDGE('',*,*,#13168,.T.);
#17223=ORIENTED_EDGE('',*,*,#13153,.F.);
#17224=ORIENTED_EDGE('',*,*,#13169,.F.);
#17225=ORIENTED_EDGE('',*,*,#13170,.F.);
#17226=ORIENTED_EDGE('',*,*,#13160,.T.);
#17227=ORIENTED_EDGE('',*,*,#13167,.T.);
#17228=ORIENTED_EDGE('',*,*,#13154,.F.);
#17229=ORIENTED_EDGE('',*,*,#13168,.F.);
#17230=ORIENTED_EDGE('',*,*,#13163,.F.);
#17231=ORIENTED_EDGE('',*,*,#13158,.F.);
#17232=ORIENTED_EDGE('',*,*,#13135,.T.);
#17233=ORIENTED_EDGE('',*,*,#13138,.T.);
#17234=ORIENTED_EDGE('',*,*,#13141,.T.);
#17235=ORIENTED_EDGE('',*,*,#13144,.T.);
#17236=ORIENTED_EDGE('',*,*,#13147,.T.);
#17237=ORIENTED_EDGE('',*,*,#13157,.F.);
#17238=ORIENTED_EDGE('',*,*,#13171,.F.);
#17239=ORIENTED_EDGE('',*,*,#13172,.T.);
#17240=ORIENTED_EDGE('',*,*,#13148,.T.);
#17241=ORIENTED_EDGE('',*,*,#13172,.F.);
#17242=ORIENTED_EDGE('',*,*,#13173,.F.);
#17243=ORIENTED_EDGE('',*,*,#13151,.T.);
#17244=ORIENTED_EDGE('',*,*,#13169,.T.);
#17245=ORIENTED_EDGE('',*,*,#13166,.F.);
#17246=ORIENTED_EDGE('',*,*,#13174,.F.);
#17247=ORIENTED_EDGE('',*,*,#13175,.T.);
#17248=ORIENTED_EDGE('',*,*,#13170,.T.);
#17249=ORIENTED_EDGE('',*,*,#13175,.F.);
#17250=ORIENTED_EDGE('',*,*,#13176,.F.);
#17251=ORIENTED_EDGE('',*,*,#13161,.T.);
#17252=ORIENTED_EDGE('',*,*,#13162,.T.);
#17253=ORIENTED_EDGE('',*,*,#13176,.T.);
#17254=ORIENTED_EDGE('',*,*,#13174,.T.);
#17255=ORIENTED_EDGE('',*,*,#13165,.T.);
#17256=ORIENTED_EDGE('',*,*,#13152,.T.);
#17257=ORIENTED_EDGE('',*,*,#13173,.T.);
#17258=ORIENTED_EDGE('',*,*,#13171,.T.);
#17259=ORIENTED_EDGE('',*,*,#13156,.T.);
#17260=ORIENTED_EDGE('',*,*,#13137,.F.);
#17261=ORIENTED_EDGE('',*,*,#13140,.F.);
#17262=ORIENTED_EDGE('',*,*,#13143,.F.);
#17263=ORIENTED_EDGE('',*,*,#13146,.F.);
#17264=ORIENTED_EDGE('',*,*,#13177,.F.);
#17265=ORIENTED_EDGE('',*,*,#13178,.T.);
#17266=ORIENTED_EDGE('',*,*,#13179,.T.);
#17267=ORIENTED_EDGE('',*,*,#13178,.F.);
#17268=ORIENTED_EDGE('',*,*,#13180,.F.);
#17269=ORIENTED_EDGE('',*,*,#13181,.T.);
#17270=ORIENTED_EDGE('',*,*,#13182,.T.);
#17271=ORIENTED_EDGE('',*,*,#13181,.F.);
#17272=ORIENTED_EDGE('',*,*,#13183,.F.);
#17273=ORIENTED_EDGE('',*,*,#13184,.T.);
#17274=ORIENTED_EDGE('',*,*,#13185,.T.);
#17275=ORIENTED_EDGE('',*,*,#13184,.F.);
#17276=ORIENTED_EDGE('',*,*,#13186,.F.);
#17277=ORIENTED_EDGE('',*,*,#13187,.T.);
#17278=ORIENTED_EDGE('',*,*,#13188,.T.);
#17279=ORIENTED_EDGE('',*,*,#13187,.F.);
#17280=ORIENTED_EDGE('',*,*,#13189,.F.);
#17281=ORIENTED_EDGE('',*,*,#13190,.T.);
#17282=ORIENTED_EDGE('',*,*,#13191,.T.);
#17283=ORIENTED_EDGE('',*,*,#13190,.F.);
#17284=ORIENTED_EDGE('',*,*,#13192,.F.);
#17285=ORIENTED_EDGE('',*,*,#13193,.T.);
#17286=ORIENTED_EDGE('',*,*,#13194,.T.);
#17287=ORIENTED_EDGE('',*,*,#13193,.F.);
#17288=ORIENTED_EDGE('',*,*,#13195,.F.);
#17289=ORIENTED_EDGE('',*,*,#13196,.T.);
#17290=ORIENTED_EDGE('',*,*,#13197,.T.);
#17291=ORIENTED_EDGE('',*,*,#13196,.F.);
#17292=ORIENTED_EDGE('',*,*,#13198,.F.);
#17293=ORIENTED_EDGE('',*,*,#13199,.T.);
#17294=ORIENTED_EDGE('',*,*,#13200,.T.);
#17295=ORIENTED_EDGE('',*,*,#13199,.F.);
#17296=ORIENTED_EDGE('',*,*,#13201,.F.);
#17297=ORIENTED_EDGE('',*,*,#13202,.T.);
#17298=ORIENTED_EDGE('',*,*,#13203,.T.);
#17299=ORIENTED_EDGE('',*,*,#13202,.F.);
#17300=ORIENTED_EDGE('',*,*,#13204,.F.);
#17301=ORIENTED_EDGE('',*,*,#13205,.T.);
#17302=ORIENTED_EDGE('',*,*,#13206,.T.);
#17303=ORIENTED_EDGE('',*,*,#13205,.F.);
#17304=ORIENTED_EDGE('',*,*,#13207,.F.);
#17305=ORIENTED_EDGE('',*,*,#13208,.T.);
#17306=ORIENTED_EDGE('',*,*,#13209,.T.);
#17307=ORIENTED_EDGE('',*,*,#13208,.F.);
#17308=ORIENTED_EDGE('',*,*,#13210,.F.);
#17309=ORIENTED_EDGE('',*,*,#13211,.T.);
#17310=ORIENTED_EDGE('',*,*,#13212,.T.);
#17311=ORIENTED_EDGE('',*,*,#13211,.F.);
#17312=ORIENTED_EDGE('',*,*,#13213,.T.);
#17313=ORIENTED_EDGE('',*,*,#13214,.T.);
#17314=ORIENTED_EDGE('',*,*,#13215,.T.);
#17315=ORIENTED_EDGE('',*,*,#13216,.T.);
#17316=ORIENTED_EDGE('',*,*,#13185,.F.);
#17317=ORIENTED_EDGE('',*,*,#13179,.F.);
#17318=ORIENTED_EDGE('',*,*,#13182,.F.);
#17319=ORIENTED_EDGE('',*,*,#13188,.F.);
#17320=ORIENTED_EDGE('',*,*,#13191,.F.);
#17321=ORIENTED_EDGE('',*,*,#13194,.F.);
#17322=ORIENTED_EDGE('',*,*,#13197,.F.);
#17323=ORIENTED_EDGE('',*,*,#13203,.F.);
#17324=ORIENTED_EDGE('',*,*,#13212,.F.);
#17325=ORIENTED_EDGE('',*,*,#13217,.T.);
#17326=ORIENTED_EDGE('',*,*,#13218,.F.);
#17327=ORIENTED_EDGE('',*,*,#13213,.F.);
#17328=ORIENTED_EDGE('',*,*,#13219,.T.);
#17329=ORIENTED_EDGE('',*,*,#13220,.T.);
#17330=ORIENTED_EDGE('',*,*,#13221,.F.);
#17331=ORIENTED_EDGE('',*,*,#13214,.F.);
#17332=ORIENTED_EDGE('',*,*,#13218,.T.);
#17333=ORIENTED_EDGE('',*,*,#13222,.T.);
#17334=ORIENTED_EDGE('',*,*,#13223,.F.);
#17335=ORIENTED_EDGE('',*,*,#13215,.F.);
#17336=ORIENTED_EDGE('',*,*,#13221,.T.);
#17337=ORIENTED_EDGE('',*,*,#13224,.T.);
#17338=ORIENTED_EDGE('',*,*,#13219,.F.);
#17339=ORIENTED_EDGE('',*,*,#13216,.F.);
#17340=ORIENTED_EDGE('',*,*,#13223,.T.);
#17341=ORIENTED_EDGE('',*,*,#13217,.F.);
#17342=ORIENTED_EDGE('',*,*,#13224,.F.);
#17343=ORIENTED_EDGE('',*,*,#13222,.F.);
#17344=ORIENTED_EDGE('',*,*,#13220,.F.);
#17345=ORIENTED_EDGE('',*,*,#13177,.T.);
#17346=ORIENTED_EDGE('',*,*,#13180,.T.);
#17347=ORIENTED_EDGE('',*,*,#13183,.T.);
#17348=ORIENTED_EDGE('',*,*,#13186,.T.);
#17349=ORIENTED_EDGE('',*,*,#13189,.T.);
#17350=ORIENTED_EDGE('',*,*,#13192,.T.);
#17351=ORIENTED_EDGE('',*,*,#13198,.T.);
#17352=ORIENTED_EDGE('',*,*,#13204,.T.);
#17353=ORIENTED_EDGE('',*,*,#13207,.T.);
#17354=ORIENTED_EDGE('',*,*,#13210,.T.);
#17355=ORIENTED_EDGE('',*,*,#13209,.F.);
#17356=ORIENTED_EDGE('',*,*,#13201,.T.);
#17357=ORIENTED_EDGE('',*,*,#13206,.F.);
#17358=ORIENTED_EDGE('',*,*,#13195,.T.);
#17359=ORIENTED_EDGE('',*,*,#13200,.F.);
#17360=ORIENTED_EDGE('',*,*,#13225,.F.);
#17361=ORIENTED_EDGE('',*,*,#13225,.T.);
#17362=ORIENTED_EDGE('',*,*,#13226,.T.);
#17363=ORIENTED_EDGE('',*,*,#13227,.F.);
#17364=ORIENTED_EDGE('',*,*,#13226,.F.);
#17365=ORIENTED_EDGE('',*,*,#13228,.T.);
#17366=ORIENTED_EDGE('',*,*,#13229,.T.);
#17367=ORIENTED_EDGE('',*,*,#13230,.F.);
#17368=ORIENTED_EDGE('',*,*,#13229,.F.);
#17369=ORIENTED_EDGE('',*,*,#13231,.T.);
#17370=ORIENTED_EDGE('',*,*,#13232,.T.);
#17371=ORIENTED_EDGE('',*,*,#13233,.T.);
#17372=ORIENTED_EDGE('',*,*,#13231,.F.);
#17373=ORIENTED_EDGE('',*,*,#13233,.F.);
#17374=ORIENTED_EDGE('',*,*,#13234,.F.);
#17375=ORIENTED_EDGE('',*,*,#13235,.F.);
#17376=ORIENTED_EDGE('',*,*,#13236,.F.);
#17377=ORIENTED_EDGE('',*,*,#13237,.T.);
#17378=ORIENTED_EDGE('',*,*,#13235,.T.);
#17379=ORIENTED_EDGE('',*,*,#13238,.F.);
#17380=ORIENTED_EDGE('',*,*,#13239,.F.);
#17381=ORIENTED_EDGE('',*,*,#13240,.T.);
#17382=ORIENTED_EDGE('',*,*,#13241,.F.);
#17383=ORIENTED_EDGE('',*,*,#13242,.F.);
#17384=ORIENTED_EDGE('',*,*,#13239,.T.);
#17385=ORIENTED_EDGE('',*,*,#13243,.T.);
#17386=ORIENTED_EDGE('',*,*,#13244,.F.);
#17387=ORIENTED_EDGE('',*,*,#13245,.F.);
#17388=ORIENTED_EDGE('',*,*,#13246,.T.);
#17389=ORIENTED_EDGE('',*,*,#13247,.F.);
#17390=ORIENTED_EDGE('',*,*,#13248,.T.);
#17391=ORIENTED_EDGE('',*,*,#13249,.T.);
#17392=ORIENTED_EDGE('',*,*,#13246,.F.);
#17393=ORIENTED_EDGE('',*,*,#13250,.T.);
#17394=ORIENTED_EDGE('',*,*,#13251,.T.);
#17395=ORIENTED_EDGE('',*,*,#13252,.T.);
#17396=ORIENTED_EDGE('',*,*,#13253,.F.);
#17397=ORIENTED_EDGE('',*,*,#13248,.F.);
#17398=ORIENTED_EDGE('',*,*,#13252,.F.);
#17399=ORIENTED_EDGE('',*,*,#13254,.F.);
#17400=ORIENTED_EDGE('',*,*,#13254,.T.);
#17401=ORIENTED_EDGE('',*,*,#13255,.F.);
#17402=ORIENTED_EDGE('',*,*,#13256,.T.);
#17403=ORIENTED_EDGE('',*,*,#13257,.T.);
#17404=ORIENTED_EDGE('',*,*,#13249,.F.);
#17405=ORIENTED_EDGE('',*,*,#13257,.F.);
#17406=ORIENTED_EDGE('',*,*,#13258,.T.);
#17407=ORIENTED_EDGE('',*,*,#13259,.F.);
#17408=ORIENTED_EDGE('',*,*,#13260,.T.);
#17409=ORIENTED_EDGE('',*,*,#13261,.F.);
#17410=ORIENTED_EDGE('',*,*,#13243,.F.);
#17411=ORIENTED_EDGE('',*,*,#13259,.T.);
#17412=ORIENTED_EDGE('',*,*,#13262,.T.);
#17413=ORIENTED_EDGE('',*,*,#13263,.F.);
#17414=ORIENTED_EDGE('',*,*,#13260,.F.);
#17415=ORIENTED_EDGE('',*,*,#13264,.T.);
#17416=ORIENTED_EDGE('',*,*,#13258,.F.);
#17417=ORIENTED_EDGE('',*,*,#13265,.T.);
#17418=ORIENTED_EDGE('',*,*,#13266,.T.);
#17419=ORIENTED_EDGE('',*,*,#13264,.F.);
#17420=ORIENTED_EDGE('',*,*,#13256,.F.);
#17421=ORIENTED_EDGE('',*,*,#13267,.F.);
#17422=ORIENTED_EDGE('',*,*,#13265,.F.);
#17423=ORIENTED_EDGE('',*,*,#13268,.T.);
#17424=ORIENTED_EDGE('',*,*,#13269,.F.);
#17425=ORIENTED_EDGE('',*,*,#13270,.F.);
#17426=ORIENTED_EDGE('',*,*,#13271,.T.);
#17427=ORIENTED_EDGE('',*,*,#13272,.T.);
#17428=ORIENTED_EDGE('',*,*,#13273,.T.);
#17429=ORIENTED_EDGE('',*,*,#13274,.F.);
#17430=ORIENTED_EDGE('',*,*,#13271,.F.);
#17431=ORIENTED_EDGE('',*,*,#13275,.F.);
#17432=ORIENTED_EDGE('',*,*,#13273,.F.);
#17433=ORIENTED_EDGE('',*,*,#13276,.F.);
#17434=ORIENTED_EDGE('',*,*,#13267,.T.);
#17435=ORIENTED_EDGE('',*,*,#13277,.F.);
#17436=ORIENTED_EDGE('',*,*,#13276,.T.);
#17437=ORIENTED_EDGE('',*,*,#13278,.T.);
#17438=ORIENTED_EDGE('',*,*,#13255,.T.);
#17439=ORIENTED_EDGE('',*,*,#13251,.F.);
#17440=ORIENTED_EDGE('',*,*,#13279,.F.);
#17441=ORIENTED_EDGE('',*,*,#13277,.T.);
#17442=ORIENTED_EDGE('',*,*,#13280,.T.);
#17443=ORIENTED_EDGE('',*,*,#13281,.F.);
#17444=ORIENTED_EDGE('',*,*,#13275,.T.);
#17445=ORIENTED_EDGE('',*,*,#13279,.T.);
#17446=ORIENTED_EDGE('',*,*,#13250,.F.);
#17447=ORIENTED_EDGE('',*,*,#13282,.F.);
#17448=ORIENTED_EDGE('',*,*,#13280,.F.);
#17449=ORIENTED_EDGE('',*,*,#13283,.T.);
#17450=ORIENTED_EDGE('',*,*,#13284,.F.);
#17451=ORIENTED_EDGE('',*,*,#13285,.F.);
#17452=ORIENTED_EDGE('',*,*,#13286,.T.);
#17453=ORIENTED_EDGE('',*,*,#13287,.T.);
#17454=ORIENTED_EDGE('',*,*,#13282,.T.);
#17455=ORIENTED_EDGE('',*,*,#13288,.F.);
#17456=ORIENTED_EDGE('',*,*,#13286,.F.);
#17457=ORIENTED_EDGE('',*,*,#13274,.T.);
#17458=ORIENTED_EDGE('',*,*,#13281,.T.);
#17459=ORIENTED_EDGE('',*,*,#13287,.F.);
#17460=ORIENTED_EDGE('',*,*,#13289,.F.);
#17461=ORIENTED_EDGE('',*,*,#13285,.T.);
#17462=ORIENTED_EDGE('',*,*,#13290,.F.);
#17463=ORIENTED_EDGE('',*,*,#13268,.F.);
#17464=ORIENTED_EDGE('',*,*,#13289,.T.);
#17465=ORIENTED_EDGE('',*,*,#13291,.T.);
#17466=ORIENTED_EDGE('',*,*,#13292,.F.);
#17467=ORIENTED_EDGE('',*,*,#13293,.F.);
#17468=ORIENTED_EDGE('',*,*,#13294,.T.);
#17469=ORIENTED_EDGE('',*,*,#13295,.F.);
#17470=ORIENTED_EDGE('',*,*,#13296,.T.);
#17471=ORIENTED_EDGE('',*,*,#13297,.T.);
#17472=ORIENTED_EDGE('',*,*,#13294,.F.);
#17473=ORIENTED_EDGE('',*,*,#13298,.T.);
#17474=ORIENTED_EDGE('',*,*,#13299,.T.);
#17475=ORIENTED_EDGE('',*,*,#13300,.T.);
#17476=ORIENTED_EDGE('',*,*,#13301,.F.);
#17477=ORIENTED_EDGE('',*,*,#13296,.F.);
#17478=ORIENTED_EDGE('',*,*,#13300,.F.);
#17479=ORIENTED_EDGE('',*,*,#13302,.F.);
#17480=ORIENTED_EDGE('',*,*,#13302,.T.);
#17481=ORIENTED_EDGE('',*,*,#13303,.F.);
#17482=ORIENTED_EDGE('',*,*,#13304,.T.);
#17483=ORIENTED_EDGE('',*,*,#13305,.T.);
#17484=ORIENTED_EDGE('',*,*,#13297,.F.);
#17485=ORIENTED_EDGE('',*,*,#13305,.F.);
#17486=ORIENTED_EDGE('',*,*,#13306,.T.);
#17487=ORIENTED_EDGE('',*,*,#13307,.F.);
#17488=ORIENTED_EDGE('',*,*,#13308,.T.);
#17489=ORIENTED_EDGE('',*,*,#13309,.F.);
#17490=ORIENTED_EDGE('',*,*,#13291,.F.);
#17491=ORIENTED_EDGE('',*,*,#13307,.T.);
#17492=ORIENTED_EDGE('',*,*,#13310,.T.);
#17493=ORIENTED_EDGE('',*,*,#13311,.F.);
#17494=ORIENTED_EDGE('',*,*,#13308,.F.);
#17495=ORIENTED_EDGE('',*,*,#13312,.T.);
#17496=ORIENTED_EDGE('',*,*,#13306,.F.);
#17497=ORIENTED_EDGE('',*,*,#13313,.T.);
#17498=ORIENTED_EDGE('',*,*,#13314,.T.);
#17499=ORIENTED_EDGE('',*,*,#13312,.F.);
#17500=ORIENTED_EDGE('',*,*,#13304,.F.);
#17501=ORIENTED_EDGE('',*,*,#13315,.F.);
#17502=ORIENTED_EDGE('',*,*,#13313,.F.);
#17503=ORIENTED_EDGE('',*,*,#13316,.T.);
#17504=ORIENTED_EDGE('',*,*,#13317,.F.);
#17505=ORIENTED_EDGE('',*,*,#13318,.F.);
#17506=ORIENTED_EDGE('',*,*,#13319,.T.);
#17507=ORIENTED_EDGE('',*,*,#13320,.T.);
#17508=ORIENTED_EDGE('',*,*,#13321,.T.);
#17509=ORIENTED_EDGE('',*,*,#13322,.F.);
#17510=ORIENTED_EDGE('',*,*,#13319,.F.);
#17511=ORIENTED_EDGE('',*,*,#13323,.F.);
#17512=ORIENTED_EDGE('',*,*,#13321,.F.);
#17513=ORIENTED_EDGE('',*,*,#13324,.F.);
#17514=ORIENTED_EDGE('',*,*,#13315,.T.);
#17515=ORIENTED_EDGE('',*,*,#13325,.F.);
#17516=ORIENTED_EDGE('',*,*,#13324,.T.);
#17517=ORIENTED_EDGE('',*,*,#13326,.T.);
#17518=ORIENTED_EDGE('',*,*,#13303,.T.);
#17519=ORIENTED_EDGE('',*,*,#13299,.F.);
#17520=ORIENTED_EDGE('',*,*,#13327,.F.);
#17521=ORIENTED_EDGE('',*,*,#13325,.T.);
#17522=ORIENTED_EDGE('',*,*,#13328,.T.);
#17523=ORIENTED_EDGE('',*,*,#13329,.F.);
#17524=ORIENTED_EDGE('',*,*,#13323,.T.);
#17525=ORIENTED_EDGE('',*,*,#13327,.T.);
#17526=ORIENTED_EDGE('',*,*,#13298,.F.);
#17527=ORIENTED_EDGE('',*,*,#13330,.F.);
#17528=ORIENTED_EDGE('',*,*,#13328,.F.);
#17529=ORIENTED_EDGE('',*,*,#13331,.T.);
#17530=ORIENTED_EDGE('',*,*,#13332,.F.);
#17531=ORIENTED_EDGE('',*,*,#13333,.F.);
#17532=ORIENTED_EDGE('',*,*,#13334,.T.);
#17533=ORIENTED_EDGE('',*,*,#13335,.T.);
#17534=ORIENTED_EDGE('',*,*,#13330,.T.);
#17535=ORIENTED_EDGE('',*,*,#13336,.F.);
#17536=ORIENTED_EDGE('',*,*,#13334,.F.);
#17537=ORIENTED_EDGE('',*,*,#13322,.T.);
#17538=ORIENTED_EDGE('',*,*,#13329,.T.);
#17539=ORIENTED_EDGE('',*,*,#13335,.F.);
#17540=ORIENTED_EDGE('',*,*,#13337,.F.);
#17541=ORIENTED_EDGE('',*,*,#13333,.T.);
#17542=ORIENTED_EDGE('',*,*,#13338,.F.);
#17543=ORIENTED_EDGE('',*,*,#13316,.F.);
#17544=ORIENTED_EDGE('',*,*,#13337,.T.);
#17545=ORIENTED_EDGE('',*,*,#13339,.T.);
#17546=ORIENTED_EDGE('',*,*,#13340,.F.);
#17547=ORIENTED_EDGE('',*,*,#13341,.F.);
#17548=ORIENTED_EDGE('',*,*,#13342,.T.);
#17549=ORIENTED_EDGE('',*,*,#13343,.F.);
#17550=ORIENTED_EDGE('',*,*,#13344,.T.);
#17551=ORIENTED_EDGE('',*,*,#13345,.T.);
#17552=ORIENTED_EDGE('',*,*,#13342,.F.);
#17553=ORIENTED_EDGE('',*,*,#13346,.T.);
#17554=ORIENTED_EDGE('',*,*,#13347,.T.);
#17555=ORIENTED_EDGE('',*,*,#13348,.T.);
#17556=ORIENTED_EDGE('',*,*,#13349,.F.);
#17557=ORIENTED_EDGE('',*,*,#13344,.F.);
#17558=ORIENTED_EDGE('',*,*,#13348,.F.);
#17559=ORIENTED_EDGE('',*,*,#13350,.F.);
#17560=ORIENTED_EDGE('',*,*,#13350,.T.);
#17561=ORIENTED_EDGE('',*,*,#13351,.F.);
#17562=ORIENTED_EDGE('',*,*,#13352,.T.);
#17563=ORIENTED_EDGE('',*,*,#13353,.T.);
#17564=ORIENTED_EDGE('',*,*,#13345,.F.);
#17565=ORIENTED_EDGE('',*,*,#13353,.F.);
#17566=ORIENTED_EDGE('',*,*,#13354,.T.);
#17567=ORIENTED_EDGE('',*,*,#13355,.F.);
#17568=ORIENTED_EDGE('',*,*,#13356,.T.);
#17569=ORIENTED_EDGE('',*,*,#13357,.F.);
#17570=ORIENTED_EDGE('',*,*,#13339,.F.);
#17571=ORIENTED_EDGE('',*,*,#13355,.T.);
#17572=ORIENTED_EDGE('',*,*,#13358,.T.);
#17573=ORIENTED_EDGE('',*,*,#13359,.F.);
#17574=ORIENTED_EDGE('',*,*,#13356,.F.);
#17575=ORIENTED_EDGE('',*,*,#13360,.T.);
#17576=ORIENTED_EDGE('',*,*,#13354,.F.);
#17577=ORIENTED_EDGE('',*,*,#13361,.T.);
#17578=ORIENTED_EDGE('',*,*,#13362,.T.);
#17579=ORIENTED_EDGE('',*,*,#13360,.F.);
#17580=ORIENTED_EDGE('',*,*,#13352,.F.);
#17581=ORIENTED_EDGE('',*,*,#13363,.F.);
#17582=ORIENTED_EDGE('',*,*,#13361,.F.);
#17583=ORIENTED_EDGE('',*,*,#13364,.T.);
#17584=ORIENTED_EDGE('',*,*,#13365,.F.);
#17585=ORIENTED_EDGE('',*,*,#13366,.F.);
#17586=ORIENTED_EDGE('',*,*,#13367,.T.);
#17587=ORIENTED_EDGE('',*,*,#13368,.T.);
#17588=ORIENTED_EDGE('',*,*,#13369,.T.);
#17589=ORIENTED_EDGE('',*,*,#13370,.F.);
#17590=ORIENTED_EDGE('',*,*,#13367,.F.);
#17591=ORIENTED_EDGE('',*,*,#13371,.F.);
#17592=ORIENTED_EDGE('',*,*,#13369,.F.);
#17593=ORIENTED_EDGE('',*,*,#13372,.F.);
#17594=ORIENTED_EDGE('',*,*,#13363,.T.);
#17595=ORIENTED_EDGE('',*,*,#13373,.F.);
#17596=ORIENTED_EDGE('',*,*,#13372,.T.);
#17597=ORIENTED_EDGE('',*,*,#13374,.T.);
#17598=ORIENTED_EDGE('',*,*,#13351,.T.);
#17599=ORIENTED_EDGE('',*,*,#13347,.F.);
#17600=ORIENTED_EDGE('',*,*,#13375,.F.);
#17601=ORIENTED_EDGE('',*,*,#13373,.T.);
#17602=ORIENTED_EDGE('',*,*,#13376,.T.);
#17603=ORIENTED_EDGE('',*,*,#13377,.F.);
#17604=ORIENTED_EDGE('',*,*,#13371,.T.);
#17605=ORIENTED_EDGE('',*,*,#13375,.T.);
#17606=ORIENTED_EDGE('',*,*,#13346,.F.);
#17607=ORIENTED_EDGE('',*,*,#13378,.F.);
#17608=ORIENTED_EDGE('',*,*,#13376,.F.);
#17609=ORIENTED_EDGE('',*,*,#13379,.T.);
#17610=ORIENTED_EDGE('',*,*,#13380,.F.);
#17611=ORIENTED_EDGE('',*,*,#13381,.F.);
#17612=ORIENTED_EDGE('',*,*,#13382,.T.);
#17613=ORIENTED_EDGE('',*,*,#13383,.T.);
#17614=ORIENTED_EDGE('',*,*,#13378,.T.);
#17615=ORIENTED_EDGE('',*,*,#13384,.F.);
#17616=ORIENTED_EDGE('',*,*,#13382,.F.);
#17617=ORIENTED_EDGE('',*,*,#13370,.T.);
#17618=ORIENTED_EDGE('',*,*,#13377,.T.);
#17619=ORIENTED_EDGE('',*,*,#13383,.F.);
#17620=ORIENTED_EDGE('',*,*,#13385,.F.);
#17621=ORIENTED_EDGE('',*,*,#13381,.T.);
#17622=ORIENTED_EDGE('',*,*,#13386,.F.);
#17623=ORIENTED_EDGE('',*,*,#13364,.F.);
#17624=ORIENTED_EDGE('',*,*,#13385,.T.);
#17625=ORIENTED_EDGE('',*,*,#13387,.T.);
#17626=ORIENTED_EDGE('',*,*,#13388,.F.);
#17627=ORIENTED_EDGE('',*,*,#13389,.F.);
#17628=ORIENTED_EDGE('',*,*,#13390,.T.);
#17629=ORIENTED_EDGE('',*,*,#13391,.F.);
#17630=ORIENTED_EDGE('',*,*,#13392,.T.);
#17631=ORIENTED_EDGE('',*,*,#13393,.T.);
#17632=ORIENTED_EDGE('',*,*,#13390,.F.);
#17633=ORIENTED_EDGE('',*,*,#13394,.T.);
#17634=ORIENTED_EDGE('',*,*,#13395,.T.);
#17635=ORIENTED_EDGE('',*,*,#13396,.T.);
#17636=ORIENTED_EDGE('',*,*,#13397,.F.);
#17637=ORIENTED_EDGE('',*,*,#13392,.F.);
#17638=ORIENTED_EDGE('',*,*,#13396,.F.);
#17639=ORIENTED_EDGE('',*,*,#13398,.F.);
#17640=ORIENTED_EDGE('',*,*,#13398,.T.);
#17641=ORIENTED_EDGE('',*,*,#13399,.F.);
#17642=ORIENTED_EDGE('',*,*,#13400,.T.);
#17643=ORIENTED_EDGE('',*,*,#13401,.T.);
#17644=ORIENTED_EDGE('',*,*,#13393,.F.);
#17645=ORIENTED_EDGE('',*,*,#13401,.F.);
#17646=ORIENTED_EDGE('',*,*,#13402,.T.);
#17647=ORIENTED_EDGE('',*,*,#13403,.F.);
#17648=ORIENTED_EDGE('',*,*,#13404,.T.);
#17649=ORIENTED_EDGE('',*,*,#13405,.F.);
#17650=ORIENTED_EDGE('',*,*,#13387,.F.);
#17651=ORIENTED_EDGE('',*,*,#13403,.T.);
#17652=ORIENTED_EDGE('',*,*,#13406,.T.);
#17653=ORIENTED_EDGE('',*,*,#13407,.F.);
#17654=ORIENTED_EDGE('',*,*,#13404,.F.);
#17655=ORIENTED_EDGE('',*,*,#13408,.T.);
#17656=ORIENTED_EDGE('',*,*,#13402,.F.);
#17657=ORIENTED_EDGE('',*,*,#13409,.T.);
#17658=ORIENTED_EDGE('',*,*,#13410,.T.);
#17659=ORIENTED_EDGE('',*,*,#13408,.F.);
#17660=ORIENTED_EDGE('',*,*,#13400,.F.);
#17661=ORIENTED_EDGE('',*,*,#13411,.F.);
#17662=ORIENTED_EDGE('',*,*,#13409,.F.);
#17663=ORIENTED_EDGE('',*,*,#13412,.T.);
#17664=ORIENTED_EDGE('',*,*,#13413,.F.);
#17665=ORIENTED_EDGE('',*,*,#13414,.F.);
#17666=ORIENTED_EDGE('',*,*,#13415,.T.);
#17667=ORIENTED_EDGE('',*,*,#13416,.T.);
#17668=ORIENTED_EDGE('',*,*,#13417,.T.);
#17669=ORIENTED_EDGE('',*,*,#13418,.F.);
#17670=ORIENTED_EDGE('',*,*,#13415,.F.);
#17671=ORIENTED_EDGE('',*,*,#13419,.F.);
#17672=ORIENTED_EDGE('',*,*,#13417,.F.);
#17673=ORIENTED_EDGE('',*,*,#13420,.F.);
#17674=ORIENTED_EDGE('',*,*,#13411,.T.);
#17675=ORIENTED_EDGE('',*,*,#13421,.F.);
#17676=ORIENTED_EDGE('',*,*,#13420,.T.);
#17677=ORIENTED_EDGE('',*,*,#13422,.T.);
#17678=ORIENTED_EDGE('',*,*,#13399,.T.);
#17679=ORIENTED_EDGE('',*,*,#13395,.F.);
#17680=ORIENTED_EDGE('',*,*,#13423,.F.);
#17681=ORIENTED_EDGE('',*,*,#13421,.T.);
#17682=ORIENTED_EDGE('',*,*,#13424,.T.);
#17683=ORIENTED_EDGE('',*,*,#13425,.F.);
#17684=ORIENTED_EDGE('',*,*,#13419,.T.);
#17685=ORIENTED_EDGE('',*,*,#13423,.T.);
#17686=ORIENTED_EDGE('',*,*,#13394,.F.);
#17687=ORIENTED_EDGE('',*,*,#13426,.F.);
#17688=ORIENTED_EDGE('',*,*,#13424,.F.);
#17689=ORIENTED_EDGE('',*,*,#13427,.T.);
#17690=ORIENTED_EDGE('',*,*,#13428,.F.);
#17691=ORIENTED_EDGE('',*,*,#13429,.F.);
#17692=ORIENTED_EDGE('',*,*,#13430,.T.);
#17693=ORIENTED_EDGE('',*,*,#13431,.T.);
#17694=ORIENTED_EDGE('',*,*,#13426,.T.);
#17695=ORIENTED_EDGE('',*,*,#13432,.F.);
#17696=ORIENTED_EDGE('',*,*,#13430,.F.);
#17697=ORIENTED_EDGE('',*,*,#13418,.T.);
#17698=ORIENTED_EDGE('',*,*,#13425,.T.);
#17699=ORIENTED_EDGE('',*,*,#13431,.F.);
#17700=ORIENTED_EDGE('',*,*,#13433,.F.);
#17701=ORIENTED_EDGE('',*,*,#13429,.T.);
#17702=ORIENTED_EDGE('',*,*,#13434,.F.);
#17703=ORIENTED_EDGE('',*,*,#13412,.F.);
#17704=ORIENTED_EDGE('',*,*,#13433,.T.);
#17705=ORIENTED_EDGE('',*,*,#13435,.F.);
#17706=ORIENTED_EDGE('',*,*,#13436,.F.);
#17707=ORIENTED_EDGE('',*,*,#13437,.F.);
#17708=ORIENTED_EDGE('',*,*,#13435,.T.);
#17709=ORIENTED_EDGE('',*,*,#13438,.T.);
#17710=ORIENTED_EDGE('',*,*,#13439,.T.);
#17711=ORIENTED_EDGE('',*,*,#13440,.F.);
#17712=ORIENTED_EDGE('',*,*,#13441,.F.);
#17713=ORIENTED_EDGE('',*,*,#13439,.F.);
#17714=ORIENTED_EDGE('',*,*,#13442,.F.);
#17715=ORIENTED_EDGE('',*,*,#13443,.F.);
#17716=ORIENTED_EDGE('',*,*,#13441,.T.);
#17717=ORIENTED_EDGE('',*,*,#13444,.T.);
#17718=ORIENTED_EDGE('',*,*,#13445,.F.);
#17719=ORIENTED_EDGE('',*,*,#13446,.T.);
#17720=ORIENTED_EDGE('',*,*,#13447,.F.);
#17721=ORIENTED_EDGE('',*,*,#13448,.F.);
#17722=ORIENTED_EDGE('',*,*,#13445,.T.);
#17723=ORIENTED_EDGE('',*,*,#13449,.T.);
#17724=ORIENTED_EDGE('',*,*,#13450,.F.);
#17725=ORIENTED_EDGE('',*,*,#13446,.F.);
#17726=ORIENTED_EDGE('',*,*,#13451,.T.);
#17727=ORIENTED_EDGE('',*,*,#13444,.F.);
#17728=ORIENTED_EDGE('',*,*,#13452,.F.);
#17729=ORIENTED_EDGE('',*,*,#13453,.T.);
#17730=ORIENTED_EDGE('',*,*,#13451,.F.);
#17731=ORIENTED_EDGE('',*,*,#13442,.T.);
#17732=ORIENTED_EDGE('',*,*,#13454,.F.);
#17733=ORIENTED_EDGE('',*,*,#13455,.T.);
#17734=ORIENTED_EDGE('',*,*,#13452,.T.);
#17735=ORIENTED_EDGE('',*,*,#13455,.F.);
#17736=ORIENTED_EDGE('',*,*,#13456,.F.);
#17737=ORIENTED_EDGE('',*,*,#13457,.F.);
#17738=ORIENTED_EDGE('',*,*,#13453,.F.);
#17739=ORIENTED_EDGE('',*,*,#13457,.T.);
#17740=ORIENTED_EDGE('',*,*,#13458,.T.);
#17741=ORIENTED_EDGE('',*,*,#13459,.F.);
#17742=ORIENTED_EDGE('',*,*,#13460,.T.);
#17743=ORIENTED_EDGE('',*,*,#13461,.F.);
#17744=ORIENTED_EDGE('',*,*,#13449,.F.);
#17745=ORIENTED_EDGE('',*,*,#13459,.T.);
#17746=ORIENTED_EDGE('',*,*,#13462,.T.);
#17747=ORIENTED_EDGE('',*,*,#13463,.F.);
#17748=ORIENTED_EDGE('',*,*,#13464,.F.);
#17749=ORIENTED_EDGE('',*,*,#13465,.T.);
#17750=ORIENTED_EDGE('',*,*,#13466,.F.);
#17751=ORIENTED_EDGE('',*,*,#13467,.T.);
#17752=ORIENTED_EDGE('',*,*,#13468,.T.);
#17753=ORIENTED_EDGE('',*,*,#13465,.F.);
#17754=ORIENTED_EDGE('',*,*,#13469,.T.);
#17755=ORIENTED_EDGE('',*,*,#13470,.T.);
#17756=ORIENTED_EDGE('',*,*,#13471,.T.);
#17757=ORIENTED_EDGE('',*,*,#13472,.F.);
#17758=ORIENTED_EDGE('',*,*,#13467,.F.);
#17759=ORIENTED_EDGE('',*,*,#13471,.F.);
#17760=ORIENTED_EDGE('',*,*,#13473,.F.);
#17761=ORIENTED_EDGE('',*,*,#13473,.T.);
#17762=ORIENTED_EDGE('',*,*,#13474,.F.);
#17763=ORIENTED_EDGE('',*,*,#13475,.T.);
#17764=ORIENTED_EDGE('',*,*,#13476,.T.);
#17765=ORIENTED_EDGE('',*,*,#13468,.F.);
#17766=ORIENTED_EDGE('',*,*,#13476,.F.);
#17767=ORIENTED_EDGE('',*,*,#13477,.T.);
#17768=ORIENTED_EDGE('',*,*,#13478,.F.);
#17769=ORIENTED_EDGE('',*,*,#13479,.T.);
#17770=ORIENTED_EDGE('',*,*,#13480,.F.);
#17771=ORIENTED_EDGE('',*,*,#13462,.F.);
#17772=ORIENTED_EDGE('',*,*,#13478,.T.);
#17773=ORIENTED_EDGE('',*,*,#13481,.T.);
#17774=ORIENTED_EDGE('',*,*,#13482,.F.);
#17775=ORIENTED_EDGE('',*,*,#13479,.F.);
#17776=ORIENTED_EDGE('',*,*,#13483,.T.);
#17777=ORIENTED_EDGE('',*,*,#13477,.F.);
#17778=ORIENTED_EDGE('',*,*,#13484,.T.);
#17779=ORIENTED_EDGE('',*,*,#13485,.T.);
#17780=ORIENTED_EDGE('',*,*,#13483,.F.);
#17781=ORIENTED_EDGE('',*,*,#13475,.F.);
#17782=ORIENTED_EDGE('',*,*,#13486,.F.);
#17783=ORIENTED_EDGE('',*,*,#13484,.F.);
#17784=ORIENTED_EDGE('',*,*,#13487,.T.);
#17785=ORIENTED_EDGE('',*,*,#13488,.F.);
#17786=ORIENTED_EDGE('',*,*,#13489,.F.);
#17787=ORIENTED_EDGE('',*,*,#13490,.T.);
#17788=ORIENTED_EDGE('',*,*,#13491,.T.);
#17789=ORIENTED_EDGE('',*,*,#13492,.T.);
#17790=ORIENTED_EDGE('',*,*,#13493,.F.);
#17791=ORIENTED_EDGE('',*,*,#13490,.F.);
#17792=ORIENTED_EDGE('',*,*,#13494,.F.);
#17793=ORIENTED_EDGE('',*,*,#13492,.F.);
#17794=ORIENTED_EDGE('',*,*,#13495,.F.);
#17795=ORIENTED_EDGE('',*,*,#13486,.T.);
#17796=ORIENTED_EDGE('',*,*,#13496,.F.);
#17797=ORIENTED_EDGE('',*,*,#13495,.T.);
#17798=ORIENTED_EDGE('',*,*,#13497,.T.);
#17799=ORIENTED_EDGE('',*,*,#13474,.T.);
#17800=ORIENTED_EDGE('',*,*,#13470,.F.);
#17801=ORIENTED_EDGE('',*,*,#13498,.F.);
#17802=ORIENTED_EDGE('',*,*,#13496,.T.);
#17803=ORIENTED_EDGE('',*,*,#13499,.T.);
#17804=ORIENTED_EDGE('',*,*,#13500,.F.);
#17805=ORIENTED_EDGE('',*,*,#13494,.T.);
#17806=ORIENTED_EDGE('',*,*,#13498,.T.);
#17807=ORIENTED_EDGE('',*,*,#13469,.F.);
#17808=ORIENTED_EDGE('',*,*,#13501,.F.);
#17809=ORIENTED_EDGE('',*,*,#13499,.F.);
#17810=ORIENTED_EDGE('',*,*,#13502,.T.);
#17811=ORIENTED_EDGE('',*,*,#13503,.F.);
#17812=ORIENTED_EDGE('',*,*,#13504,.F.);
#17813=ORIENTED_EDGE('',*,*,#13505,.T.);
#17814=ORIENTED_EDGE('',*,*,#13506,.T.);
#17815=ORIENTED_EDGE('',*,*,#13501,.T.);
#17816=ORIENTED_EDGE('',*,*,#13507,.F.);
#17817=ORIENTED_EDGE('',*,*,#13505,.F.);
#17818=ORIENTED_EDGE('',*,*,#13493,.T.);
#17819=ORIENTED_EDGE('',*,*,#13500,.T.);
#17820=ORIENTED_EDGE('',*,*,#13506,.F.);
#17821=ORIENTED_EDGE('',*,*,#13508,.F.);
#17822=ORIENTED_EDGE('',*,*,#13504,.T.);
#17823=ORIENTED_EDGE('',*,*,#13509,.F.);
#17824=ORIENTED_EDGE('',*,*,#13487,.F.);
#17825=ORIENTED_EDGE('',*,*,#13508,.T.);
#17826=ORIENTED_EDGE('',*,*,#13510,.T.);
#17827=ORIENTED_EDGE('',*,*,#13511,.F.);
#17828=ORIENTED_EDGE('',*,*,#13244,.T.);
#17829=ORIENTED_EDGE('',*,*,#13261,.T.);
#17830=ORIENTED_EDGE('',*,*,#13263,.T.);
#17831=ORIENTED_EDGE('',*,*,#13512,.F.);
#17832=ORIENTED_EDGE('',*,*,#13241,.T.);
#17833=ORIENTED_EDGE('',*,*,#13513,.T.);
#17834=ORIENTED_EDGE('',*,*,#13284,.T.);
#17835=ORIENTED_EDGE('',*,*,#13514,.F.);
#17836=ORIENTED_EDGE('',*,*,#13292,.T.);
#17837=ORIENTED_EDGE('',*,*,#13309,.T.);
#17838=ORIENTED_EDGE('',*,*,#13311,.T.);
#17839=ORIENTED_EDGE('',*,*,#13515,.F.);
#17840=ORIENTED_EDGE('',*,*,#13269,.T.);
#17841=ORIENTED_EDGE('',*,*,#13290,.T.);
#17842=ORIENTED_EDGE('',*,*,#13332,.T.);
#17843=ORIENTED_EDGE('',*,*,#13516,.F.);
#17844=ORIENTED_EDGE('',*,*,#13340,.T.);
#17845=ORIENTED_EDGE('',*,*,#13357,.T.);
#17846=ORIENTED_EDGE('',*,*,#13359,.T.);
#17847=ORIENTED_EDGE('',*,*,#13517,.F.);
#17848=ORIENTED_EDGE('',*,*,#13317,.T.);
#17849=ORIENTED_EDGE('',*,*,#13338,.T.);
#17850=ORIENTED_EDGE('',*,*,#13380,.T.);
#17851=ORIENTED_EDGE('',*,*,#13518,.F.);
#17852=ORIENTED_EDGE('',*,*,#13388,.T.);
#17853=ORIENTED_EDGE('',*,*,#13405,.T.);
#17854=ORIENTED_EDGE('',*,*,#13407,.T.);
#17855=ORIENTED_EDGE('',*,*,#13519,.F.);
#17856=ORIENTED_EDGE('',*,*,#13365,.T.);
#17857=ORIENTED_EDGE('',*,*,#13386,.T.);
#17858=ORIENTED_EDGE('',*,*,#13428,.T.);
#17859=ORIENTED_EDGE('',*,*,#13520,.F.);
#17860=ORIENTED_EDGE('',*,*,#13463,.T.);
#17861=ORIENTED_EDGE('',*,*,#13480,.T.);
#17862=ORIENTED_EDGE('',*,*,#13482,.T.);
#17863=ORIENTED_EDGE('',*,*,#13521,.F.);
#17864=ORIENTED_EDGE('',*,*,#13413,.T.);
#17865=ORIENTED_EDGE('',*,*,#13434,.T.);
#17866=ORIENTED_EDGE('',*,*,#13503,.T.);
#17867=ORIENTED_EDGE('',*,*,#13522,.F.);
#17868=ORIENTED_EDGE('',*,*,#13447,.T.);
#17869=ORIENTED_EDGE('',*,*,#13450,.T.);
#17870=ORIENTED_EDGE('',*,*,#13461,.T.);
#17871=ORIENTED_EDGE('',*,*,#13523,.F.);
#17872=ORIENTED_EDGE('',*,*,#13488,.T.);
#17873=ORIENTED_EDGE('',*,*,#13509,.T.);
#17874=ORIENTED_EDGE('',*,*,#13524,.T.);
#17875=ORIENTED_EDGE('',*,*,#13525,.T.);
#17876=ORIENTED_EDGE('',*,*,#13526,.T.);
#17877=ORIENTED_EDGE('',*,*,#13524,.F.);
#17878=ORIENTED_EDGE('',*,*,#13526,.F.);
#17879=ORIENTED_EDGE('',*,*,#13527,.T.);
#17880=ORIENTED_EDGE('',*,*,#13528,.T.);
#17881=ORIENTED_EDGE('',*,*,#13529,.T.);
#17882=ORIENTED_EDGE('',*,*,#13527,.F.);
#17883=ORIENTED_EDGE('',*,*,#13529,.F.);
#17884=ORIENTED_EDGE('',*,*,#13262,.F.);
#17885=ORIENTED_EDGE('',*,*,#13266,.F.);
#17886=ORIENTED_EDGE('',*,*,#13278,.F.);
#17887=ORIENTED_EDGE('',*,*,#13272,.F.);
#17888=ORIENTED_EDGE('',*,*,#13270,.T.);
#17889=ORIENTED_EDGE('',*,*,#13515,.T.);
#17890=ORIENTED_EDGE('',*,*,#13310,.F.);
#17891=ORIENTED_EDGE('',*,*,#13314,.F.);
#17892=ORIENTED_EDGE('',*,*,#13326,.F.);
#17893=ORIENTED_EDGE('',*,*,#13320,.F.);
#17894=ORIENTED_EDGE('',*,*,#13318,.T.);
#17895=ORIENTED_EDGE('',*,*,#13517,.T.);
#17896=ORIENTED_EDGE('',*,*,#13358,.F.);
#17897=ORIENTED_EDGE('',*,*,#13362,.F.);
#17898=ORIENTED_EDGE('',*,*,#13374,.F.);
#17899=ORIENTED_EDGE('',*,*,#13368,.F.);
#17900=ORIENTED_EDGE('',*,*,#13366,.T.);
#17901=ORIENTED_EDGE('',*,*,#13519,.T.);
#17902=ORIENTED_EDGE('',*,*,#13406,.F.);
#17903=ORIENTED_EDGE('',*,*,#13410,.F.);
#17904=ORIENTED_EDGE('',*,*,#13422,.F.);
#17905=ORIENTED_EDGE('',*,*,#13416,.F.);
#17906=ORIENTED_EDGE('',*,*,#13414,.T.);
#17907=ORIENTED_EDGE('',*,*,#13521,.T.);
#17908=ORIENTED_EDGE('',*,*,#13481,.F.);
#17909=ORIENTED_EDGE('',*,*,#13485,.F.);
#17910=ORIENTED_EDGE('',*,*,#13497,.F.);
#17911=ORIENTED_EDGE('',*,*,#13491,.F.);
#17912=ORIENTED_EDGE('',*,*,#13489,.T.);
#17913=ORIENTED_EDGE('',*,*,#13523,.T.);
#17914=ORIENTED_EDGE('',*,*,#13460,.F.);
#17915=ORIENTED_EDGE('',*,*,#13458,.F.);
#17916=ORIENTED_EDGE('',*,*,#13530,.F.);
#17917=ORIENTED_EDGE('',*,*,#13237,.F.);
#17918=ORIENTED_EDGE('',*,*,#13242,.T.);
#17919=ORIENTED_EDGE('',*,*,#13512,.T.);
#17920=ORIENTED_EDGE('',*,*,#13230,.T.);
#17921=ORIENTED_EDGE('',*,*,#13232,.F.);
#17922=ORIENTED_EDGE('',*,*,#13528,.F.);
#17923=ORIENTED_EDGE('',*,*,#13525,.F.);
#17924=ORIENTED_EDGE('',*,*,#13456,.T.);
#17925=ORIENTED_EDGE('',*,*,#13531,.F.);
#17926=ORIENTED_EDGE('',*,*,#13236,.T.);
#17927=ORIENTED_EDGE('',*,*,#13530,.T.);
#17928=ORIENTED_EDGE('',*,*,#13454,.T.);
#17929=ORIENTED_EDGE('',*,*,#13438,.F.);
#17930=ORIENTED_EDGE('',*,*,#13532,.F.);
#17931=ORIENTED_EDGE('',*,*,#13531,.T.);
#17932=ORIENTED_EDGE('',*,*,#13437,.T.);
#17933=ORIENTED_EDGE('',*,*,#13533,.F.);
#17934=ORIENTED_EDGE('',*,*,#13234,.T.);
#17935=ORIENTED_EDGE('',*,*,#13532,.T.);
#17936=ORIENTED_EDGE('',*,*,#13238,.T.);
#17937=ORIENTED_EDGE('',*,*,#13533,.T.);
#17938=ORIENTED_EDGE('',*,*,#13534,.F.);
#17939=ORIENTED_EDGE('',*,*,#13535,.F.);
#17940=ORIENTED_EDGE('',*,*,#13536,.T.);
#17941=ORIENTED_EDGE('',*,*,#13513,.F.);
#17942=ORIENTED_EDGE('',*,*,#13240,.F.);
#17943=ORIENTED_EDGE('',*,*,#13535,.T.);
#17944=ORIENTED_EDGE('',*,*,#13537,.T.);
#17945=ORIENTED_EDGE('',*,*,#13510,.F.);
#17946=ORIENTED_EDGE('',*,*,#13536,.F.);
#17947=ORIENTED_EDGE('',*,*,#13538,.T.);
#17948=ORIENTED_EDGE('',*,*,#13534,.T.);
#17949=ORIENTED_EDGE('',*,*,#13436,.T.);
#17950=ORIENTED_EDGE('',*,*,#13539,.F.);
#17951=ORIENTED_EDGE('',*,*,#13538,.F.);
#17952=ORIENTED_EDGE('',*,*,#13540,.F.);
#17953=ORIENTED_EDGE('',*,*,#13540,.T.);
#17954=ORIENTED_EDGE('',*,*,#13541,.T.);
#17955=ORIENTED_EDGE('',*,*,#13542,.F.);
#17956=ORIENTED_EDGE('',*,*,#13541,.F.);
#17957=ORIENTED_EDGE('',*,*,#13543,.F.);
#17958=ORIENTED_EDGE('',*,*,#13543,.T.);
#17959=ORIENTED_EDGE('',*,*,#13544,.T.);
#17960=ORIENTED_EDGE('',*,*,#13545,.F.);
#17961=ORIENTED_EDGE('',*,*,#13544,.F.);
#17962=ORIENTED_EDGE('',*,*,#13440,.T.);
#17963=ORIENTED_EDGE('',*,*,#13443,.T.);
#17964=ORIENTED_EDGE('',*,*,#13448,.T.);
#17965=ORIENTED_EDGE('',*,*,#13522,.T.);
#17966=ORIENTED_EDGE('',*,*,#13502,.F.);
#17967=ORIENTED_EDGE('',*,*,#13507,.T.);
#17968=ORIENTED_EDGE('',*,*,#13472,.T.);
#17969=ORIENTED_EDGE('',*,*,#13466,.T.);
#17970=ORIENTED_EDGE('',*,*,#13464,.T.);
#17971=ORIENTED_EDGE('',*,*,#13520,.T.);
#17972=ORIENTED_EDGE('',*,*,#13427,.F.);
#17973=ORIENTED_EDGE('',*,*,#13432,.T.);
#17974=ORIENTED_EDGE('',*,*,#13397,.T.);
#17975=ORIENTED_EDGE('',*,*,#13391,.T.);
#17976=ORIENTED_EDGE('',*,*,#13389,.T.);
#17977=ORIENTED_EDGE('',*,*,#13518,.T.);
#17978=ORIENTED_EDGE('',*,*,#13379,.F.);
#17979=ORIENTED_EDGE('',*,*,#13384,.T.);
#17980=ORIENTED_EDGE('',*,*,#13349,.T.);
#17981=ORIENTED_EDGE('',*,*,#13343,.T.);
#17982=ORIENTED_EDGE('',*,*,#13341,.T.);
#17983=ORIENTED_EDGE('',*,*,#13516,.T.);
#17984=ORIENTED_EDGE('',*,*,#13331,.F.);
#17985=ORIENTED_EDGE('',*,*,#13336,.T.);
#17986=ORIENTED_EDGE('',*,*,#13301,.T.);
#17987=ORIENTED_EDGE('',*,*,#13295,.T.);
#17988=ORIENTED_EDGE('',*,*,#13293,.T.);
#17989=ORIENTED_EDGE('',*,*,#13514,.T.);
#17990=ORIENTED_EDGE('',*,*,#13283,.F.);
#17991=ORIENTED_EDGE('',*,*,#13288,.T.);
#17992=ORIENTED_EDGE('',*,*,#13253,.T.);
#17993=ORIENTED_EDGE('',*,*,#13247,.T.);
#17994=ORIENTED_EDGE('',*,*,#13245,.T.);
#17995=ORIENTED_EDGE('',*,*,#13511,.T.);
#17996=ORIENTED_EDGE('',*,*,#13537,.F.);
#17997=ORIENTED_EDGE('',*,*,#13539,.T.);
#17998=ORIENTED_EDGE('',*,*,#13228,.F.);
#17999=ORIENTED_EDGE('',*,*,#13227,.T.);
#18000=ORIENTED_EDGE('',*,*,#13545,.T.);
#18001=ORIENTED_EDGE('',*,*,#13542,.T.);
#18002=ORIENTED_EDGE('',*,*,#13546,.T.);
#18003=ORIENTED_EDGE('',*,*,#13547,.T.);
#18004=ORIENTED_EDGE('',*,*,#13548,.T.);
#18005=ORIENTED_EDGE('',*,*,#13549,.T.);
#18006=ORIENTED_EDGE('',*,*,#13550,.T.);
#18007=ORIENTED_EDGE('',*,*,#13551,.T.);
#18008=ORIENTED_EDGE('',*,*,#13552,.T.);
#18009=ORIENTED_EDGE('',*,*,#13553,.T.);
#18010=ORIENTED_EDGE('',*,*,#13546,.F.);
#18011=ORIENTED_EDGE('',*,*,#13554,.T.);
#18012=ORIENTED_EDGE('',*,*,#13553,.F.);
#18013=ORIENTED_EDGE('',*,*,#13554,.F.);
#18014=ORIENTED_EDGE('',*,*,#13555,.F.);
#18015=ORIENTED_EDGE('',*,*,#13556,.F.);
#18016=ORIENTED_EDGE('',*,*,#13557,.F.);
#18017=ORIENTED_EDGE('',*,*,#13558,.F.);
#18018=ORIENTED_EDGE('',*,*,#13559,.F.);
#18019=ORIENTED_EDGE('',*,*,#13560,.F.);
#18020=ORIENTED_EDGE('',*,*,#13552,.F.);
#18021=ORIENTED_EDGE('',*,*,#13561,.F.);
#18022=ORIENTED_EDGE('',*,*,#13555,.T.);
#18023=ORIENTED_EDGE('',*,*,#13562,.T.);
#18024=ORIENTED_EDGE('',*,*,#13551,.F.);
#18025=ORIENTED_EDGE('',*,*,#13563,.F.);
#18026=ORIENTED_EDGE('',*,*,#13556,.T.);
#18027=ORIENTED_EDGE('',*,*,#13561,.T.);
#18028=ORIENTED_EDGE('',*,*,#13550,.F.);
#18029=ORIENTED_EDGE('',*,*,#13564,.F.);
#18030=ORIENTED_EDGE('',*,*,#13557,.T.);
#18031=ORIENTED_EDGE('',*,*,#13563,.T.);
#18032=ORIENTED_EDGE('',*,*,#13549,.F.);
#18033=ORIENTED_EDGE('',*,*,#13565,.F.);
#18034=ORIENTED_EDGE('',*,*,#13558,.T.);
#18035=ORIENTED_EDGE('',*,*,#13564,.T.);
#18036=ORIENTED_EDGE('',*,*,#13548,.F.);
#18037=ORIENTED_EDGE('',*,*,#13566,.F.);
#18038=ORIENTED_EDGE('',*,*,#13559,.T.);
#18039=ORIENTED_EDGE('',*,*,#13565,.T.);
#18040=ORIENTED_EDGE('',*,*,#13547,.F.);
#18041=ORIENTED_EDGE('',*,*,#13562,.F.);
#18042=ORIENTED_EDGE('',*,*,#13560,.T.);
#18043=ORIENTED_EDGE('',*,*,#13566,.T.);
#18044=ORIENTED_EDGE('',*,*,#13567,.T.);
#18045=ORIENTED_EDGE('',*,*,#13568,.F.);
#18046=ORIENTED_EDGE('',*,*,#13569,.T.);
#18047=ORIENTED_EDGE('',*,*,#13570,.T.);
#18048=ORIENTED_EDGE('',*,*,#13571,.T.);
#18049=ORIENTED_EDGE('',*,*,#13572,.T.);
#18050=ORIENTED_EDGE('',*,*,#13573,.T.);
#18051=ORIENTED_EDGE('',*,*,#13574,.T.);
#18052=ORIENTED_EDGE('',*,*,#13575,.T.);
#18053=ORIENTED_EDGE('',*,*,#13576,.T.);
#18054=ORIENTED_EDGE('',*,*,#13577,.T.);
#18055=ORIENTED_EDGE('',*,*,#13571,.F.);
#18056=ORIENTED_EDGE('',*,*,#13577,.F.);
#18057=ORIENTED_EDGE('',*,*,#13578,.T.);
#18058=ORIENTED_EDGE('',*,*,#13579,.T.);
#18059=ORIENTED_EDGE('',*,*,#13580,.T.);
#18060=ORIENTED_EDGE('',*,*,#13581,.T.);
#18061=ORIENTED_EDGE('',*,*,#13582,.T.);
#18062=ORIENTED_EDGE('',*,*,#13583,.F.);
#18063=ORIENTED_EDGE('',*,*,#13584,.T.);
#18064=ORIENTED_EDGE('',*,*,#13585,.T.);
#18065=ORIENTED_EDGE('',*,*,#13586,.T.);
#18066=ORIENTED_EDGE('',*,*,#13587,.T.);
#18067=ORIENTED_EDGE('',*,*,#13588,.T.);
#18068=ORIENTED_EDGE('',*,*,#13589,.F.);
#18069=ORIENTED_EDGE('',*,*,#13590,.T.);
#18070=ORIENTED_EDGE('',*,*,#13591,.F.);
#18071=ORIENTED_EDGE('',*,*,#13567,.F.);
#18072=ORIENTED_EDGE('',*,*,#13592,.F.);
#18073=ORIENTED_EDGE('',*,*,#13587,.F.);
#18074=ORIENTED_EDGE('',*,*,#13593,.T.);
#18075=ORIENTED_EDGE('',*,*,#13594,.T.);
#18076=ORIENTED_EDGE('',*,*,#13595,.T.);
#18077=ORIENTED_EDGE('',*,*,#13596,.T.);
#18078=ORIENTED_EDGE('',*,*,#13597,.T.);
#18079=ORIENTED_EDGE('',*,*,#13598,.T.);
#18080=ORIENTED_EDGE('',*,*,#13585,.F.);
#18081=ORIENTED_EDGE('',*,*,#13592,.T.);
#18082=ORIENTED_EDGE('',*,*,#13570,.F.);
#18083=ORIENTED_EDGE('',*,*,#13599,.T.);
#18084=ORIENTED_EDGE('',*,*,#13600,.T.);
#18085=ORIENTED_EDGE('',*,*,#13584,.F.);
#18086=ORIENTED_EDGE('',*,*,#13601,.F.);
#18087=ORIENTED_EDGE('',*,*,#13602,.T.);
#18088=ORIENTED_EDGE('',*,*,#13596,.F.);
#18089=ORIENTED_EDGE('',*,*,#13603,.T.);
#18090=ORIENTED_EDGE('',*,*,#13604,.F.);
#18091=ORIENTED_EDGE('',*,*,#13588,.F.);
#18092=ORIENTED_EDGE('',*,*,#13595,.F.);
#18093=ORIENTED_EDGE('',*,*,#13605,.F.);
#18094=ORIENTED_EDGE('',*,*,#13590,.F.);
#18095=ORIENTED_EDGE('',*,*,#13600,.F.);
#18096=ORIENTED_EDGE('',*,*,#13606,.F.);
#18097=ORIENTED_EDGE('',*,*,#13607,.F.);
#18098=ORIENTED_EDGE('',*,*,#13608,.F.);
#18099=ORIENTED_EDGE('',*,*,#13609,.F.);
#18100=ORIENTED_EDGE('',*,*,#13597,.F.);
#18101=ORIENTED_EDGE('',*,*,#13602,.F.);
#18102=ORIENTED_EDGE('',*,*,#13610,.F.);
#18103=ORIENTED_EDGE('',*,*,#13603,.F.);
#18104=ORIENTED_EDGE('',*,*,#13594,.F.);
#18105=ORIENTED_EDGE('',*,*,#13611,.F.);
#18106=ORIENTED_EDGE('',*,*,#13612,.T.);
#18107=ORIENTED_EDGE('',*,*,#13613,.T.);
#18108=ORIENTED_EDGE('',*,*,#13614,.T.);
#18109=ORIENTED_EDGE('',*,*,#13615,.T.);
#18110=ORIENTED_EDGE('',*,*,#13569,.F.);
#18111=ORIENTED_EDGE('',*,*,#13616,.F.);
#18112=ORIENTED_EDGE('',*,*,#13606,.T.);
#18113=ORIENTED_EDGE('',*,*,#13599,.F.);
#18114=ORIENTED_EDGE('',*,*,#13609,.T.);
#18115=ORIENTED_EDGE('',*,*,#13617,.F.);
#18116=ORIENTED_EDGE('',*,*,#13582,.F.);
#18117=ORIENTED_EDGE('',*,*,#13598,.F.);
#18118=ORIENTED_EDGE('',*,*,#13586,.F.);
#18119=ORIENTED_EDGE('',*,*,#13618,.F.);
#18120=ORIENTED_EDGE('',*,*,#13611,.T.);
#18121=ORIENTED_EDGE('',*,*,#13593,.F.);
#18122=ORIENTED_EDGE('',*,*,#13615,.F.);
#18123=ORIENTED_EDGE('',*,*,#13619,.F.);
#18124=ORIENTED_EDGE('',*,*,#13573,.F.);
#18125=ORIENTED_EDGE('',*,*,#13620,.F.);
#18126=ORIENTED_EDGE('',*,*,#13613,.F.);
#18127=ORIENTED_EDGE('',*,*,#13621,.F.);
#18128=ORIENTED_EDGE('',*,*,#13575,.F.);
#18129=ORIENTED_EDGE('',*,*,#13622,.F.);
#18130=ORIENTED_EDGE('',*,*,#13623,.F.);
#18131=ORIENTED_EDGE('',*,*,#13620,.T.);
#18132=ORIENTED_EDGE('',*,*,#13572,.F.);
#18133=ORIENTED_EDGE('',*,*,#13621,.T.);
#18134=ORIENTED_EDGE('',*,*,#13612,.F.);
#18135=ORIENTED_EDGE('',*,*,#13619,.T.);
#18136=ORIENTED_EDGE('',*,*,#13614,.F.);
#18137=ORIENTED_EDGE('',*,*,#13622,.T.);
#18138=ORIENTED_EDGE('',*,*,#13574,.F.);
#18139=ORIENTED_EDGE('',*,*,#13623,.T.);
#18140=ORIENTED_EDGE('',*,*,#13624,.T.);
#18141=ORIENTED_EDGE('',*,*,#13625,.F.);
#18142=ORIENTED_EDGE('',*,*,#13626,.F.);
#18143=ORIENTED_EDGE('',*,*,#13627,.F.);
#18144=ORIENTED_EDGE('',*,*,#13624,.F.);
#18145=ORIENTED_EDGE('',*,*,#13576,.F.);
#18146=ORIENTED_EDGE('',*,*,#13628,.T.);
#18147=ORIENTED_EDGE('',*,*,#13627,.T.);
#18148=ORIENTED_EDGE('',*,*,#13626,.T.);
#18149=ORIENTED_EDGE('',*,*,#13629,.T.);
#18150=ORIENTED_EDGE('',*,*,#13607,.T.);
#18151=ORIENTED_EDGE('',*,*,#13616,.T.);
#18152=ORIENTED_EDGE('',*,*,#13568,.T.);
#18153=ORIENTED_EDGE('',*,*,#13591,.T.);
#18154=ORIENTED_EDGE('',*,*,#13605,.T.);
#18155=ORIENTED_EDGE('',*,*,#13618,.T.);
#18156=ORIENTED_EDGE('',*,*,#13589,.T.);
#18157=ORIENTED_EDGE('',*,*,#13604,.T.);
#18158=ORIENTED_EDGE('',*,*,#13610,.T.);
#18159=ORIENTED_EDGE('',*,*,#13601,.T.);
#18160=ORIENTED_EDGE('',*,*,#13583,.T.);
#18161=ORIENTED_EDGE('',*,*,#13617,.T.);
#18162=ORIENTED_EDGE('',*,*,#13608,.T.);
#18163=ORIENTED_EDGE('',*,*,#13629,.F.);
#18164=ORIENTED_EDGE('',*,*,#13625,.T.);
#18165=ORIENTED_EDGE('',*,*,#13628,.F.);
#18166=ORIENTED_EDGE('',*,*,#13630,.T.);
#18167=ORIENTED_EDGE('',*,*,#13631,.T.);
#18168=ORIENTED_EDGE('',*,*,#13632,.T.);
#18169=ORIENTED_EDGE('',*,*,#13633,.T.);
#18170=ORIENTED_EDGE('',*,*,#13634,.T.);
#18171=ORIENTED_EDGE('',*,*,#13635,.T.);
#18172=ORIENTED_EDGE('',*,*,#13636,.T.);
#18173=ORIENTED_EDGE('',*,*,#13637,.T.);
#18174=ORIENTED_EDGE('',*,*,#13638,.T.);
#18175=ORIENTED_EDGE('',*,*,#13639,.T.);
#18176=ORIENTED_EDGE('',*,*,#13640,.T.);
#18177=ORIENTED_EDGE('',*,*,#13641,.T.);
#18178=ORIENTED_EDGE('',*,*,#13642,.T.);
#18179=ORIENTED_EDGE('',*,*,#13643,.T.);
#18180=ORIENTED_EDGE('',*,*,#13644,.T.);
#18181=ORIENTED_EDGE('',*,*,#13645,.T.);
#18182=ORIENTED_EDGE('',*,*,#13646,.T.);
#18183=ORIENTED_EDGE('',*,*,#13647,.T.);
#18184=ORIENTED_EDGE('',*,*,#13648,.T.);
#18185=ORIENTED_EDGE('',*,*,#13649,.T.);
#18186=ORIENTED_EDGE('',*,*,#13650,.T.);
#18187=ORIENTED_EDGE('',*,*,#13651,.T.);
#18188=ORIENTED_EDGE('',*,*,#13652,.T.);
#18189=ORIENTED_EDGE('',*,*,#13653,.T.);
#18190=ORIENTED_EDGE('',*,*,#13654,.T.);
#18191=ORIENTED_EDGE('',*,*,#13655,.T.);
#18192=ORIENTED_EDGE('',*,*,#13656,.T.);
#18193=ORIENTED_EDGE('',*,*,#13657,.T.);
#18194=ORIENTED_EDGE('',*,*,#13658,.T.);
#18195=ORIENTED_EDGE('',*,*,#13659,.T.);
#18196=ORIENTED_EDGE('',*,*,#13660,.T.);
#18197=ORIENTED_EDGE('',*,*,#13661,.T.);
#18198=ORIENTED_EDGE('',*,*,#13662,.T.);
#18199=ORIENTED_EDGE('',*,*,#13663,.T.);
#18200=ORIENTED_EDGE('',*,*,#13664,.T.);
#18201=ORIENTED_EDGE('',*,*,#13665,.T.);
#18202=ORIENTED_EDGE('',*,*,#13666,.T.);
#18203=ORIENTED_EDGE('',*,*,#13667,.T.);
#18204=ORIENTED_EDGE('',*,*,#13668,.T.);
#18205=ORIENTED_EDGE('',*,*,#13669,.T.);
#18206=ORIENTED_EDGE('',*,*,#13670,.T.);
#18207=ORIENTED_EDGE('',*,*,#13671,.T.);
#18208=ORIENTED_EDGE('',*,*,#13672,.T.);
#18209=ORIENTED_EDGE('',*,*,#13673,.T.);
#18210=ORIENTED_EDGE('',*,*,#13674,.T.);
#18211=ORIENTED_EDGE('',*,*,#13675,.T.);
#18212=ORIENTED_EDGE('',*,*,#13676,.T.);
#18213=ORIENTED_EDGE('',*,*,#13677,.T.);
#18214=ORIENTED_EDGE('',*,*,#13641,.F.);
#18215=ORIENTED_EDGE('',*,*,#13678,.F.);
#18216=ORIENTED_EDGE('',*,*,#13676,.F.);
#18217=ORIENTED_EDGE('',*,*,#13679,.T.);
#18218=ORIENTED_EDGE('',*,*,#13640,.F.);
#18219=ORIENTED_EDGE('',*,*,#13680,.F.);
#18220=ORIENTED_EDGE('',*,*,#13677,.F.);
#18221=ORIENTED_EDGE('',*,*,#13678,.T.);
#18222=ORIENTED_EDGE('',*,*,#13642,.F.);
#18223=ORIENTED_EDGE('',*,*,#13679,.F.);
#18224=ORIENTED_EDGE('',*,*,#13675,.F.);
#18225=ORIENTED_EDGE('',*,*,#13681,.T.);
#18226=ORIENTED_EDGE('',*,*,#13643,.F.);
#18227=ORIENTED_EDGE('',*,*,#13681,.F.);
#18228=ORIENTED_EDGE('',*,*,#13674,.F.);
#18229=ORIENTED_EDGE('',*,*,#13682,.T.);
#18230=ORIENTED_EDGE('',*,*,#13644,.F.);
#18231=ORIENTED_EDGE('',*,*,#13682,.F.);
#18232=ORIENTED_EDGE('',*,*,#13673,.F.);
#18233=ORIENTED_EDGE('',*,*,#13683,.T.);
#18234=ORIENTED_EDGE('',*,*,#13645,.F.);
#18235=ORIENTED_EDGE('',*,*,#13683,.F.);
#18236=ORIENTED_EDGE('',*,*,#13672,.F.);
#18237=ORIENTED_EDGE('',*,*,#13684,.T.);
#18238=ORIENTED_EDGE('',*,*,#13646,.F.);
#18239=ORIENTED_EDGE('',*,*,#13684,.F.);
#18240=ORIENTED_EDGE('',*,*,#13671,.F.);
#18241=ORIENTED_EDGE('',*,*,#13685,.T.);
#18242=ORIENTED_EDGE('',*,*,#13639,.F.);
#18243=ORIENTED_EDGE('',*,*,#13685,.F.);
#18244=ORIENTED_EDGE('',*,*,#13670,.F.);
#18245=ORIENTED_EDGE('',*,*,#13680,.T.);
#18246=ORIENTED_EDGE('',*,*,#13655,.F.);
#18247=ORIENTED_EDGE('',*,*,#13686,.F.);
#18248=ORIENTED_EDGE('',*,*,#13687,.F.);
#18249=ORIENTED_EDGE('',*,*,#13688,.T.);
#18250=ORIENTED_EDGE('',*,*,#13654,.F.);
#18251=ORIENTED_EDGE('',*,*,#13689,.F.);
#18252=ORIENTED_EDGE('',*,*,#13690,.F.);
#18253=ORIENTED_EDGE('',*,*,#13686,.T.);
#18254=ORIENTED_EDGE('',*,*,#13653,.F.);
#18255=ORIENTED_EDGE('',*,*,#13691,.F.);
#18256=ORIENTED_EDGE('',*,*,#13692,.F.);
#18257=ORIENTED_EDGE('',*,*,#13689,.T.);
#18258=ORIENTED_EDGE('',*,*,#13662,.F.);
#18259=ORIENTED_EDGE('',*,*,#13693,.F.);
#18260=ORIENTED_EDGE('',*,*,#13694,.F.);
#18261=ORIENTED_EDGE('',*,*,#13695,.T.);
#18262=ORIENTED_EDGE('',*,*,#13661,.F.);
#18263=ORIENTED_EDGE('',*,*,#13696,.F.);
#18264=ORIENTED_EDGE('',*,*,#13697,.F.);
#18265=ORIENTED_EDGE('',*,*,#13693,.T.);
#18266=ORIENTED_EDGE('',*,*,#13660,.F.);
#18267=ORIENTED_EDGE('',*,*,#13698,.F.);
#18268=ORIENTED_EDGE('',*,*,#13699,.F.);
#18269=ORIENTED_EDGE('',*,*,#13696,.T.);
#18270=ORIENTED_EDGE('',*,*,#13659,.F.);
#18271=ORIENTED_EDGE('',*,*,#13700,.F.);
#18272=ORIENTED_EDGE('',*,*,#13701,.F.);
#18273=ORIENTED_EDGE('',*,*,#13698,.T.);
#18274=ORIENTED_EDGE('',*,*,#13658,.F.);
#18275=ORIENTED_EDGE('',*,*,#13702,.F.);
#18276=ORIENTED_EDGE('',*,*,#13703,.F.);
#18277=ORIENTED_EDGE('',*,*,#13700,.T.);
#18278=ORIENTED_EDGE('',*,*,#13657,.F.);
#18279=ORIENTED_EDGE('',*,*,#13704,.F.);
#18280=ORIENTED_EDGE('',*,*,#13705,.F.);
#18281=ORIENTED_EDGE('',*,*,#13702,.T.);
#18282=ORIENTED_EDGE('',*,*,#13656,.F.);
#18283=ORIENTED_EDGE('',*,*,#13688,.F.);
#18284=ORIENTED_EDGE('',*,*,#13706,.F.);
#18285=ORIENTED_EDGE('',*,*,#13704,.T.);
#18286=ORIENTED_EDGE('',*,*,#13663,.F.);
#18287=ORIENTED_EDGE('',*,*,#13695,.F.);
#18288=ORIENTED_EDGE('',*,*,#13707,.F.);
#18289=ORIENTED_EDGE('',*,*,#13691,.T.);
#18290=ORIENTED_EDGE('',*,*,#13692,.T.);
#18291=ORIENTED_EDGE('',*,*,#13707,.T.);
#18292=ORIENTED_EDGE('',*,*,#13694,.T.);
#18293=ORIENTED_EDGE('',*,*,#13697,.T.);
#18294=ORIENTED_EDGE('',*,*,#13699,.T.);
#18295=ORIENTED_EDGE('',*,*,#13701,.T.);
#18296=ORIENTED_EDGE('',*,*,#13703,.T.);
#18297=ORIENTED_EDGE('',*,*,#13705,.T.);
#18298=ORIENTED_EDGE('',*,*,#13706,.T.);
#18299=ORIENTED_EDGE('',*,*,#13687,.T.);
#18300=ORIENTED_EDGE('',*,*,#13690,.T.);
#18301=ORIENTED_EDGE('',*,*,#13708,.T.);
#18302=ORIENTED_EDGE('',*,*,#13709,.T.);
#18303=ORIENTED_EDGE('',*,*,#13710,.T.);
#18304=ORIENTED_EDGE('',*,*,#13711,.T.);
#18305=ORIENTED_EDGE('',*,*,#13712,.T.);
#18306=ORIENTED_EDGE('',*,*,#13713,.T.);
#18307=ORIENTED_EDGE('',*,*,#13649,.F.);
#18308=ORIENTED_EDGE('',*,*,#13714,.F.);
#18309=ORIENTED_EDGE('',*,*,#13710,.F.);
#18310=ORIENTED_EDGE('',*,*,#13715,.T.);
#18311=ORIENTED_EDGE('',*,*,#13648,.F.);
#18312=ORIENTED_EDGE('',*,*,#13716,.F.);
#18313=ORIENTED_EDGE('',*,*,#13711,.F.);
#18314=ORIENTED_EDGE('',*,*,#13714,.T.);
#18315=ORIENTED_EDGE('',*,*,#13650,.F.);
#18316=ORIENTED_EDGE('',*,*,#13715,.F.);
#18317=ORIENTED_EDGE('',*,*,#13709,.F.);
#18318=ORIENTED_EDGE('',*,*,#13717,.T.);
#18319=ORIENTED_EDGE('',*,*,#13651,.F.);
#18320=ORIENTED_EDGE('',*,*,#13717,.F.);
#18321=ORIENTED_EDGE('',*,*,#13708,.F.);
#18322=ORIENTED_EDGE('',*,*,#13718,.T.);
#18323=ORIENTED_EDGE('',*,*,#13652,.F.);
#18324=ORIENTED_EDGE('',*,*,#13718,.F.);
#18325=ORIENTED_EDGE('',*,*,#13713,.F.);
#18326=ORIENTED_EDGE('',*,*,#13719,.T.);
#18327=ORIENTED_EDGE('',*,*,#13647,.F.);
#18328=ORIENTED_EDGE('',*,*,#13719,.F.);
#18329=ORIENTED_EDGE('',*,*,#13712,.F.);
#18330=ORIENTED_EDGE('',*,*,#13716,.T.);
#18331=ORIENTED_EDGE('',*,*,#13668,.F.);
#18332=ORIENTED_EDGE('',*,*,#13720,.F.);
#18333=ORIENTED_EDGE('',*,*,#13721,.F.);
#18334=ORIENTED_EDGE('',*,*,#13722,.T.);
#18335=ORIENTED_EDGE('',*,*,#13667,.F.);
#18336=ORIENTED_EDGE('',*,*,#13723,.F.);
#18337=ORIENTED_EDGE('',*,*,#13724,.F.);
#18338=ORIENTED_EDGE('',*,*,#13720,.T.);
#18339=ORIENTED_EDGE('',*,*,#13666,.F.);
#18340=ORIENTED_EDGE('',*,*,#13725,.F.);
#18341=ORIENTED_EDGE('',*,*,#13726,.F.);
#18342=ORIENTED_EDGE('',*,*,#13723,.T.);
#18343=ORIENTED_EDGE('',*,*,#13665,.F.);
#18344=ORIENTED_EDGE('',*,*,#13727,.F.);
#18345=ORIENTED_EDGE('',*,*,#13728,.F.);
#18346=ORIENTED_EDGE('',*,*,#13725,.T.);
#18347=ORIENTED_EDGE('',*,*,#13669,.F.);
#18348=ORIENTED_EDGE('',*,*,#13722,.F.);
#18349=ORIENTED_EDGE('',*,*,#13729,.F.);
#18350=ORIENTED_EDGE('',*,*,#13730,.T.);
#18351=ORIENTED_EDGE('',*,*,#13664,.F.);
#18352=ORIENTED_EDGE('',*,*,#13730,.F.);
#18353=ORIENTED_EDGE('',*,*,#13731,.F.);
#18354=ORIENTED_EDGE('',*,*,#13727,.T.);
#18355=ORIENTED_EDGE('',*,*,#13726,.T.);
#18356=ORIENTED_EDGE('',*,*,#13728,.T.);
#18357=ORIENTED_EDGE('',*,*,#13731,.T.);
#18358=ORIENTED_EDGE('',*,*,#13729,.T.);
#18359=ORIENTED_EDGE('',*,*,#13721,.T.);
#18360=ORIENTED_EDGE('',*,*,#13724,.T.);
#18361=ORIENTED_EDGE('',*,*,#13633,.F.);
#18362=ORIENTED_EDGE('',*,*,#13732,.F.);
#18363=ORIENTED_EDGE('',*,*,#13733,.F.);
#18364=ORIENTED_EDGE('',*,*,#13734,.T.);
#18365=ORIENTED_EDGE('',*,*,#13632,.F.);
#18366=ORIENTED_EDGE('',*,*,#13735,.F.);
#18367=ORIENTED_EDGE('',*,*,#13736,.F.);
#18368=ORIENTED_EDGE('',*,*,#13732,.T.);
#18369=ORIENTED_EDGE('',*,*,#13631,.F.);
#18370=ORIENTED_EDGE('',*,*,#13737,.F.);
#18371=ORIENTED_EDGE('',*,*,#13738,.F.);
#18372=ORIENTED_EDGE('',*,*,#13735,.T.);
#18373=ORIENTED_EDGE('',*,*,#13630,.F.);
#18374=ORIENTED_EDGE('',*,*,#13739,.F.);
#18375=ORIENTED_EDGE('',*,*,#13740,.F.);
#18376=ORIENTED_EDGE('',*,*,#13737,.T.);
#18377=ORIENTED_EDGE('',*,*,#13638,.F.);
#18378=ORIENTED_EDGE('',*,*,#13741,.F.);
#18379=ORIENTED_EDGE('',*,*,#13742,.F.);
#18380=ORIENTED_EDGE('',*,*,#13739,.T.);
#18381=ORIENTED_EDGE('',*,*,#13581,.F.);
#18382=ORIENTED_EDGE('',*,*,#13743,.F.);
#18383=ORIENTED_EDGE('',*,*,#13744,.F.);
#18384=ORIENTED_EDGE('',*,*,#13745,.T.);
#18385=ORIENTED_EDGE('',*,*,#13580,.F.);
#18386=ORIENTED_EDGE('',*,*,#13746,.F.);
#18387=ORIENTED_EDGE('',*,*,#13747,.F.);
#18388=ORIENTED_EDGE('',*,*,#13743,.T.);
#18389=ORIENTED_EDGE('',*,*,#13637,.F.);
#18390=ORIENTED_EDGE('',*,*,#13748,.F.);
#18391=ORIENTED_EDGE('',*,*,#13749,.F.);
#18392=ORIENTED_EDGE('',*,*,#13741,.T.);
#18393=ORIENTED_EDGE('',*,*,#13636,.F.);
#18394=ORIENTED_EDGE('',*,*,#13750,.F.);
#18395=ORIENTED_EDGE('',*,*,#13751,.F.);
#18396=ORIENTED_EDGE('',*,*,#13748,.T.);
#18397=ORIENTED_EDGE('',*,*,#13635,.F.);
#18398=ORIENTED_EDGE('',*,*,#13752,.F.);
#18399=ORIENTED_EDGE('',*,*,#13753,.F.);
#18400=ORIENTED_EDGE('',*,*,#13750,.T.);
#18401=ORIENTED_EDGE('',*,*,#13634,.F.);
#18402=ORIENTED_EDGE('',*,*,#13734,.F.);
#18403=ORIENTED_EDGE('',*,*,#13754,.F.);
#18404=ORIENTED_EDGE('',*,*,#13752,.T.);
#18405=ORIENTED_EDGE('',*,*,#13579,.F.);
#18406=ORIENTED_EDGE('',*,*,#13755,.F.);
#18407=ORIENTED_EDGE('',*,*,#13756,.F.);
#18408=ORIENTED_EDGE('',*,*,#13746,.T.);
#18409=ORIENTED_EDGE('',*,*,#13578,.F.);
#18410=ORIENTED_EDGE('',*,*,#13745,.F.);
#18411=ORIENTED_EDGE('',*,*,#13757,.F.);
#18412=ORIENTED_EDGE('',*,*,#13755,.T.);
#18413=ORIENTED_EDGE('',*,*,#13740,.T.);
#18414=ORIENTED_EDGE('',*,*,#13742,.T.);
#18415=ORIENTED_EDGE('',*,*,#13749,.T.);
#18416=ORIENTED_EDGE('',*,*,#13751,.T.);
#18417=ORIENTED_EDGE('',*,*,#13753,.T.);
#18418=ORIENTED_EDGE('',*,*,#13754,.T.);
#18419=ORIENTED_EDGE('',*,*,#13733,.T.);
#18420=ORIENTED_EDGE('',*,*,#13736,.T.);
#18421=ORIENTED_EDGE('',*,*,#13738,.T.);
#18422=ORIENTED_EDGE('',*,*,#13747,.T.);
#18423=ORIENTED_EDGE('',*,*,#13756,.T.);
#18424=ORIENTED_EDGE('',*,*,#13757,.T.);
#18425=ORIENTED_EDGE('',*,*,#13744,.T.);
#18426=ORIENTED_EDGE('',*,*,#13758,.T.);
#18427=ORIENTED_EDGE('',*,*,#13759,.T.);
#18428=ORIENTED_EDGE('',*,*,#13760,.T.);
#18429=ORIENTED_EDGE('',*,*,#13761,.T.);
#18430=ORIENTED_EDGE('',*,*,#13762,.T.);
#18431=ORIENTED_EDGE('',*,*,#13763,.T.);
#18432=ORIENTED_EDGE('',*,*,#13764,.T.);
#18433=ORIENTED_EDGE('',*,*,#13765,.T.);
#18434=ORIENTED_EDGE('',*,*,#13758,.F.);
#18435=ORIENTED_EDGE('',*,*,#13766,.T.);
#18436=ORIENTED_EDGE('',*,*,#13765,.F.);
#18437=ORIENTED_EDGE('',*,*,#13766,.F.);
#18438=ORIENTED_EDGE('',*,*,#13767,.F.);
#18439=ORIENTED_EDGE('',*,*,#13768,.F.);
#18440=ORIENTED_EDGE('',*,*,#13769,.F.);
#18441=ORIENTED_EDGE('',*,*,#13770,.F.);
#18442=ORIENTED_EDGE('',*,*,#13771,.F.);
#18443=ORIENTED_EDGE('',*,*,#13772,.F.);
#18444=ORIENTED_EDGE('',*,*,#13764,.F.);
#18445=ORIENTED_EDGE('',*,*,#13773,.F.);
#18446=ORIENTED_EDGE('',*,*,#13767,.T.);
#18447=ORIENTED_EDGE('',*,*,#13774,.T.);
#18448=ORIENTED_EDGE('',*,*,#13763,.F.);
#18449=ORIENTED_EDGE('',*,*,#13775,.F.);
#18450=ORIENTED_EDGE('',*,*,#13768,.T.);
#18451=ORIENTED_EDGE('',*,*,#13773,.T.);
#18452=ORIENTED_EDGE('',*,*,#13762,.F.);
#18453=ORIENTED_EDGE('',*,*,#13776,.F.);
#18454=ORIENTED_EDGE('',*,*,#13769,.T.);
#18455=ORIENTED_EDGE('',*,*,#13775,.T.);
#18456=ORIENTED_EDGE('',*,*,#13761,.F.);
#18457=ORIENTED_EDGE('',*,*,#13777,.F.);
#18458=ORIENTED_EDGE('',*,*,#13770,.T.);
#18459=ORIENTED_EDGE('',*,*,#13776,.T.);
#18460=ORIENTED_EDGE('',*,*,#13760,.F.);
#18461=ORIENTED_EDGE('',*,*,#13778,.F.);
#18462=ORIENTED_EDGE('',*,*,#13771,.T.);
#18463=ORIENTED_EDGE('',*,*,#13777,.T.);
#18464=ORIENTED_EDGE('',*,*,#13759,.F.);
#18465=ORIENTED_EDGE('',*,*,#13774,.F.);
#18466=ORIENTED_EDGE('',*,*,#13772,.T.);
#18467=ORIENTED_EDGE('',*,*,#13778,.T.);
#18468=ORIENTED_EDGE('',*,*,#13779,.T.);
#18469=ORIENTED_EDGE('',*,*,#13780,.F.);
#18470=ORIENTED_EDGE('',*,*,#13781,.T.);
#18471=ORIENTED_EDGE('',*,*,#13782,.T.);
#18472=ORIENTED_EDGE('',*,*,#13783,.T.);
#18473=ORIENTED_EDGE('',*,*,#13784,.T.);
#18474=ORIENTED_EDGE('',*,*,#13785,.T.);
#18475=ORIENTED_EDGE('',*,*,#13786,.T.);
#18476=ORIENTED_EDGE('',*,*,#13787,.T.);
#18477=ORIENTED_EDGE('',*,*,#13788,.T.);
#18478=ORIENTED_EDGE('',*,*,#13789,.T.);
#18479=ORIENTED_EDGE('',*,*,#13783,.F.);
#18480=ORIENTED_EDGE('',*,*,#13789,.F.);
#18481=ORIENTED_EDGE('',*,*,#13790,.T.);
#18482=ORIENTED_EDGE('',*,*,#13791,.T.);
#18483=ORIENTED_EDGE('',*,*,#13792,.T.);
#18484=ORIENTED_EDGE('',*,*,#13793,.T.);
#18485=ORIENTED_EDGE('',*,*,#13794,.T.);
#18486=ORIENTED_EDGE('',*,*,#13795,.F.);
#18487=ORIENTED_EDGE('',*,*,#13796,.T.);
#18488=ORIENTED_EDGE('',*,*,#13797,.T.);
#18489=ORIENTED_EDGE('',*,*,#13798,.T.);
#18490=ORIENTED_EDGE('',*,*,#13799,.T.);
#18491=ORIENTED_EDGE('',*,*,#13800,.T.);
#18492=ORIENTED_EDGE('',*,*,#13801,.F.);
#18493=ORIENTED_EDGE('',*,*,#13802,.T.);
#18494=ORIENTED_EDGE('',*,*,#13803,.F.);
#18495=ORIENTED_EDGE('',*,*,#13779,.F.);
#18496=ORIENTED_EDGE('',*,*,#13804,.F.);
#18497=ORIENTED_EDGE('',*,*,#13799,.F.);
#18498=ORIENTED_EDGE('',*,*,#13805,.T.);
#18499=ORIENTED_EDGE('',*,*,#13806,.T.);
#18500=ORIENTED_EDGE('',*,*,#13807,.T.);
#18501=ORIENTED_EDGE('',*,*,#13808,.T.);
#18502=ORIENTED_EDGE('',*,*,#13809,.T.);
#18503=ORIENTED_EDGE('',*,*,#13810,.T.);
#18504=ORIENTED_EDGE('',*,*,#13797,.F.);
#18505=ORIENTED_EDGE('',*,*,#13804,.T.);
#18506=ORIENTED_EDGE('',*,*,#13782,.F.);
#18507=ORIENTED_EDGE('',*,*,#13811,.T.);
#18508=ORIENTED_EDGE('',*,*,#13812,.T.);
#18509=ORIENTED_EDGE('',*,*,#13796,.F.);
#18510=ORIENTED_EDGE('',*,*,#13813,.F.);
#18511=ORIENTED_EDGE('',*,*,#13814,.T.);
#18512=ORIENTED_EDGE('',*,*,#13808,.F.);
#18513=ORIENTED_EDGE('',*,*,#13815,.T.);
#18514=ORIENTED_EDGE('',*,*,#13816,.F.);
#18515=ORIENTED_EDGE('',*,*,#13800,.F.);
#18516=ORIENTED_EDGE('',*,*,#13807,.F.);
#18517=ORIENTED_EDGE('',*,*,#13817,.F.);
#18518=ORIENTED_EDGE('',*,*,#13802,.F.);
#18519=ORIENTED_EDGE('',*,*,#13812,.F.);
#18520=ORIENTED_EDGE('',*,*,#13818,.F.);
#18521=ORIENTED_EDGE('',*,*,#13819,.F.);
#18522=ORIENTED_EDGE('',*,*,#13820,.F.);
#18523=ORIENTED_EDGE('',*,*,#13821,.F.);
#18524=ORIENTED_EDGE('',*,*,#13809,.F.);
#18525=ORIENTED_EDGE('',*,*,#13814,.F.);
#18526=ORIENTED_EDGE('',*,*,#13822,.F.);
#18527=ORIENTED_EDGE('',*,*,#13815,.F.);
#18528=ORIENTED_EDGE('',*,*,#13806,.F.);
#18529=ORIENTED_EDGE('',*,*,#13823,.F.);
#18530=ORIENTED_EDGE('',*,*,#13824,.T.);
#18531=ORIENTED_EDGE('',*,*,#13825,.T.);
#18532=ORIENTED_EDGE('',*,*,#13826,.T.);
#18533=ORIENTED_EDGE('',*,*,#13827,.T.);
#18534=ORIENTED_EDGE('',*,*,#13781,.F.);
#18535=ORIENTED_EDGE('',*,*,#13828,.F.);
#18536=ORIENTED_EDGE('',*,*,#13818,.T.);
#18537=ORIENTED_EDGE('',*,*,#13811,.F.);
#18538=ORIENTED_EDGE('',*,*,#13821,.T.);
#18539=ORIENTED_EDGE('',*,*,#13829,.F.);
#18540=ORIENTED_EDGE('',*,*,#13794,.F.);
#18541=ORIENTED_EDGE('',*,*,#13810,.F.);
#18542=ORIENTED_EDGE('',*,*,#13798,.F.);
#18543=ORIENTED_EDGE('',*,*,#13830,.F.);
#18544=ORIENTED_EDGE('',*,*,#13823,.T.);
#18545=ORIENTED_EDGE('',*,*,#13805,.F.);
#18546=ORIENTED_EDGE('',*,*,#13825,.F.);
#18547=ORIENTED_EDGE('',*,*,#13831,.F.);
#18548=ORIENTED_EDGE('',*,*,#13832,.F.);
#18549=ORIENTED_EDGE('',*,*,#13833,.F.);
#18550=ORIENTED_EDGE('',*,*,#13787,.F.);
#18551=ORIENTED_EDGE('',*,*,#13834,.F.);
#18552=ORIENTED_EDGE('',*,*,#13835,.F.);
#18553=ORIENTED_EDGE('',*,*,#13836,.F.);
#18554=ORIENTED_EDGE('',*,*,#13837,.F.);
#18555=ORIENTED_EDGE('',*,*,#13838,.T.);
#18556=ORIENTED_EDGE('',*,*,#13826,.F.);
#18557=ORIENTED_EDGE('',*,*,#13836,.T.);
#18558=ORIENTED_EDGE('',*,*,#13839,.F.);
#18559=ORIENTED_EDGE('',*,*,#13834,.T.);
#18560=ORIENTED_EDGE('',*,*,#13786,.F.);
#18561=ORIENTED_EDGE('',*,*,#13840,.T.);
#18562=ORIENTED_EDGE('',*,*,#13841,.F.);
#18563=ORIENTED_EDGE('',*,*,#13842,.F.);
#18564=ORIENTED_EDGE('',*,*,#13827,.F.);
#18565=ORIENTED_EDGE('',*,*,#13838,.F.);
#18566=ORIENTED_EDGE('',*,*,#13843,.F.);
#18567=ORIENTED_EDGE('',*,*,#13840,.F.);
#18568=ORIENTED_EDGE('',*,*,#13785,.F.);
#18569=ORIENTED_EDGE('',*,*,#13844,.F.);
#18570=ORIENTED_EDGE('',*,*,#13845,.F.);
#18571=ORIENTED_EDGE('',*,*,#13846,.F.);
#18572=ORIENTED_EDGE('',*,*,#13831,.T.);
#18573=ORIENTED_EDGE('',*,*,#13824,.F.);
#18574=ORIENTED_EDGE('',*,*,#13842,.T.);
#18575=ORIENTED_EDGE('',*,*,#13847,.F.);
#18576=ORIENTED_EDGE('',*,*,#13844,.T.);
#18577=ORIENTED_EDGE('',*,*,#13784,.F.);
#18578=ORIENTED_EDGE('',*,*,#13833,.T.);
#18579=ORIENTED_EDGE('',*,*,#13843,.T.);
#18580=ORIENTED_EDGE('',*,*,#13848,.T.);
#18581=ORIENTED_EDGE('',*,*,#13849,.F.);
#18582=ORIENTED_EDGE('',*,*,#13850,.F.);
#18583=ORIENTED_EDGE('',*,*,#13851,.F.);
#18584=ORIENTED_EDGE('',*,*,#13848,.F.);
#18585=ORIENTED_EDGE('',*,*,#13845,.T.);
#18586=ORIENTED_EDGE('',*,*,#13847,.T.);
#18587=ORIENTED_EDGE('',*,*,#13832,.T.);
#18588=ORIENTED_EDGE('',*,*,#13846,.T.);
#18589=ORIENTED_EDGE('',*,*,#13841,.T.);
#18590=ORIENTED_EDGE('',*,*,#13837,.T.);
#18591=ORIENTED_EDGE('',*,*,#13835,.T.);
#18592=ORIENTED_EDGE('',*,*,#13839,.T.);
#18593=ORIENTED_EDGE('',*,*,#13788,.F.);
#18594=ORIENTED_EDGE('',*,*,#13852,.T.);
#18595=ORIENTED_EDGE('',*,*,#13851,.T.);
#18596=ORIENTED_EDGE('',*,*,#13850,.T.);
#18597=ORIENTED_EDGE('',*,*,#13853,.T.);
#18598=ORIENTED_EDGE('',*,*,#13819,.T.);
#18599=ORIENTED_EDGE('',*,*,#13828,.T.);
#18600=ORIENTED_EDGE('',*,*,#13780,.T.);
#18601=ORIENTED_EDGE('',*,*,#13803,.T.);
#18602=ORIENTED_EDGE('',*,*,#13817,.T.);
#18603=ORIENTED_EDGE('',*,*,#13830,.T.);
#18604=ORIENTED_EDGE('',*,*,#13801,.T.);
#18605=ORIENTED_EDGE('',*,*,#13816,.T.);
#18606=ORIENTED_EDGE('',*,*,#13822,.T.);
#18607=ORIENTED_EDGE('',*,*,#13813,.T.);
#18608=ORIENTED_EDGE('',*,*,#13795,.T.);
#18609=ORIENTED_EDGE('',*,*,#13829,.T.);
#18610=ORIENTED_EDGE('',*,*,#13820,.T.);
#18611=ORIENTED_EDGE('',*,*,#13853,.F.);
#18612=ORIENTED_EDGE('',*,*,#13849,.T.);
#18613=ORIENTED_EDGE('',*,*,#13852,.F.);
#18614=ORIENTED_EDGE('',*,*,#13854,.T.);
#18615=ORIENTED_EDGE('',*,*,#13855,.T.);
#18616=ORIENTED_EDGE('',*,*,#13856,.T.);
#18617=ORIENTED_EDGE('',*,*,#13857,.T.);
#18618=ORIENTED_EDGE('',*,*,#13858,.T.);
#18619=ORIENTED_EDGE('',*,*,#13859,.T.);
#18620=ORIENTED_EDGE('',*,*,#13860,.T.);
#18621=ORIENTED_EDGE('',*,*,#13861,.T.);
#18622=ORIENTED_EDGE('',*,*,#13862,.T.);
#18623=ORIENTED_EDGE('',*,*,#13863,.T.);
#18624=ORIENTED_EDGE('',*,*,#13864,.T.);
#18625=ORIENTED_EDGE('',*,*,#13865,.T.);
#18626=ORIENTED_EDGE('',*,*,#13866,.T.);
#18627=ORIENTED_EDGE('',*,*,#13867,.T.);
#18628=ORIENTED_EDGE('',*,*,#13868,.T.);
#18629=ORIENTED_EDGE('',*,*,#13869,.T.);
#18630=ORIENTED_EDGE('',*,*,#13870,.T.);
#18631=ORIENTED_EDGE('',*,*,#13871,.T.);
#18632=ORIENTED_EDGE('',*,*,#13872,.T.);
#18633=ORIENTED_EDGE('',*,*,#13873,.T.);
#18634=ORIENTED_EDGE('',*,*,#13874,.T.);
#18635=ORIENTED_EDGE('',*,*,#13875,.T.);
#18636=ORIENTED_EDGE('',*,*,#13876,.T.);
#18637=ORIENTED_EDGE('',*,*,#13877,.T.);
#18638=ORIENTED_EDGE('',*,*,#13878,.T.);
#18639=ORIENTED_EDGE('',*,*,#13879,.T.);
#18640=ORIENTED_EDGE('',*,*,#13880,.T.);
#18641=ORIENTED_EDGE('',*,*,#13881,.T.);
#18642=ORIENTED_EDGE('',*,*,#13882,.T.);
#18643=ORIENTED_EDGE('',*,*,#13883,.T.);
#18644=ORIENTED_EDGE('',*,*,#13884,.T.);
#18645=ORIENTED_EDGE('',*,*,#13885,.T.);
#18646=ORIENTED_EDGE('',*,*,#13886,.T.);
#18647=ORIENTED_EDGE('',*,*,#13887,.T.);
#18648=ORIENTED_EDGE('',*,*,#13888,.T.);
#18649=ORIENTED_EDGE('',*,*,#13889,.T.);
#18650=ORIENTED_EDGE('',*,*,#13890,.T.);
#18651=ORIENTED_EDGE('',*,*,#13891,.T.);
#18652=ORIENTED_EDGE('',*,*,#13892,.T.);
#18653=ORIENTED_EDGE('',*,*,#13893,.T.);
#18654=ORIENTED_EDGE('',*,*,#13894,.T.);
#18655=ORIENTED_EDGE('',*,*,#13895,.T.);
#18656=ORIENTED_EDGE('',*,*,#13896,.T.);
#18657=ORIENTED_EDGE('',*,*,#13897,.T.);
#18658=ORIENTED_EDGE('',*,*,#13898,.T.);
#18659=ORIENTED_EDGE('',*,*,#13899,.T.);
#18660=ORIENTED_EDGE('',*,*,#13900,.T.);
#18661=ORIENTED_EDGE('',*,*,#13901,.T.);
#18662=ORIENTED_EDGE('',*,*,#13865,.F.);
#18663=ORIENTED_EDGE('',*,*,#13902,.F.);
#18664=ORIENTED_EDGE('',*,*,#13900,.F.);
#18665=ORIENTED_EDGE('',*,*,#13903,.T.);
#18666=ORIENTED_EDGE('',*,*,#13864,.F.);
#18667=ORIENTED_EDGE('',*,*,#13904,.F.);
#18668=ORIENTED_EDGE('',*,*,#13901,.F.);
#18669=ORIENTED_EDGE('',*,*,#13902,.T.);
#18670=ORIENTED_EDGE('',*,*,#13866,.F.);
#18671=ORIENTED_EDGE('',*,*,#13903,.F.);
#18672=ORIENTED_EDGE('',*,*,#13899,.F.);
#18673=ORIENTED_EDGE('',*,*,#13905,.T.);
#18674=ORIENTED_EDGE('',*,*,#13867,.F.);
#18675=ORIENTED_EDGE('',*,*,#13905,.F.);
#18676=ORIENTED_EDGE('',*,*,#13898,.F.);
#18677=ORIENTED_EDGE('',*,*,#13906,.T.);
#18678=ORIENTED_EDGE('',*,*,#13868,.F.);
#18679=ORIENTED_EDGE('',*,*,#13906,.F.);
#18680=ORIENTED_EDGE('',*,*,#13897,.F.);
#18681=ORIENTED_EDGE('',*,*,#13907,.T.);
#18682=ORIENTED_EDGE('',*,*,#13869,.F.);
#18683=ORIENTED_EDGE('',*,*,#13907,.F.);
#18684=ORIENTED_EDGE('',*,*,#13896,.F.);
#18685=ORIENTED_EDGE('',*,*,#13908,.T.);
#18686=ORIENTED_EDGE('',*,*,#13870,.F.);
#18687=ORIENTED_EDGE('',*,*,#13908,.F.);
#18688=ORIENTED_EDGE('',*,*,#13895,.F.);
#18689=ORIENTED_EDGE('',*,*,#13909,.T.);
#18690=ORIENTED_EDGE('',*,*,#13863,.F.);
#18691=ORIENTED_EDGE('',*,*,#13909,.F.);
#18692=ORIENTED_EDGE('',*,*,#13894,.F.);
#18693=ORIENTED_EDGE('',*,*,#13904,.T.);
#18694=ORIENTED_EDGE('',*,*,#13879,.F.);
#18695=ORIENTED_EDGE('',*,*,#13910,.F.);
#18696=ORIENTED_EDGE('',*,*,#13911,.F.);
#18697=ORIENTED_EDGE('',*,*,#13912,.T.);
#18698=ORIENTED_EDGE('',*,*,#13878,.F.);
#18699=ORIENTED_EDGE('',*,*,#13913,.F.);
#18700=ORIENTED_EDGE('',*,*,#13914,.F.);
#18701=ORIENTED_EDGE('',*,*,#13910,.T.);
#18702=ORIENTED_EDGE('',*,*,#13877,.F.);
#18703=ORIENTED_EDGE('',*,*,#13915,.F.);
#18704=ORIENTED_EDGE('',*,*,#13916,.F.);
#18705=ORIENTED_EDGE('',*,*,#13913,.T.);
#18706=ORIENTED_EDGE('',*,*,#13886,.F.);
#18707=ORIENTED_EDGE('',*,*,#13917,.F.);
#18708=ORIENTED_EDGE('',*,*,#13918,.F.);
#18709=ORIENTED_EDGE('',*,*,#13919,.T.);
#18710=ORIENTED_EDGE('',*,*,#13885,.F.);
#18711=ORIENTED_EDGE('',*,*,#13920,.F.);
#18712=ORIENTED_EDGE('',*,*,#13921,.F.);
#18713=ORIENTED_EDGE('',*,*,#13917,.T.);
#18714=ORIENTED_EDGE('',*,*,#13884,.F.);
#18715=ORIENTED_EDGE('',*,*,#13922,.F.);
#18716=ORIENTED_EDGE('',*,*,#13923,.F.);
#18717=ORIENTED_EDGE('',*,*,#13920,.T.);
#18718=ORIENTED_EDGE('',*,*,#13883,.F.);
#18719=ORIENTED_EDGE('',*,*,#13924,.F.);
#18720=ORIENTED_EDGE('',*,*,#13925,.F.);
#18721=ORIENTED_EDGE('',*,*,#13922,.T.);
#18722=ORIENTED_EDGE('',*,*,#13882,.F.);
#18723=ORIENTED_EDGE('',*,*,#13926,.F.);
#18724=ORIENTED_EDGE('',*,*,#13927,.F.);
#18725=ORIENTED_EDGE('',*,*,#13924,.T.);
#18726=ORIENTED_EDGE('',*,*,#13881,.F.);
#18727=ORIENTED_EDGE('',*,*,#13928,.F.);
#18728=ORIENTED_EDGE('',*,*,#13929,.F.);
#18729=ORIENTED_EDGE('',*,*,#13926,.T.);
#18730=ORIENTED_EDGE('',*,*,#13880,.F.);
#18731=ORIENTED_EDGE('',*,*,#13912,.F.);
#18732=ORIENTED_EDGE('',*,*,#13930,.F.);
#18733=ORIENTED_EDGE('',*,*,#13928,.T.);
#18734=ORIENTED_EDGE('',*,*,#13887,.F.);
#18735=ORIENTED_EDGE('',*,*,#13919,.F.);
#18736=ORIENTED_EDGE('',*,*,#13931,.F.);
#18737=ORIENTED_EDGE('',*,*,#13915,.T.);
#18738=ORIENTED_EDGE('',*,*,#13916,.T.);
#18739=ORIENTED_EDGE('',*,*,#13931,.T.);
#18740=ORIENTED_EDGE('',*,*,#13918,.T.);
#18741=ORIENTED_EDGE('',*,*,#13921,.T.);
#18742=ORIENTED_EDGE('',*,*,#13923,.T.);
#18743=ORIENTED_EDGE('',*,*,#13925,.T.);
#18744=ORIENTED_EDGE('',*,*,#13927,.T.);
#18745=ORIENTED_EDGE('',*,*,#13929,.T.);
#18746=ORIENTED_EDGE('',*,*,#13930,.T.);
#18747=ORIENTED_EDGE('',*,*,#13911,.T.);
#18748=ORIENTED_EDGE('',*,*,#13914,.T.);
#18749=ORIENTED_EDGE('',*,*,#13932,.T.);
#18750=ORIENTED_EDGE('',*,*,#13933,.T.);
#18751=ORIENTED_EDGE('',*,*,#13934,.T.);
#18752=ORIENTED_EDGE('',*,*,#13935,.T.);
#18753=ORIENTED_EDGE('',*,*,#13936,.T.);
#18754=ORIENTED_EDGE('',*,*,#13937,.T.);
#18755=ORIENTED_EDGE('',*,*,#13873,.F.);
#18756=ORIENTED_EDGE('',*,*,#13938,.F.);
#18757=ORIENTED_EDGE('',*,*,#13934,.F.);
#18758=ORIENTED_EDGE('',*,*,#13939,.T.);
#18759=ORIENTED_EDGE('',*,*,#13872,.F.);
#18760=ORIENTED_EDGE('',*,*,#13940,.F.);
#18761=ORIENTED_EDGE('',*,*,#13935,.F.);
#18762=ORIENTED_EDGE('',*,*,#13938,.T.);
#18763=ORIENTED_EDGE('',*,*,#13874,.F.);
#18764=ORIENTED_EDGE('',*,*,#13939,.F.);
#18765=ORIENTED_EDGE('',*,*,#13933,.F.);
#18766=ORIENTED_EDGE('',*,*,#13941,.T.);
#18767=ORIENTED_EDGE('',*,*,#13875,.F.);
#18768=ORIENTED_EDGE('',*,*,#13941,.F.);
#18769=ORIENTED_EDGE('',*,*,#13932,.F.);
#18770=ORIENTED_EDGE('',*,*,#13942,.T.);
#18771=ORIENTED_EDGE('',*,*,#13876,.F.);
#18772=ORIENTED_EDGE('',*,*,#13942,.F.);
#18773=ORIENTED_EDGE('',*,*,#13937,.F.);
#18774=ORIENTED_EDGE('',*,*,#13943,.T.);
#18775=ORIENTED_EDGE('',*,*,#13871,.F.);
#18776=ORIENTED_EDGE('',*,*,#13943,.F.);
#18777=ORIENTED_EDGE('',*,*,#13936,.F.);
#18778=ORIENTED_EDGE('',*,*,#13940,.T.);
#18779=ORIENTED_EDGE('',*,*,#13892,.F.);
#18780=ORIENTED_EDGE('',*,*,#13944,.F.);
#18781=ORIENTED_EDGE('',*,*,#13945,.F.);
#18782=ORIENTED_EDGE('',*,*,#13946,.T.);
#18783=ORIENTED_EDGE('',*,*,#13891,.F.);
#18784=ORIENTED_EDGE('',*,*,#13947,.F.);
#18785=ORIENTED_EDGE('',*,*,#13948,.F.);
#18786=ORIENTED_EDGE('',*,*,#13944,.T.);
#18787=ORIENTED_EDGE('',*,*,#13890,.F.);
#18788=ORIENTED_EDGE('',*,*,#13949,.F.);
#18789=ORIENTED_EDGE('',*,*,#13950,.F.);
#18790=ORIENTED_EDGE('',*,*,#13947,.T.);
#18791=ORIENTED_EDGE('',*,*,#13889,.F.);
#18792=ORIENTED_EDGE('',*,*,#13951,.F.);
#18793=ORIENTED_EDGE('',*,*,#13952,.F.);
#18794=ORIENTED_EDGE('',*,*,#13949,.T.);
#18795=ORIENTED_EDGE('',*,*,#13893,.F.);
#18796=ORIENTED_EDGE('',*,*,#13946,.F.);
#18797=ORIENTED_EDGE('',*,*,#13953,.F.);
#18798=ORIENTED_EDGE('',*,*,#13954,.T.);
#18799=ORIENTED_EDGE('',*,*,#13888,.F.);
#18800=ORIENTED_EDGE('',*,*,#13954,.F.);
#18801=ORIENTED_EDGE('',*,*,#13955,.F.);
#18802=ORIENTED_EDGE('',*,*,#13951,.T.);
#18803=ORIENTED_EDGE('',*,*,#13950,.T.);
#18804=ORIENTED_EDGE('',*,*,#13952,.T.);
#18805=ORIENTED_EDGE('',*,*,#13955,.T.);
#18806=ORIENTED_EDGE('',*,*,#13953,.T.);
#18807=ORIENTED_EDGE('',*,*,#13945,.T.);
#18808=ORIENTED_EDGE('',*,*,#13948,.T.);
#18809=ORIENTED_EDGE('',*,*,#13857,.F.);
#18810=ORIENTED_EDGE('',*,*,#13956,.F.);
#18811=ORIENTED_EDGE('',*,*,#13957,.F.);
#18812=ORIENTED_EDGE('',*,*,#13958,.T.);
#18813=ORIENTED_EDGE('',*,*,#13856,.F.);
#18814=ORIENTED_EDGE('',*,*,#13959,.F.);
#18815=ORIENTED_EDGE('',*,*,#13960,.F.);
#18816=ORIENTED_EDGE('',*,*,#13956,.T.);
#18817=ORIENTED_EDGE('',*,*,#13855,.F.);
#18818=ORIENTED_EDGE('',*,*,#13961,.F.);
#18819=ORIENTED_EDGE('',*,*,#13962,.F.);
#18820=ORIENTED_EDGE('',*,*,#13959,.T.);
#18821=ORIENTED_EDGE('',*,*,#13854,.F.);
#18822=ORIENTED_EDGE('',*,*,#13963,.F.);
#18823=ORIENTED_EDGE('',*,*,#13964,.F.);
#18824=ORIENTED_EDGE('',*,*,#13961,.T.);
#18825=ORIENTED_EDGE('',*,*,#13862,.F.);
#18826=ORIENTED_EDGE('',*,*,#13965,.F.);
#18827=ORIENTED_EDGE('',*,*,#13966,.F.);
#18828=ORIENTED_EDGE('',*,*,#13963,.T.);
#18829=ORIENTED_EDGE('',*,*,#13793,.F.);
#18830=ORIENTED_EDGE('',*,*,#13967,.F.);
#18831=ORIENTED_EDGE('',*,*,#13968,.F.);
#18832=ORIENTED_EDGE('',*,*,#13969,.T.);
#18833=ORIENTED_EDGE('',*,*,#13792,.F.);
#18834=ORIENTED_EDGE('',*,*,#13970,.F.);
#18835=ORIENTED_EDGE('',*,*,#13971,.F.);
#18836=ORIENTED_EDGE('',*,*,#13967,.T.);
#18837=ORIENTED_EDGE('',*,*,#13861,.F.);
#18838=ORIENTED_EDGE('',*,*,#13972,.F.);
#18839=ORIENTED_EDGE('',*,*,#13973,.F.);
#18840=ORIENTED_EDGE('',*,*,#13965,.T.);
#18841=ORIENTED_EDGE('',*,*,#13860,.F.);
#18842=ORIENTED_EDGE('',*,*,#13974,.F.);
#18843=ORIENTED_EDGE('',*,*,#13975,.F.);
#18844=ORIENTED_EDGE('',*,*,#13972,.T.);
#18845=ORIENTED_EDGE('',*,*,#13859,.F.);
#18846=ORIENTED_EDGE('',*,*,#13976,.F.);
#18847=ORIENTED_EDGE('',*,*,#13977,.F.);
#18848=ORIENTED_EDGE('',*,*,#13974,.T.);
#18849=ORIENTED_EDGE('',*,*,#13858,.F.);
#18850=ORIENTED_EDGE('',*,*,#13958,.F.);
#18851=ORIENTED_EDGE('',*,*,#13978,.F.);
#18852=ORIENTED_EDGE('',*,*,#13976,.T.);
#18853=ORIENTED_EDGE('',*,*,#13791,.F.);
#18854=ORIENTED_EDGE('',*,*,#13979,.F.);
#18855=ORIENTED_EDGE('',*,*,#13980,.F.);
#18856=ORIENTED_EDGE('',*,*,#13970,.T.);
#18857=ORIENTED_EDGE('',*,*,#13790,.F.);
#18858=ORIENTED_EDGE('',*,*,#13969,.F.);
#18859=ORIENTED_EDGE('',*,*,#13981,.F.);
#18860=ORIENTED_EDGE('',*,*,#13979,.T.);
#18861=ORIENTED_EDGE('',*,*,#13964,.T.);
#18862=ORIENTED_EDGE('',*,*,#13966,.T.);
#18863=ORIENTED_EDGE('',*,*,#13973,.T.);
#18864=ORIENTED_EDGE('',*,*,#13975,.T.);
#18865=ORIENTED_EDGE('',*,*,#13977,.T.);
#18866=ORIENTED_EDGE('',*,*,#13978,.T.);
#18867=ORIENTED_EDGE('',*,*,#13957,.T.);
#18868=ORIENTED_EDGE('',*,*,#13960,.T.);
#18869=ORIENTED_EDGE('',*,*,#13962,.T.);
#18870=ORIENTED_EDGE('',*,*,#13971,.T.);
#18871=ORIENTED_EDGE('',*,*,#13980,.T.);
#18872=ORIENTED_EDGE('',*,*,#13981,.T.);
#18873=ORIENTED_EDGE('',*,*,#13968,.T.);
#18874=ORIENTED_EDGE('',*,*,#13982,.F.);
#18875=ORIENTED_EDGE('',*,*,#13983,.T.);
#18876=ORIENTED_EDGE('',*,*,#13984,.T.);
#18877=ORIENTED_EDGE('',*,*,#13983,.F.);
#18878=ORIENTED_EDGE('',*,*,#13985,.F.);
#18879=ORIENTED_EDGE('',*,*,#13986,.T.);
#18880=ORIENTED_EDGE('',*,*,#13987,.T.);
#18881=ORIENTED_EDGE('',*,*,#13986,.F.);
#18882=ORIENTED_EDGE('',*,*,#13988,.F.);
#18883=ORIENTED_EDGE('',*,*,#13989,.T.);
#18884=ORIENTED_EDGE('',*,*,#13990,.T.);
#18885=ORIENTED_EDGE('',*,*,#13989,.F.);
#18886=ORIENTED_EDGE('',*,*,#13991,.F.);
#18887=ORIENTED_EDGE('',*,*,#13992,.T.);
#18888=ORIENTED_EDGE('',*,*,#13993,.T.);
#18889=ORIENTED_EDGE('',*,*,#13992,.F.);
#18890=ORIENTED_EDGE('',*,*,#13994,.F.);
#18891=ORIENTED_EDGE('',*,*,#13995,.T.);
#18892=ORIENTED_EDGE('',*,*,#13996,.T.);
#18893=ORIENTED_EDGE('',*,*,#13995,.F.);
#18894=ORIENTED_EDGE('',*,*,#13997,.F.);
#18895=ORIENTED_EDGE('',*,*,#13998,.T.);
#18896=ORIENTED_EDGE('',*,*,#13999,.T.);
#18897=ORIENTED_EDGE('',*,*,#13998,.F.);
#18898=ORIENTED_EDGE('',*,*,#14000,.F.);
#18899=ORIENTED_EDGE('',*,*,#14001,.T.);
#18900=ORIENTED_EDGE('',*,*,#14002,.T.);
#18901=ORIENTED_EDGE('',*,*,#14001,.F.);
#18902=ORIENTED_EDGE('',*,*,#14003,.F.);
#18903=ORIENTED_EDGE('',*,*,#14004,.T.);
#18904=ORIENTED_EDGE('',*,*,#14005,.F.);
#18905=ORIENTED_EDGE('',*,*,#14006,.T.);
#18906=ORIENTED_EDGE('',*,*,#14007,.T.);
#18907=ORIENTED_EDGE('',*,*,#14008,.T.);
#18908=ORIENTED_EDGE('',*,*,#13987,.F.);
#18909=ORIENTED_EDGE('',*,*,#13984,.F.);
#18910=ORIENTED_EDGE('',*,*,#13990,.F.);
#18911=ORIENTED_EDGE('',*,*,#13993,.F.);
#18912=ORIENTED_EDGE('',*,*,#13996,.F.);
#18913=ORIENTED_EDGE('',*,*,#13999,.F.);
#18914=ORIENTED_EDGE('',*,*,#14002,.F.);
#18915=ORIENTED_EDGE('',*,*,#14009,.F.);
#18916=ORIENTED_EDGE('',*,*,#14010,.T.);
#18917=ORIENTED_EDGE('',*,*,#14003,.T.);
#18918=ORIENTED_EDGE('',*,*,#14011,.T.);
#18919=ORIENTED_EDGE('',*,*,#14012,.F.);
#18920=ORIENTED_EDGE('',*,*,#14013,.T.);
#18921=ORIENTED_EDGE('',*,*,#14009,.T.);
#18922=ORIENTED_EDGE('',*,*,#14014,.T.);
#18923=ORIENTED_EDGE('',*,*,#14015,.T.);
#18924=ORIENTED_EDGE('',*,*,#14016,.F.);
#18925=ORIENTED_EDGE('',*,*,#13982,.T.);
#18926=ORIENTED_EDGE('',*,*,#13985,.T.);
#18927=ORIENTED_EDGE('',*,*,#13988,.T.);
#18928=ORIENTED_EDGE('',*,*,#13991,.T.);
#18929=ORIENTED_EDGE('',*,*,#13994,.T.);
#18930=ORIENTED_EDGE('',*,*,#13997,.T.);
#18931=ORIENTED_EDGE('',*,*,#14000,.T.);
#18932=ORIENTED_EDGE('',*,*,#14017,.T.);
#18933=ORIENTED_EDGE('',*,*,#14006,.F.);
#18934=ORIENTED_EDGE('',*,*,#14018,.F.);
#18935=ORIENTED_EDGE('',*,*,#14016,.T.);
#18936=ORIENTED_EDGE('',*,*,#14005,.T.);
#18937=ORIENTED_EDGE('',*,*,#14019,.T.);
#18938=ORIENTED_EDGE('',*,*,#14012,.T.);
#18939=ORIENTED_EDGE('',*,*,#14018,.T.);
#18940=ORIENTED_EDGE('',*,*,#14015,.F.);
#18941=ORIENTED_EDGE('',*,*,#14020,.T.);
#18942=ORIENTED_EDGE('',*,*,#14007,.F.);
#18943=ORIENTED_EDGE('',*,*,#14017,.F.);
#18944=ORIENTED_EDGE('',*,*,#14004,.F.);
#18945=ORIENTED_EDGE('',*,*,#14010,.F.);
#18946=ORIENTED_EDGE('',*,*,#14013,.F.);
#18947=ORIENTED_EDGE('',*,*,#14019,.F.);
#18948=ORIENTED_EDGE('',*,*,#14008,.F.);
#18949=ORIENTED_EDGE('',*,*,#14020,.F.);
#18950=ORIENTED_EDGE('',*,*,#14014,.F.);
#18951=ORIENTED_EDGE('',*,*,#14011,.F.);
#18952=ORIENTED_EDGE('',*,*,#14021,.F.);
#18953=ORIENTED_EDGE('',*,*,#14022,.T.);
#18954=ORIENTED_EDGE('',*,*,#14023,.T.);
#18955=ORIENTED_EDGE('',*,*,#14022,.F.);
#18956=ORIENTED_EDGE('',*,*,#14024,.F.);
#18957=ORIENTED_EDGE('',*,*,#14025,.T.);
#18958=ORIENTED_EDGE('',*,*,#14026,.T.);
#18959=ORIENTED_EDGE('',*,*,#14025,.F.);
#18960=ORIENTED_EDGE('',*,*,#14027,.F.);
#18961=ORIENTED_EDGE('',*,*,#14028,.T.);
#18962=ORIENTED_EDGE('',*,*,#14029,.T.);
#18963=ORIENTED_EDGE('',*,*,#14028,.F.);
#18964=ORIENTED_EDGE('',*,*,#14030,.F.);
#18965=ORIENTED_EDGE('',*,*,#14031,.T.);
#18966=ORIENTED_EDGE('',*,*,#14032,.T.);
#18967=ORIENTED_EDGE('',*,*,#14031,.F.);
#18968=ORIENTED_EDGE('',*,*,#14033,.F.);
#18969=ORIENTED_EDGE('',*,*,#14034,.T.);
#18970=ORIENTED_EDGE('',*,*,#14035,.T.);
#18971=ORIENTED_EDGE('',*,*,#14034,.F.);
#18972=ORIENTED_EDGE('',*,*,#14036,.F.);
#18973=ORIENTED_EDGE('',*,*,#14037,.T.);
#18974=ORIENTED_EDGE('',*,*,#14038,.T.);
#18975=ORIENTED_EDGE('',*,*,#14037,.F.);
#18976=ORIENTED_EDGE('',*,*,#14039,.T.);
#18977=ORIENTED_EDGE('',*,*,#14040,.F.);
#18978=ORIENTED_EDGE('',*,*,#14041,.F.);
#18979=ORIENTED_EDGE('',*,*,#14042,.T.);
#18980=ORIENTED_EDGE('',*,*,#14043,.T.);
#18981=ORIENTED_EDGE('',*,*,#14044,.F.);
#18982=ORIENTED_EDGE('',*,*,#14045,.F.);
#18983=ORIENTED_EDGE('',*,*,#14040,.T.);
#18984=ORIENTED_EDGE('',*,*,#14046,.T.);
#18985=ORIENTED_EDGE('',*,*,#14047,.F.);
#18986=ORIENTED_EDGE('',*,*,#14048,.F.);
#18987=ORIENTED_EDGE('',*,*,#14044,.T.);
#18988=ORIENTED_EDGE('',*,*,#14049,.T.);
#18989=ORIENTED_EDGE('',*,*,#14042,.F.);
#18990=ORIENTED_EDGE('',*,*,#14050,.F.);
#18991=ORIENTED_EDGE('',*,*,#14047,.T.);
#18992=ORIENTED_EDGE('',*,*,#14041,.T.);
#18993=ORIENTED_EDGE('',*,*,#14045,.T.);
#18994=ORIENTED_EDGE('',*,*,#14048,.T.);
#18995=ORIENTED_EDGE('',*,*,#14050,.T.);
#18996=ORIENTED_EDGE('',*,*,#14023,.F.);
#18997=ORIENTED_EDGE('',*,*,#14026,.F.);
#18998=ORIENTED_EDGE('',*,*,#14029,.F.);
#18999=ORIENTED_EDGE('',*,*,#14032,.F.);
#19000=ORIENTED_EDGE('',*,*,#14035,.F.);
#19001=ORIENTED_EDGE('',*,*,#14038,.F.);
#19002=ORIENTED_EDGE('',*,*,#14039,.F.);
#19003=ORIENTED_EDGE('',*,*,#14049,.F.);
#19004=ORIENTED_EDGE('',*,*,#14046,.F.);
#19005=ORIENTED_EDGE('',*,*,#14043,.F.);
#19006=ORIENTED_EDGE('',*,*,#14021,.T.);
#19007=ORIENTED_EDGE('',*,*,#14024,.T.);
#19008=ORIENTED_EDGE('',*,*,#14027,.T.);
#19009=ORIENTED_EDGE('',*,*,#14030,.T.);
#19010=ORIENTED_EDGE('',*,*,#14033,.T.);
#19011=ORIENTED_EDGE('',*,*,#14036,.T.);
#19012=ORIENTED_EDGE('',*,*,#14051,.F.);
#19013=ORIENTED_EDGE('',*,*,#14052,.T.);
#19014=ORIENTED_EDGE('',*,*,#14053,.T.);
#19015=ORIENTED_EDGE('',*,*,#14052,.F.);
#19016=ORIENTED_EDGE('',*,*,#14054,.F.);
#19017=ORIENTED_EDGE('',*,*,#14055,.T.);
#19018=ORIENTED_EDGE('',*,*,#14056,.T.);
#19019=ORIENTED_EDGE('',*,*,#14055,.F.);
#19020=ORIENTED_EDGE('',*,*,#14057,.F.);
#19021=ORIENTED_EDGE('',*,*,#14058,.T.);
#19022=ORIENTED_EDGE('',*,*,#14059,.T.);
#19023=ORIENTED_EDGE('',*,*,#14058,.F.);
#19024=ORIENTED_EDGE('',*,*,#14060,.F.);
#19025=ORIENTED_EDGE('',*,*,#14061,.T.);
#19026=ORIENTED_EDGE('',*,*,#14062,.T.);
#19027=ORIENTED_EDGE('',*,*,#14061,.F.);
#19028=ORIENTED_EDGE('',*,*,#14063,.F.);
#19029=ORIENTED_EDGE('',*,*,#14064,.T.);
#19030=ORIENTED_EDGE('',*,*,#14065,.T.);
#19031=ORIENTED_EDGE('',*,*,#14064,.F.);
#19032=ORIENTED_EDGE('',*,*,#14066,.F.);
#19033=ORIENTED_EDGE('',*,*,#14067,.T.);
#19034=ORIENTED_EDGE('',*,*,#14068,.T.);
#19035=ORIENTED_EDGE('',*,*,#14067,.F.);
#19036=ORIENTED_EDGE('',*,*,#14069,.T.);
#19037=ORIENTED_EDGE('',*,*,#14070,.F.);
#19038=ORIENTED_EDGE('',*,*,#14071,.F.);
#19039=ORIENTED_EDGE('',*,*,#14072,.T.);
#19040=ORIENTED_EDGE('',*,*,#14073,.T.);
#19041=ORIENTED_EDGE('',*,*,#14074,.F.);
#19042=ORIENTED_EDGE('',*,*,#14075,.F.);
#19043=ORIENTED_EDGE('',*,*,#14070,.T.);
#19044=ORIENTED_EDGE('',*,*,#14076,.T.);
#19045=ORIENTED_EDGE('',*,*,#14077,.F.);
#19046=ORIENTED_EDGE('',*,*,#14078,.F.);
#19047=ORIENTED_EDGE('',*,*,#14074,.T.);
#19048=ORIENTED_EDGE('',*,*,#14079,.T.);
#19049=ORIENTED_EDGE('',*,*,#14072,.F.);
#19050=ORIENTED_EDGE('',*,*,#14080,.F.);
#19051=ORIENTED_EDGE('',*,*,#14077,.T.);
#19052=ORIENTED_EDGE('',*,*,#14071,.T.);
#19053=ORIENTED_EDGE('',*,*,#14075,.T.);
#19054=ORIENTED_EDGE('',*,*,#14078,.T.);
#19055=ORIENTED_EDGE('',*,*,#14080,.T.);
#19056=ORIENTED_EDGE('',*,*,#14053,.F.);
#19057=ORIENTED_EDGE('',*,*,#14056,.F.);
#19058=ORIENTED_EDGE('',*,*,#14059,.F.);
#19059=ORIENTED_EDGE('',*,*,#14062,.F.);
#19060=ORIENTED_EDGE('',*,*,#14065,.F.);
#19061=ORIENTED_EDGE('',*,*,#14068,.F.);
#19062=ORIENTED_EDGE('',*,*,#14069,.F.);
#19063=ORIENTED_EDGE('',*,*,#14079,.F.);
#19064=ORIENTED_EDGE('',*,*,#14076,.F.);
#19065=ORIENTED_EDGE('',*,*,#14073,.F.);
#19066=ORIENTED_EDGE('',*,*,#14051,.T.);
#19067=ORIENTED_EDGE('',*,*,#14054,.T.);
#19068=ORIENTED_EDGE('',*,*,#14057,.T.);
#19069=ORIENTED_EDGE('',*,*,#14060,.T.);
#19070=ORIENTED_EDGE('',*,*,#14063,.T.);
#19071=ORIENTED_EDGE('',*,*,#14066,.T.);
#19072=ORIENTED_EDGE('',*,*,#14081,.F.);
#19073=ORIENTED_EDGE('',*,*,#14082,.F.);
#19074=ORIENTED_EDGE('',*,*,#14083,.T.);
#19075=ORIENTED_EDGE('',*,*,#14084,.T.);
#19076=ORIENTED_EDGE('',*,*,#14085,.F.);
#19077=ORIENTED_EDGE('',*,*,#14086,.F.);
#19078=ORIENTED_EDGE('',*,*,#14087,.T.);
#19079=ORIENTED_EDGE('',*,*,#14082,.T.);
#19080=ORIENTED_EDGE('',*,*,#14088,.F.);
#19081=ORIENTED_EDGE('',*,*,#14089,.F.);
#19082=ORIENTED_EDGE('',*,*,#14090,.T.);
#19083=ORIENTED_EDGE('',*,*,#14086,.T.);
#19084=ORIENTED_EDGE('',*,*,#14091,.T.);
#19085=ORIENTED_EDGE('',*,*,#14092,.F.);
#19086=ORIENTED_EDGE('',*,*,#14093,.F.);
#19087=ORIENTED_EDGE('',*,*,#14089,.T.);
#19088=ORIENTED_EDGE('',*,*,#14094,.T.);
#19089=ORIENTED_EDGE('',*,*,#14084,.F.);
#19090=ORIENTED_EDGE('',*,*,#14095,.F.);
#19091=ORIENTED_EDGE('',*,*,#14092,.T.);
#19092=ORIENTED_EDGE('',*,*,#14083,.F.);
#19093=ORIENTED_EDGE('',*,*,#14087,.F.);
#19094=ORIENTED_EDGE('',*,*,#14090,.F.);
#19095=ORIENTED_EDGE('',*,*,#14093,.T.);
#19096=ORIENTED_EDGE('',*,*,#14095,.T.);
#19097=ORIENTED_EDGE('',*,*,#14081,.T.);
#19098=ORIENTED_EDGE('',*,*,#14094,.F.);
#19099=ORIENTED_EDGE('',*,*,#14091,.F.);
#19100=ORIENTED_EDGE('',*,*,#14088,.T.);
#19101=ORIENTED_EDGE('',*,*,#14085,.T.);
#19102=ORIENTED_EDGE('',*,*,#14096,.T.);
#19103=ORIENTED_EDGE('',*,*,#14097,.F.);
#19104=ORIENTED_EDGE('',*,*,#14098,.F.);
#19105=ORIENTED_EDGE('',*,*,#14099,.T.);
#19106=ORIENTED_EDGE('',*,*,#14100,.T.);
#19107=ORIENTED_EDGE('',*,*,#14099,.F.);
#19108=ORIENTED_EDGE('',*,*,#14101,.F.);
#19109=ORIENTED_EDGE('',*,*,#14102,.T.);
#19110=ORIENTED_EDGE('',*,*,#14103,.T.);
#19111=ORIENTED_EDGE('',*,*,#14102,.F.);
#19112=ORIENTED_EDGE('',*,*,#14104,.F.);
#19113=ORIENTED_EDGE('',*,*,#14105,.T.);
#19114=ORIENTED_EDGE('',*,*,#14106,.F.);
#19115=ORIENTED_EDGE('',*,*,#14105,.F.);
#19116=ORIENTED_EDGE('',*,*,#14107,.T.);
#19117=ORIENTED_EDGE('',*,*,#14108,.T.);
#19118=ORIENTED_EDGE('',*,*,#14109,.F.);
#19119=ORIENTED_EDGE('',*,*,#14108,.F.);
#19120=ORIENTED_EDGE('',*,*,#14110,.T.);
#19121=ORIENTED_EDGE('',*,*,#14097,.T.);
#19122=ORIENTED_EDGE('',*,*,#14098,.T.);
#19123=ORIENTED_EDGE('',*,*,#14110,.F.);
#19124=ORIENTED_EDGE('',*,*,#14107,.F.);
#19125=ORIENTED_EDGE('',*,*,#14104,.T.);
#19126=ORIENTED_EDGE('',*,*,#14101,.T.);
#19127=ORIENTED_EDGE('',*,*,#14096,.F.);
#19128=ORIENTED_EDGE('',*,*,#14100,.F.);
#19129=ORIENTED_EDGE('',*,*,#14103,.F.);
#19130=ORIENTED_EDGE('',*,*,#14106,.T.);
#19131=ORIENTED_EDGE('',*,*,#14109,.T.);
#19132=ORIENTED_EDGE('',*,*,#14111,.T.);
#19133=ORIENTED_EDGE('',*,*,#14112,.T.);
#19134=ORIENTED_EDGE('',*,*,#14113,.T.);
#19135=ORIENTED_EDGE('',*,*,#14114,.F.);
#19136=ORIENTED_EDGE('',*,*,#14115,.T.);
#19137=ORIENTED_EDGE('',*,*,#14116,.T.);
#19138=ORIENTED_EDGE('',*,*,#14117,.T.);
#19139=ORIENTED_EDGE('',*,*,#14116,.F.);
#19140=ORIENTED_EDGE('',*,*,#14118,.T.);
#19141=ORIENTED_EDGE('',*,*,#14119,.T.);
#19142=ORIENTED_EDGE('',*,*,#14120,.T.);
#19143=ORIENTED_EDGE('',*,*,#14119,.F.);
#19144=ORIENTED_EDGE('',*,*,#14121,.T.);
#19145=ORIENTED_EDGE('',*,*,#14122,.T.);
#19146=ORIENTED_EDGE('',*,*,#14123,.T.);
#19147=ORIENTED_EDGE('',*,*,#14122,.F.);
#19148=ORIENTED_EDGE('',*,*,#14124,.T.);
#19149=ORIENTED_EDGE('',*,*,#14125,.T.);
#19150=ORIENTED_EDGE('',*,*,#14126,.T.);
#19151=ORIENTED_EDGE('',*,*,#14125,.F.);
#19152=ORIENTED_EDGE('',*,*,#14127,.T.);
#19153=ORIENTED_EDGE('',*,*,#14128,.T.);
#19154=ORIENTED_EDGE('',*,*,#14129,.T.);
#19155=ORIENTED_EDGE('',*,*,#14128,.F.);
#19156=ORIENTED_EDGE('',*,*,#14130,.T.);
#19157=ORIENTED_EDGE('',*,*,#14131,.T.);
#19158=ORIENTED_EDGE('',*,*,#14132,.T.);
#19159=ORIENTED_EDGE('',*,*,#14131,.F.);
#19160=ORIENTED_EDGE('',*,*,#14133,.T.);
#19161=ORIENTED_EDGE('',*,*,#14134,.T.);
#19162=ORIENTED_EDGE('',*,*,#14135,.T.);
#19163=ORIENTED_EDGE('',*,*,#14134,.F.);
#19164=ORIENTED_EDGE('',*,*,#14136,.T.);
#19165=ORIENTED_EDGE('',*,*,#14137,.T.);
#19166=ORIENTED_EDGE('',*,*,#14138,.T.);
#19167=ORIENTED_EDGE('',*,*,#14137,.F.);
#19168=ORIENTED_EDGE('',*,*,#14139,.T.);
#19169=ORIENTED_EDGE('',*,*,#14140,.T.);
#19170=ORIENTED_EDGE('',*,*,#14141,.T.);
#19171=ORIENTED_EDGE('',*,*,#14140,.F.);
#19172=ORIENTED_EDGE('',*,*,#14142,.F.);
#19173=ORIENTED_EDGE('',*,*,#14143,.T.);
#19174=ORIENTED_EDGE('',*,*,#14144,.T.);
#19175=ORIENTED_EDGE('',*,*,#14143,.F.);
#19176=ORIENTED_EDGE('',*,*,#14145,.T.);
#19177=ORIENTED_EDGE('',*,*,#14146,.T.);
#19178=ORIENTED_EDGE('',*,*,#14147,.T.);
#19179=ORIENTED_EDGE('',*,*,#14146,.F.);
#19180=ORIENTED_EDGE('',*,*,#14148,.T.);
#19181=ORIENTED_EDGE('',*,*,#14149,.T.);
#19182=ORIENTED_EDGE('',*,*,#14150,.T.);
#19183=ORIENTED_EDGE('',*,*,#14149,.F.);
#19184=ORIENTED_EDGE('',*,*,#14151,.T.);
#19185=ORIENTED_EDGE('',*,*,#14152,.T.);
#19186=ORIENTED_EDGE('',*,*,#14153,.T.);
#19187=ORIENTED_EDGE('',*,*,#14152,.F.);
#19188=ORIENTED_EDGE('',*,*,#14154,.T.);
#19189=ORIENTED_EDGE('',*,*,#14155,.T.);
#19190=ORIENTED_EDGE('',*,*,#14156,.T.);
#19191=ORIENTED_EDGE('',*,*,#14155,.F.);
#19192=ORIENTED_EDGE('',*,*,#14157,.T.);
#19193=ORIENTED_EDGE('',*,*,#14158,.T.);
#19194=ORIENTED_EDGE('',*,*,#14159,.T.);
#19195=ORIENTED_EDGE('',*,*,#14158,.F.);
#19196=ORIENTED_EDGE('',*,*,#14160,.T.);
#19197=ORIENTED_EDGE('',*,*,#14161,.T.);
#19198=ORIENTED_EDGE('',*,*,#14162,.T.);
#19199=ORIENTED_EDGE('',*,*,#14161,.F.);
#19200=ORIENTED_EDGE('',*,*,#14163,.F.);
#19201=ORIENTED_EDGE('',*,*,#14164,.T.);
#19202=ORIENTED_EDGE('',*,*,#14165,.T.);
#19203=ORIENTED_EDGE('',*,*,#14164,.F.);
#19204=ORIENTED_EDGE('',*,*,#14166,.F.);
#19205=ORIENTED_EDGE('',*,*,#14167,.T.);
#19206=ORIENTED_EDGE('',*,*,#14168,.T.);
#19207=ORIENTED_EDGE('',*,*,#14167,.F.);
#19208=ORIENTED_EDGE('',*,*,#14169,.F.);
#19209=ORIENTED_EDGE('',*,*,#14170,.T.);
#19210=ORIENTED_EDGE('',*,*,#14171,.T.);
#19211=ORIENTED_EDGE('',*,*,#14170,.F.);
#19212=ORIENTED_EDGE('',*,*,#14172,.F.);
#19213=ORIENTED_EDGE('',*,*,#14173,.T.);
#19214=ORIENTED_EDGE('',*,*,#14174,.T.);
#19215=ORIENTED_EDGE('',*,*,#14173,.F.);
#19216=ORIENTED_EDGE('',*,*,#14175,.F.);
#19217=ORIENTED_EDGE('',*,*,#14176,.T.);
#19218=ORIENTED_EDGE('',*,*,#14177,.T.);
#19219=ORIENTED_EDGE('',*,*,#14176,.F.);
#19220=ORIENTED_EDGE('',*,*,#14178,.F.);
#19221=ORIENTED_EDGE('',*,*,#14179,.T.);
#19222=ORIENTED_EDGE('',*,*,#14180,.T.);
#19223=ORIENTED_EDGE('',*,*,#14179,.F.);
#19224=ORIENTED_EDGE('',*,*,#14181,.F.);
#19225=ORIENTED_EDGE('',*,*,#14182,.T.);
#19226=ORIENTED_EDGE('',*,*,#14183,.T.);
#19227=ORIENTED_EDGE('',*,*,#14182,.F.);
#19228=ORIENTED_EDGE('',*,*,#14184,.F.);
#19229=ORIENTED_EDGE('',*,*,#14185,.T.);
#19230=ORIENTED_EDGE('',*,*,#14186,.T.);
#19231=ORIENTED_EDGE('',*,*,#14185,.F.);
#19232=ORIENTED_EDGE('',*,*,#14187,.F.);
#19233=ORIENTED_EDGE('',*,*,#14188,.T.);
#19234=ORIENTED_EDGE('',*,*,#14189,.T.);
#19235=ORIENTED_EDGE('',*,*,#14188,.F.);
#19236=ORIENTED_EDGE('',*,*,#14190,.F.);
#19237=ORIENTED_EDGE('',*,*,#14191,.T.);
#19238=ORIENTED_EDGE('',*,*,#14192,.T.);
#19239=ORIENTED_EDGE('',*,*,#14191,.F.);
#19240=ORIENTED_EDGE('',*,*,#14193,.F.);
#19241=ORIENTED_EDGE('',*,*,#14194,.T.);
#19242=ORIENTED_EDGE('',*,*,#14195,.T.);
#19243=ORIENTED_EDGE('',*,*,#14194,.F.);
#19244=ORIENTED_EDGE('',*,*,#14196,.F.);
#19245=ORIENTED_EDGE('',*,*,#14197,.T.);
#19246=ORIENTED_EDGE('',*,*,#14198,.T.);
#19247=ORIENTED_EDGE('',*,*,#14197,.F.);
#19248=ORIENTED_EDGE('',*,*,#14199,.F.);
#19249=ORIENTED_EDGE('',*,*,#14200,.T.);
#19250=ORIENTED_EDGE('',*,*,#14201,.T.);
#19251=ORIENTED_EDGE('',*,*,#14200,.F.);
#19252=ORIENTED_EDGE('',*,*,#14202,.F.);
#19253=ORIENTED_EDGE('',*,*,#14203,.T.);
#19254=ORIENTED_EDGE('',*,*,#14204,.T.);
#19255=ORIENTED_EDGE('',*,*,#14203,.F.);
#19256=ORIENTED_EDGE('',*,*,#14205,.F.);
#19257=ORIENTED_EDGE('',*,*,#14206,.T.);
#19258=ORIENTED_EDGE('',*,*,#14207,.T.);
#19259=ORIENTED_EDGE('',*,*,#14206,.F.);
#19260=ORIENTED_EDGE('',*,*,#14208,.F.);
#19261=ORIENTED_EDGE('',*,*,#14209,.T.);
#19262=ORIENTED_EDGE('',*,*,#14210,.T.);
#19263=ORIENTED_EDGE('',*,*,#14209,.F.);
#19264=ORIENTED_EDGE('',*,*,#14211,.F.);
#19265=ORIENTED_EDGE('',*,*,#14212,.T.);
#19266=ORIENTED_EDGE('',*,*,#14213,.T.);
#19267=ORIENTED_EDGE('',*,*,#14212,.F.);
#19268=ORIENTED_EDGE('',*,*,#14214,.F.);
#19269=ORIENTED_EDGE('',*,*,#14215,.T.);
#19270=ORIENTED_EDGE('',*,*,#14216,.T.);
#19271=ORIENTED_EDGE('',*,*,#14215,.F.);
#19272=ORIENTED_EDGE('',*,*,#14217,.F.);
#19273=ORIENTED_EDGE('',*,*,#14218,.T.);
#19274=ORIENTED_EDGE('',*,*,#14219,.T.);
#19275=ORIENTED_EDGE('',*,*,#14218,.F.);
#19276=ORIENTED_EDGE('',*,*,#14220,.F.);
#19277=ORIENTED_EDGE('',*,*,#14221,.T.);
#19278=ORIENTED_EDGE('',*,*,#14222,.T.);
#19279=ORIENTED_EDGE('',*,*,#14221,.F.);
#19280=ORIENTED_EDGE('',*,*,#14223,.F.);
#19281=ORIENTED_EDGE('',*,*,#14224,.T.);
#19282=ORIENTED_EDGE('',*,*,#14225,.T.);
#19283=ORIENTED_EDGE('',*,*,#14224,.F.);
#19284=ORIENTED_EDGE('',*,*,#14226,.F.);
#19285=ORIENTED_EDGE('',*,*,#14227,.T.);
#19286=ORIENTED_EDGE('',*,*,#14228,.T.);
#19287=ORIENTED_EDGE('',*,*,#14227,.F.);
#19288=ORIENTED_EDGE('',*,*,#14229,.F.);
#19289=ORIENTED_EDGE('',*,*,#14230,.T.);
#19290=ORIENTED_EDGE('',*,*,#14231,.T.);
#19291=ORIENTED_EDGE('',*,*,#14230,.F.);
#19292=ORIENTED_EDGE('',*,*,#14232,.F.);
#19293=ORIENTED_EDGE('',*,*,#14233,.T.);
#19294=ORIENTED_EDGE('',*,*,#14234,.T.);
#19295=ORIENTED_EDGE('',*,*,#14233,.F.);
#19296=ORIENTED_EDGE('',*,*,#14235,.F.);
#19297=ORIENTED_EDGE('',*,*,#14236,.T.);
#19298=ORIENTED_EDGE('',*,*,#14237,.T.);
#19299=ORIENTED_EDGE('',*,*,#14236,.F.);
#19300=ORIENTED_EDGE('',*,*,#14238,.F.);
#19301=ORIENTED_EDGE('',*,*,#14239,.T.);
#19302=ORIENTED_EDGE('',*,*,#14240,.T.);
#19303=ORIENTED_EDGE('',*,*,#14239,.F.);
#19304=ORIENTED_EDGE('',*,*,#14241,.F.);
#19305=ORIENTED_EDGE('',*,*,#14242,.T.);
#19306=ORIENTED_EDGE('',*,*,#14243,.T.);
#19307=ORIENTED_EDGE('',*,*,#14242,.F.);
#19308=ORIENTED_EDGE('',*,*,#14244,.F.);
#19309=ORIENTED_EDGE('',*,*,#14245,.T.);
#19310=ORIENTED_EDGE('',*,*,#14246,.T.);
#19311=ORIENTED_EDGE('',*,*,#14245,.F.);
#19312=ORIENTED_EDGE('',*,*,#14247,.F.);
#19313=ORIENTED_EDGE('',*,*,#14248,.T.);
#19314=ORIENTED_EDGE('',*,*,#14249,.T.);
#19315=ORIENTED_EDGE('',*,*,#14248,.F.);
#19316=ORIENTED_EDGE('',*,*,#14250,.F.);
#19317=ORIENTED_EDGE('',*,*,#14251,.T.);
#19318=ORIENTED_EDGE('',*,*,#14252,.T.);
#19319=ORIENTED_EDGE('',*,*,#14251,.F.);
#19320=ORIENTED_EDGE('',*,*,#14253,.F.);
#19321=ORIENTED_EDGE('',*,*,#14254,.T.);
#19322=ORIENTED_EDGE('',*,*,#14255,.T.);
#19323=ORIENTED_EDGE('',*,*,#14254,.F.);
#19324=ORIENTED_EDGE('',*,*,#14256,.F.);
#19325=ORIENTED_EDGE('',*,*,#14257,.T.);
#19326=ORIENTED_EDGE('',*,*,#14258,.T.);
#19327=ORIENTED_EDGE('',*,*,#14257,.F.);
#19328=ORIENTED_EDGE('',*,*,#14259,.F.);
#19329=ORIENTED_EDGE('',*,*,#14260,.T.);
#19330=ORIENTED_EDGE('',*,*,#14261,.F.);
#19331=ORIENTED_EDGE('',*,*,#14262,.T.);
#19332=ORIENTED_EDGE('',*,*,#14263,.F.);
#19333=ORIENTED_EDGE('',*,*,#14264,.T.);
#19334=ORIENTED_EDGE('',*,*,#14265,.F.);
#19335=ORIENTED_EDGE('',*,*,#14266,.T.);
#19336=ORIENTED_EDGE('',*,*,#14256,.T.);
#19337=ORIENTED_EDGE('',*,*,#14250,.T.);
#19338=ORIENTED_EDGE('',*,*,#14244,.T.);
#19339=ORIENTED_EDGE('',*,*,#14238,.T.);
#19340=ORIENTED_EDGE('',*,*,#14232,.T.);
#19341=ORIENTED_EDGE('',*,*,#14226,.T.);
#19342=ORIENTED_EDGE('',*,*,#14220,.T.);
#19343=ORIENTED_EDGE('',*,*,#14166,.T.);
#19344=ORIENTED_EDGE('',*,*,#14147,.F.);
#19345=ORIENTED_EDGE('',*,*,#14150,.F.);
#19346=ORIENTED_EDGE('',*,*,#14153,.F.);
#19347=ORIENTED_EDGE('',*,*,#14156,.F.);
#19348=ORIENTED_EDGE('',*,*,#14159,.F.);
#19349=ORIENTED_EDGE('',*,*,#14162,.F.);
#19350=ORIENTED_EDGE('',*,*,#14172,.T.);
#19351=ORIENTED_EDGE('',*,*,#14178,.T.);
#19352=ORIENTED_EDGE('',*,*,#14184,.T.);
#19353=ORIENTED_EDGE('',*,*,#14190,.T.);
#19354=ORIENTED_EDGE('',*,*,#14196,.T.);
#19355=ORIENTED_EDGE('',*,*,#14202,.T.);
#19356=ORIENTED_EDGE('',*,*,#14208,.T.);
#19357=ORIENTED_EDGE('',*,*,#14214,.T.);
#19358=ORIENTED_EDGE('',*,*,#14267,.T.);
#19359=ORIENTED_EDGE('',*,*,#14268,.T.);
#19360=ORIENTED_EDGE('',*,*,#14269,.F.);
#19361=ORIENTED_EDGE('',*,*,#14270,.T.);
#19362=ORIENTED_EDGE('',*,*,#14271,.F.);
#19363=ORIENTED_EDGE('',*,*,#14272,.T.);
#19364=ORIENTED_EDGE('',*,*,#14273,.T.);
#19365=ORIENTED_EDGE('',*,*,#14274,.T.);
#19366=ORIENTED_EDGE('',*,*,#14275,.T.);
#19367=ORIENTED_EDGE('',*,*,#14276,.T.);
#19368=ORIENTED_EDGE('',*,*,#14277,.F.);
#19369=ORIENTED_EDGE('',*,*,#14278,.F.);
#19370=ORIENTED_EDGE('',*,*,#14269,.T.);
#19371=ORIENTED_EDGE('',*,*,#14279,.T.);
#19372=ORIENTED_EDGE('',*,*,#14271,.T.);
#19373=ORIENTED_EDGE('',*,*,#14280,.T.);
#19374=ORIENTED_EDGE('',*,*,#14275,.F.);
#19375=ORIENTED_EDGE('',*,*,#14281,.T.);
#19376=ORIENTED_EDGE('',*,*,#14117,.F.);
#19377=ORIENTED_EDGE('',*,*,#14120,.F.);
#19378=ORIENTED_EDGE('',*,*,#14123,.F.);
#19379=ORIENTED_EDGE('',*,*,#14126,.F.);
#19380=ORIENTED_EDGE('',*,*,#14282,.F.);
#19381=ORIENTED_EDGE('',*,*,#14111,.F.);
#19382=ORIENTED_EDGE('',*,*,#14283,.F.);
#19383=ORIENTED_EDGE('',*,*,#14284,.F.);
#19384=ORIENTED_EDGE('',*,*,#14129,.F.);
#19385=ORIENTED_EDGE('',*,*,#14132,.F.);
#19386=ORIENTED_EDGE('',*,*,#14135,.F.);
#19387=ORIENTED_EDGE('',*,*,#14138,.F.);
#19388=ORIENTED_EDGE('',*,*,#14144,.F.);
#19389=ORIENTED_EDGE('',*,*,#14273,.F.);
#19390=ORIENTED_EDGE('',*,*,#14285,.T.);
#19391=ORIENTED_EDGE('',*,*,#14267,.F.);
#19392=ORIENTED_EDGE('',*,*,#14286,.F.);
#19393=ORIENTED_EDGE('',*,*,#14277,.T.);
#19394=ORIENTED_EDGE('',*,*,#14287,.T.);
#19395=ORIENTED_EDGE('',*,*,#14113,.F.);
#19396=ORIENTED_EDGE('',*,*,#14288,.F.);
#19397=ORIENTED_EDGE('',*,*,#14289,.F.);
#19398=ORIENTED_EDGE('',*,*,#14290,.F.);
#19399=ORIENTED_EDGE('',*,*,#14115,.F.);
#19400=ORIENTED_EDGE('',*,*,#14118,.F.);
#19401=ORIENTED_EDGE('',*,*,#14121,.F.);
#19402=ORIENTED_EDGE('',*,*,#14124,.F.);
#19403=ORIENTED_EDGE('',*,*,#14127,.F.);
#19404=ORIENTED_EDGE('',*,*,#14130,.F.);
#19405=ORIENTED_EDGE('',*,*,#14133,.F.);
#19406=ORIENTED_EDGE('',*,*,#14136,.F.);
#19407=ORIENTED_EDGE('',*,*,#14139,.F.);
#19408=ORIENTED_EDGE('',*,*,#14291,.T.);
#19409=ORIENTED_EDGE('',*,*,#14292,.T.);
#19410=ORIENTED_EDGE('',*,*,#14293,.T.);
#19411=ORIENTED_EDGE('',*,*,#14294,.T.);
#19412=ORIENTED_EDGE('',*,*,#14295,.T.);
#19413=ORIENTED_EDGE('',*,*,#14296,.T.);
#19414=ORIENTED_EDGE('',*,*,#14297,.T.);
#19415=ORIENTED_EDGE('',*,*,#14298,.T.);
#19416=ORIENTED_EDGE('',*,*,#14281,.F.);
#19417=ORIENTED_EDGE('',*,*,#14278,.T.);
#19418=ORIENTED_EDGE('',*,*,#14286,.T.);
#19419=ORIENTED_EDGE('',*,*,#14270,.F.);
#19420=ORIENTED_EDGE('',*,*,#14145,.F.);
#19421=ORIENTED_EDGE('',*,*,#14148,.F.);
#19422=ORIENTED_EDGE('',*,*,#14151,.F.);
#19423=ORIENTED_EDGE('',*,*,#14154,.F.);
#19424=ORIENTED_EDGE('',*,*,#14157,.F.);
#19425=ORIENTED_EDGE('',*,*,#14160,.F.);
#19426=ORIENTED_EDGE('',*,*,#14165,.F.);
#19427=ORIENTED_EDGE('',*,*,#14171,.F.);
#19428=ORIENTED_EDGE('',*,*,#14177,.F.);
#19429=ORIENTED_EDGE('',*,*,#14183,.F.);
#19430=ORIENTED_EDGE('',*,*,#14189,.F.);
#19431=ORIENTED_EDGE('',*,*,#14195,.F.);
#19432=ORIENTED_EDGE('',*,*,#14201,.F.);
#19433=ORIENTED_EDGE('',*,*,#14207,.F.);
#19434=ORIENTED_EDGE('',*,*,#14213,.F.);
#19435=ORIENTED_EDGE('',*,*,#14219,.F.);
#19436=ORIENTED_EDGE('',*,*,#14225,.F.);
#19437=ORIENTED_EDGE('',*,*,#14231,.F.);
#19438=ORIENTED_EDGE('',*,*,#14237,.F.);
#19439=ORIENTED_EDGE('',*,*,#14243,.F.);
#19440=ORIENTED_EDGE('',*,*,#14249,.F.);
#19441=ORIENTED_EDGE('',*,*,#14255,.F.);
#19442=ORIENTED_EDGE('',*,*,#14293,.F.);
#19443=ORIENTED_EDGE('',*,*,#14299,.T.);
#19444=ORIENTED_EDGE('',*,*,#14259,.T.);
#19445=ORIENTED_EDGE('',*,*,#14300,.T.);
#19446=ORIENTED_EDGE('',*,*,#14265,.T.);
#19447=ORIENTED_EDGE('',*,*,#14301,.T.);
#19448=ORIENTED_EDGE('',*,*,#14295,.F.);
#19449=ORIENTED_EDGE('',*,*,#14302,.T.);
#19450=ORIENTED_EDGE('',*,*,#14263,.T.);
#19451=ORIENTED_EDGE('',*,*,#14303,.T.);
#19452=ORIENTED_EDGE('',*,*,#14297,.F.);
#19453=ORIENTED_EDGE('',*,*,#14304,.T.);
#19454=ORIENTED_EDGE('',*,*,#14261,.T.);
#19455=ORIENTED_EDGE('',*,*,#14305,.T.);
#19456=ORIENTED_EDGE('',*,*,#14291,.F.);
#19457=ORIENTED_EDGE('',*,*,#14306,.T.);
#19458=ORIENTED_EDGE('',*,*,#14253,.T.);
#19459=ORIENTED_EDGE('',*,*,#14258,.F.);
#19460=ORIENTED_EDGE('',*,*,#14247,.T.);
#19461=ORIENTED_EDGE('',*,*,#14252,.F.);
#19462=ORIENTED_EDGE('',*,*,#14241,.T.);
#19463=ORIENTED_EDGE('',*,*,#14246,.F.);
#19464=ORIENTED_EDGE('',*,*,#14235,.T.);
#19465=ORIENTED_EDGE('',*,*,#14240,.F.);
#19466=ORIENTED_EDGE('',*,*,#14229,.T.);
#19467=ORIENTED_EDGE('',*,*,#14234,.F.);
#19468=ORIENTED_EDGE('',*,*,#14223,.T.);
#19469=ORIENTED_EDGE('',*,*,#14228,.F.);
#19470=ORIENTED_EDGE('',*,*,#14217,.T.);
#19471=ORIENTED_EDGE('',*,*,#14222,.F.);
#19472=ORIENTED_EDGE('',*,*,#14211,.T.);
#19473=ORIENTED_EDGE('',*,*,#14216,.F.);
#19474=ORIENTED_EDGE('',*,*,#14205,.T.);
#19475=ORIENTED_EDGE('',*,*,#14210,.F.);
#19476=ORIENTED_EDGE('',*,*,#14199,.T.);
#19477=ORIENTED_EDGE('',*,*,#14204,.F.);
#19478=ORIENTED_EDGE('',*,*,#14193,.T.);
#19479=ORIENTED_EDGE('',*,*,#14198,.F.);
#19480=ORIENTED_EDGE('',*,*,#14187,.T.);
#19481=ORIENTED_EDGE('',*,*,#14192,.F.);
#19482=ORIENTED_EDGE('',*,*,#14181,.T.);
#19483=ORIENTED_EDGE('',*,*,#14186,.F.);
#19484=ORIENTED_EDGE('',*,*,#14175,.T.);
#19485=ORIENTED_EDGE('',*,*,#14180,.F.);
#19486=ORIENTED_EDGE('',*,*,#14169,.T.);
#19487=ORIENTED_EDGE('',*,*,#14174,.F.);
#19488=ORIENTED_EDGE('',*,*,#14163,.T.);
#19489=ORIENTED_EDGE('',*,*,#14168,.F.);
#19490=ORIENTED_EDGE('',*,*,#14142,.T.);
#19491=ORIENTED_EDGE('',*,*,#14141,.F.);
#19492=ORIENTED_EDGE('',*,*,#14279,.F.);
#19493=ORIENTED_EDGE('',*,*,#14268,.F.);
#19494=ORIENTED_EDGE('',*,*,#14285,.F.);
#19495=ORIENTED_EDGE('',*,*,#14272,.F.);
#19496=ORIENTED_EDGE('',*,*,#14280,.F.);
#19497=ORIENTED_EDGE('',*,*,#14274,.F.);
#19498=ORIENTED_EDGE('',*,*,#14287,.F.);
#19499=ORIENTED_EDGE('',*,*,#14276,.F.);
#19500=ORIENTED_EDGE('',*,*,#14282,.T.);
#19501=ORIENTED_EDGE('',*,*,#14307,.T.);
#19502=ORIENTED_EDGE('',*,*,#14288,.T.);
#19503=ORIENTED_EDGE('',*,*,#14112,.F.);
#19504=ORIENTED_EDGE('',*,*,#14283,.T.);
#19505=ORIENTED_EDGE('',*,*,#14114,.T.);
#19506=ORIENTED_EDGE('',*,*,#14290,.T.);
#19507=ORIENTED_EDGE('',*,*,#14308,.F.);
#19508=ORIENTED_EDGE('',*,*,#14284,.T.);
#19509=ORIENTED_EDGE('',*,*,#14308,.T.);
#19510=ORIENTED_EDGE('',*,*,#14289,.T.);
#19511=ORIENTED_EDGE('',*,*,#14307,.F.);
#19512=ORIENTED_EDGE('',*,*,#14292,.F.);
#19513=ORIENTED_EDGE('',*,*,#14305,.F.);
#19514=ORIENTED_EDGE('',*,*,#14260,.F.);
#19515=ORIENTED_EDGE('',*,*,#14299,.F.);
#19516=ORIENTED_EDGE('',*,*,#14298,.F.);
#19517=ORIENTED_EDGE('',*,*,#14303,.F.);
#19518=ORIENTED_EDGE('',*,*,#14262,.F.);
#19519=ORIENTED_EDGE('',*,*,#14306,.F.);
#19520=ORIENTED_EDGE('',*,*,#14296,.F.);
#19521=ORIENTED_EDGE('',*,*,#14301,.F.);
#19522=ORIENTED_EDGE('',*,*,#14264,.F.);
#19523=ORIENTED_EDGE('',*,*,#14304,.F.);
#19524=ORIENTED_EDGE('',*,*,#14294,.F.);
#19525=ORIENTED_EDGE('',*,*,#14300,.F.);
#19526=ORIENTED_EDGE('',*,*,#14266,.F.);
#19527=ORIENTED_EDGE('',*,*,#14302,.F.);
#19528=ORIENTED_EDGE('',*,*,#14309,.F.);
#19529=ORIENTED_EDGE('',*,*,#14310,.T.);
#19530=ORIENTED_EDGE('',*,*,#14311,.T.);
#19531=ORIENTED_EDGE('',*,*,#14310,.F.);
#19532=ORIENTED_EDGE('',*,*,#14312,.F.);
#19533=ORIENTED_EDGE('',*,*,#14313,.F.);
#19534=ORIENTED_EDGE('',*,*,#14314,.F.);
#19535=ORIENTED_EDGE('',*,*,#14315,.F.);
#19536=ORIENTED_EDGE('',*,*,#14316,.F.);
#19537=ORIENTED_EDGE('',*,*,#14317,.T.);
#19538=ORIENTED_EDGE('',*,*,#14318,.T.);
#19539=ORIENTED_EDGE('',*,*,#14317,.F.);
#19540=ORIENTED_EDGE('',*,*,#14319,.F.);
#19541=ORIENTED_EDGE('',*,*,#14320,.F.);
#19542=ORIENTED_EDGE('',*,*,#14321,.F.);
#19543=ORIENTED_EDGE('',*,*,#14322,.F.);
#19544=ORIENTED_EDGE('',*,*,#14323,.F.);
#19545=ORIENTED_EDGE('',*,*,#14324,.T.);
#19546=ORIENTED_EDGE('',*,*,#14325,.T.);
#19547=ORIENTED_EDGE('',*,*,#14324,.F.);
#19548=ORIENTED_EDGE('',*,*,#14326,.F.);
#19549=ORIENTED_EDGE('',*,*,#14327,.F.);
#19550=ORIENTED_EDGE('',*,*,#14328,.F.);
#19551=ORIENTED_EDGE('',*,*,#14329,.F.);
#19552=ORIENTED_EDGE('',*,*,#14330,.F.);
#19553=ORIENTED_EDGE('',*,*,#14331,.T.);
#19554=ORIENTED_EDGE('',*,*,#14332,.T.);
#19555=ORIENTED_EDGE('',*,*,#14331,.F.);
#19556=ORIENTED_EDGE('',*,*,#14333,.F.);
#19557=ORIENTED_EDGE('',*,*,#14334,.F.);
#19558=ORIENTED_EDGE('',*,*,#14335,.F.);
#19559=ORIENTED_EDGE('',*,*,#14336,.F.);
#19560=ORIENTED_EDGE('',*,*,#14337,.F.);
#19561=ORIENTED_EDGE('',*,*,#14338,.T.);
#19562=ORIENTED_EDGE('',*,*,#14339,.T.);
#19563=ORIENTED_EDGE('',*,*,#14338,.F.);
#19564=ORIENTED_EDGE('',*,*,#14340,.F.);
#19565=ORIENTED_EDGE('',*,*,#14341,.F.);
#19566=ORIENTED_EDGE('',*,*,#14342,.F.);
#19567=ORIENTED_EDGE('',*,*,#14343,.F.);
#19568=ORIENTED_EDGE('',*,*,#14344,.F.);
#19569=ORIENTED_EDGE('',*,*,#14345,.T.);
#19570=ORIENTED_EDGE('',*,*,#14346,.T.);
#19571=ORIENTED_EDGE('',*,*,#14345,.F.);
#19572=ORIENTED_EDGE('',*,*,#14347,.F.);
#19573=ORIENTED_EDGE('',*,*,#14348,.F.);
#19574=ORIENTED_EDGE('',*,*,#14349,.F.);
#19575=ORIENTED_EDGE('',*,*,#14350,.F.);
#19576=ORIENTED_EDGE('',*,*,#14351,.F.);
#19577=ORIENTED_EDGE('',*,*,#14352,.T.);
#19578=ORIENTED_EDGE('',*,*,#14353,.T.);
#19579=ORIENTED_EDGE('',*,*,#14352,.F.);
#19580=ORIENTED_EDGE('',*,*,#14354,.F.);
#19581=ORIENTED_EDGE('',*,*,#14355,.F.);
#19582=ORIENTED_EDGE('',*,*,#14356,.F.);
#19583=ORIENTED_EDGE('',*,*,#14357,.F.);
#19584=ORIENTED_EDGE('',*,*,#14358,.F.);
#19585=ORIENTED_EDGE('',*,*,#14359,.T.);
#19586=ORIENTED_EDGE('',*,*,#14360,.T.);
#19587=ORIENTED_EDGE('',*,*,#14359,.F.);
#19588=ORIENTED_EDGE('',*,*,#14361,.F.);
#19589=ORIENTED_EDGE('',*,*,#14362,.F.);
#19590=ORIENTED_EDGE('',*,*,#14363,.F.);
#19591=ORIENTED_EDGE('',*,*,#14364,.F.);
#19592=ORIENTED_EDGE('',*,*,#14365,.F.);
#19593=ORIENTED_EDGE('',*,*,#14366,.T.);
#19594=ORIENTED_EDGE('',*,*,#14367,.T.);
#19595=ORIENTED_EDGE('',*,*,#14366,.F.);
#19596=ORIENTED_EDGE('',*,*,#14368,.F.);
#19597=ORIENTED_EDGE('',*,*,#14369,.F.);
#19598=ORIENTED_EDGE('',*,*,#14370,.F.);
#19599=ORIENTED_EDGE('',*,*,#14371,.F.);
#19600=ORIENTED_EDGE('',*,*,#14372,.F.);
#19601=ORIENTED_EDGE('',*,*,#14373,.T.);
#19602=ORIENTED_EDGE('',*,*,#14374,.T.);
#19603=ORIENTED_EDGE('',*,*,#14373,.F.);
#19604=ORIENTED_EDGE('',*,*,#14375,.F.);
#19605=ORIENTED_EDGE('',*,*,#14376,.F.);
#19606=ORIENTED_EDGE('',*,*,#14377,.F.);
#19607=ORIENTED_EDGE('',*,*,#14378,.F.);
#19608=ORIENTED_EDGE('',*,*,#14379,.F.);
#19609=ORIENTED_EDGE('',*,*,#14380,.T.);
#19610=ORIENTED_EDGE('',*,*,#14381,.T.);
#19611=ORIENTED_EDGE('',*,*,#14380,.F.);
#19612=ORIENTED_EDGE('',*,*,#14382,.F.);
#19613=ORIENTED_EDGE('',*,*,#14383,.F.);
#19614=ORIENTED_EDGE('',*,*,#14384,.F.);
#19615=ORIENTED_EDGE('',*,*,#14385,.F.);
#19616=ORIENTED_EDGE('',*,*,#14386,.F.);
#19617=ORIENTED_EDGE('',*,*,#14387,.T.);
#19618=ORIENTED_EDGE('',*,*,#14388,.T.);
#19619=ORIENTED_EDGE('',*,*,#14387,.F.);
#19620=ORIENTED_EDGE('',*,*,#14389,.F.);
#19621=ORIENTED_EDGE('',*,*,#14390,.F.);
#19622=ORIENTED_EDGE('',*,*,#14391,.F.);
#19623=ORIENTED_EDGE('',*,*,#14392,.F.);
#19624=ORIENTED_EDGE('',*,*,#14393,.F.);
#19625=ORIENTED_EDGE('',*,*,#14394,.T.);
#19626=ORIENTED_EDGE('',*,*,#14395,.T.);
#19627=ORIENTED_EDGE('',*,*,#14394,.F.);
#19628=ORIENTED_EDGE('',*,*,#14396,.F.);
#19629=ORIENTED_EDGE('',*,*,#14397,.F.);
#19630=ORIENTED_EDGE('',*,*,#14398,.F.);
#19631=ORIENTED_EDGE('',*,*,#14399,.F.);
#19632=ORIENTED_EDGE('',*,*,#14400,.F.);
#19633=ORIENTED_EDGE('',*,*,#14401,.T.);
#19634=ORIENTED_EDGE('',*,*,#14402,.T.);
#19635=ORIENTED_EDGE('',*,*,#14401,.F.);
#19636=ORIENTED_EDGE('',*,*,#14403,.F.);
#19637=ORIENTED_EDGE('',*,*,#14404,.F.);
#19638=ORIENTED_EDGE('',*,*,#14405,.F.);
#19639=ORIENTED_EDGE('',*,*,#14406,.F.);
#19640=ORIENTED_EDGE('',*,*,#14407,.F.);
#19641=ORIENTED_EDGE('',*,*,#14408,.T.);
#19642=ORIENTED_EDGE('',*,*,#14409,.T.);
#19643=ORIENTED_EDGE('',*,*,#14408,.F.);
#19644=ORIENTED_EDGE('',*,*,#14410,.F.);
#19645=ORIENTED_EDGE('',*,*,#14411,.F.);
#19646=ORIENTED_EDGE('',*,*,#14412,.F.);
#19647=ORIENTED_EDGE('',*,*,#14413,.F.);
#19648=ORIENTED_EDGE('',*,*,#14414,.F.);
#19649=ORIENTED_EDGE('',*,*,#14415,.T.);
#19650=ORIENTED_EDGE('',*,*,#14416,.T.);
#19651=ORIENTED_EDGE('',*,*,#14415,.F.);
#19652=ORIENTED_EDGE('',*,*,#14417,.F.);
#19653=ORIENTED_EDGE('',*,*,#14418,.F.);
#19654=ORIENTED_EDGE('',*,*,#14419,.F.);
#19655=ORIENTED_EDGE('',*,*,#14420,.F.);
#19656=ORIENTED_EDGE('',*,*,#14421,.T.);
#19657=ORIENTED_EDGE('',*,*,#14315,.T.);
#19658=ORIENTED_EDGE('',*,*,#14422,.F.);
#19659=ORIENTED_EDGE('',*,*,#14423,.F.);
#19660=ORIENTED_EDGE('',*,*,#14424,.F.);
#19661=ORIENTED_EDGE('',*,*,#14312,.T.);
#19662=ORIENTED_EDGE('',*,*,#14425,.T.);
#19663=ORIENTED_EDGE('',*,*,#14333,.T.);
#19664=ORIENTED_EDGE('',*,*,#14330,.T.);
#19665=ORIENTED_EDGE('',*,*,#14425,.F.);
#19666=ORIENTED_EDGE('',*,*,#14322,.T.);
#19667=ORIENTED_EDGE('',*,*,#14426,.T.);
#19668=ORIENTED_EDGE('',*,*,#14334,.T.);
#19669=ORIENTED_EDGE('',*,*,#14422,.T.);
#19670=ORIENTED_EDGE('',*,*,#14314,.T.);
#19671=ORIENTED_EDGE('',*,*,#14427,.T.);
#19672=ORIENTED_EDGE('',*,*,#14328,.T.);
#19673=ORIENTED_EDGE('',*,*,#14428,.T.);
#19674=ORIENTED_EDGE('',*,*,#14342,.T.);
#19675=ORIENTED_EDGE('',*,*,#14429,.T.);
#19676=ORIENTED_EDGE('',*,*,#14356,.T.);
#19677=ORIENTED_EDGE('',*,*,#14430,.T.);
#19678=ORIENTED_EDGE('',*,*,#14370,.T.);
#19679=ORIENTED_EDGE('',*,*,#14431,.T.);
#19680=ORIENTED_EDGE('',*,*,#14384,.T.);
#19681=ORIENTED_EDGE('',*,*,#14432,.T.);
#19682=ORIENTED_EDGE('',*,*,#14398,.T.);
#19683=ORIENTED_EDGE('',*,*,#14433,.T.);
#19684=ORIENTED_EDGE('',*,*,#14412,.T.);
#19685=ORIENTED_EDGE('',*,*,#14434,.T.);
#19686=ORIENTED_EDGE('',*,*,#14435,.F.);
#19687=ORIENTED_EDGE('',*,*,#14436,.F.);
#19688=ORIENTED_EDGE('',*,*,#14437,.T.);
#19689=ORIENTED_EDGE('',*,*,#14426,.F.);
#19690=ORIENTED_EDGE('',*,*,#14321,.T.);
#19691=ORIENTED_EDGE('',*,*,#14438,.F.);
#19692=ORIENTED_EDGE('',*,*,#14439,.T.);
#19693=ORIENTED_EDGE('',*,*,#14440,.T.);
#19694=ORIENTED_EDGE('',*,*,#14441,.F.);
#19695=ORIENTED_EDGE('',*,*,#14442,.F.);
#19696=ORIENTED_EDGE('',*,*,#14419,.T.);
#19697=ORIENTED_EDGE('',*,*,#14443,.F.);
#19698=ORIENTED_EDGE('',*,*,#14405,.T.);
#19699=ORIENTED_EDGE('',*,*,#14444,.F.);
#19700=ORIENTED_EDGE('',*,*,#14391,.T.);
#19701=ORIENTED_EDGE('',*,*,#14445,.F.);
#19702=ORIENTED_EDGE('',*,*,#14377,.T.);
#19703=ORIENTED_EDGE('',*,*,#14446,.F.);
#19704=ORIENTED_EDGE('',*,*,#14363,.T.);
#19705=ORIENTED_EDGE('',*,*,#14447,.F.);
#19706=ORIENTED_EDGE('',*,*,#14349,.T.);
#19707=ORIENTED_EDGE('',*,*,#14448,.F.);
#19708=ORIENTED_EDGE('',*,*,#14335,.T.);
#19709=ORIENTED_EDGE('',*,*,#14427,.F.);
#19710=ORIENTED_EDGE('',*,*,#14313,.T.);
#19711=ORIENTED_EDGE('',*,*,#14424,.T.);
#19712=ORIENTED_EDGE('',*,*,#14329,.T.);
#19713=ORIENTED_EDGE('',*,*,#14449,.F.);
#19714=ORIENTED_EDGE('',*,*,#14326,.T.);
#19715=ORIENTED_EDGE('',*,*,#14450,.T.);
#19716=ORIENTED_EDGE('',*,*,#14347,.T.);
#19717=ORIENTED_EDGE('',*,*,#14344,.T.);
#19718=ORIENTED_EDGE('',*,*,#14450,.F.);
#19719=ORIENTED_EDGE('',*,*,#14336,.T.);
#19720=ORIENTED_EDGE('',*,*,#14448,.T.);
#19721=ORIENTED_EDGE('',*,*,#14348,.T.);
#19722=ORIENTED_EDGE('',*,*,#14428,.F.);
#19723=ORIENTED_EDGE('',*,*,#14327,.T.);
#19724=ORIENTED_EDGE('',*,*,#14449,.T.);
#19725=ORIENTED_EDGE('',*,*,#14343,.T.);
#19726=ORIENTED_EDGE('',*,*,#14451,.F.);
#19727=ORIENTED_EDGE('',*,*,#14340,.T.);
#19728=ORIENTED_EDGE('',*,*,#14452,.T.);
#19729=ORIENTED_EDGE('',*,*,#14361,.T.);
#19730=ORIENTED_EDGE('',*,*,#14358,.T.);
#19731=ORIENTED_EDGE('',*,*,#14452,.F.);
#19732=ORIENTED_EDGE('',*,*,#14350,.T.);
#19733=ORIENTED_EDGE('',*,*,#14447,.T.);
#19734=ORIENTED_EDGE('',*,*,#14362,.T.);
#19735=ORIENTED_EDGE('',*,*,#14429,.F.);
#19736=ORIENTED_EDGE('',*,*,#14341,.T.);
#19737=ORIENTED_EDGE('',*,*,#14451,.T.);
#19738=ORIENTED_EDGE('',*,*,#14357,.T.);
#19739=ORIENTED_EDGE('',*,*,#14453,.F.);
#19740=ORIENTED_EDGE('',*,*,#14364,.T.);
#19741=ORIENTED_EDGE('',*,*,#14446,.T.);
#19742=ORIENTED_EDGE('',*,*,#14376,.T.);
#19743=ORIENTED_EDGE('',*,*,#14454,.F.);
#19744=ORIENTED_EDGE('',*,*,#14354,.T.);
#19745=ORIENTED_EDGE('',*,*,#14453,.T.);
#19746=ORIENTED_EDGE('',*,*,#14375,.T.);
#19747=ORIENTED_EDGE('',*,*,#14372,.T.);
#19748=ORIENTED_EDGE('',*,*,#14430,.F.);
#19749=ORIENTED_EDGE('',*,*,#14355,.T.);
#19750=ORIENTED_EDGE('',*,*,#14454,.T.);
#19751=ORIENTED_EDGE('',*,*,#14371,.T.);
#19752=ORIENTED_EDGE('',*,*,#14455,.F.);
#19753=ORIENTED_EDGE('',*,*,#14368,.T.);
#19754=ORIENTED_EDGE('',*,*,#14456,.T.);
#19755=ORIENTED_EDGE('',*,*,#14389,.T.);
#19756=ORIENTED_EDGE('',*,*,#14386,.T.);
#19757=ORIENTED_EDGE('',*,*,#14456,.F.);
#19758=ORIENTED_EDGE('',*,*,#14378,.T.);
#19759=ORIENTED_EDGE('',*,*,#14445,.T.);
#19760=ORIENTED_EDGE('',*,*,#14390,.T.);
#19761=ORIENTED_EDGE('',*,*,#14431,.F.);
#19762=ORIENTED_EDGE('',*,*,#14369,.T.);
#19763=ORIENTED_EDGE('',*,*,#14455,.T.);
#19764=ORIENTED_EDGE('',*,*,#14385,.T.);
#19765=ORIENTED_EDGE('',*,*,#14457,.F.);
#19766=ORIENTED_EDGE('',*,*,#14382,.T.);
#19767=ORIENTED_EDGE('',*,*,#14458,.T.);
#19768=ORIENTED_EDGE('',*,*,#14403,.T.);
#19769=ORIENTED_EDGE('',*,*,#14400,.T.);
#19770=ORIENTED_EDGE('',*,*,#14458,.F.);
#19771=ORIENTED_EDGE('',*,*,#14392,.T.);
#19772=ORIENTED_EDGE('',*,*,#14444,.T.);
#19773=ORIENTED_EDGE('',*,*,#14404,.T.);
#19774=ORIENTED_EDGE('',*,*,#14432,.F.);
#19775=ORIENTED_EDGE('',*,*,#14383,.T.);
#19776=ORIENTED_EDGE('',*,*,#14457,.T.);
#19777=ORIENTED_EDGE('',*,*,#14399,.T.);
#19778=ORIENTED_EDGE('',*,*,#14459,.F.);
#19779=ORIENTED_EDGE('',*,*,#14396,.T.);
#19780=ORIENTED_EDGE('',*,*,#14460,.T.);
#19781=ORIENTED_EDGE('',*,*,#14417,.T.);
#19782=ORIENTED_EDGE('',*,*,#14414,.T.);
#19783=ORIENTED_EDGE('',*,*,#14460,.F.);
#19784=ORIENTED_EDGE('',*,*,#14406,.T.);
#19785=ORIENTED_EDGE('',*,*,#14443,.T.);
#19786=ORIENTED_EDGE('',*,*,#14418,.T.);
#19787=ORIENTED_EDGE('',*,*,#14433,.F.);
#19788=ORIENTED_EDGE('',*,*,#14397,.T.);
#19789=ORIENTED_EDGE('',*,*,#14459,.T.);
#19790=ORIENTED_EDGE('',*,*,#14413,.T.);
#19791=ORIENTED_EDGE('',*,*,#14461,.F.);
#19792=ORIENTED_EDGE('',*,*,#14410,.T.);
#19793=ORIENTED_EDGE('',*,*,#14462,.T.);
#19794=ORIENTED_EDGE('',*,*,#14463,.T.);
#19795=ORIENTED_EDGE('',*,*,#14462,.F.);
#19796=ORIENTED_EDGE('',*,*,#14420,.T.);
#19797=ORIENTED_EDGE('',*,*,#14442,.T.);
#19798=ORIENTED_EDGE('',*,*,#14464,.T.);
#19799=ORIENTED_EDGE('',*,*,#14423,.T.);
#19800=ORIENTED_EDGE('',*,*,#14437,.F.);
#19801=ORIENTED_EDGE('',*,*,#14465,.F.);
#19802=ORIENTED_EDGE('',*,*,#14466,.F.);
#19803=ORIENTED_EDGE('',*,*,#14467,.T.);
#19804=ORIENTED_EDGE('',*,*,#14468,.F.);
#19805=ORIENTED_EDGE('',*,*,#14469,.T.);
#19806=ORIENTED_EDGE('',*,*,#14470,.F.);
#19807=ORIENTED_EDGE('',*,*,#14471,.T.);
#19808=ORIENTED_EDGE('',*,*,#14472,.F.);
#19809=ORIENTED_EDGE('',*,*,#14473,.T.);
#19810=ORIENTED_EDGE('',*,*,#14474,.T.);
#19811=ORIENTED_EDGE('',*,*,#14475,.T.);
#19812=ORIENTED_EDGE('',*,*,#14476,.F.);
#19813=ORIENTED_EDGE('',*,*,#14477,.T.);
#19814=ORIENTED_EDGE('',*,*,#14478,.F.);
#19815=ORIENTED_EDGE('',*,*,#14479,.T.);
#19816=ORIENTED_EDGE('',*,*,#14480,.F.);
#19817=ORIENTED_EDGE('',*,*,#14481,.T.);
#19818=ORIENTED_EDGE('',*,*,#14482,.T.);
#19819=ORIENTED_EDGE('',*,*,#14483,.T.);
#19820=ORIENTED_EDGE('',*,*,#14484,.F.);
#19821=ORIENTED_EDGE('',*,*,#14485,.F.);
#19822=ORIENTED_EDGE('',*,*,#14486,.T.);
#19823=ORIENTED_EDGE('',*,*,#14487,.T.);
#19824=ORIENTED_EDGE('',*,*,#14488,.F.);
#19825=ORIENTED_EDGE('',*,*,#14489,.T.);
#19826=ORIENTED_EDGE('',*,*,#14490,.T.);
#19827=ORIENTED_EDGE('',*,*,#14491,.T.);
#19828=ORIENTED_EDGE('',*,*,#14492,.T.);
#19829=ORIENTED_EDGE('',*,*,#14493,.T.);
#19830=ORIENTED_EDGE('',*,*,#14494,.T.);
#19831=ORIENTED_EDGE('',*,*,#14495,.T.);
#19832=ORIENTED_EDGE('',*,*,#14496,.F.);
#19833=ORIENTED_EDGE('',*,*,#14497,.T.);
#19834=ORIENTED_EDGE('',*,*,#14498,.T.);
#19835=ORIENTED_EDGE('',*,*,#14499,.T.);
#19836=ORIENTED_EDGE('',*,*,#14500,.T.);
#19837=ORIENTED_EDGE('',*,*,#14501,.T.);
#19838=ORIENTED_EDGE('',*,*,#14502,.T.);
#19839=ORIENTED_EDGE('',*,*,#14503,.T.);
#19840=ORIENTED_EDGE('',*,*,#14504,.T.);
#19841=ORIENTED_EDGE('',*,*,#14505,.T.);
#19842=ORIENTED_EDGE('',*,*,#14439,.F.);
#19843=ORIENTED_EDGE('',*,*,#14506,.T.);
#19844=ORIENTED_EDGE('',*,*,#14507,.T.);
#19845=ORIENTED_EDGE('',*,*,#14435,.T.);
#19846=ORIENTED_EDGE('',*,*,#14508,.F.);
#19847=ORIENTED_EDGE('',*,*,#14463,.F.);
#19848=ORIENTED_EDGE('',*,*,#14464,.F.);
#19849=ORIENTED_EDGE('',*,*,#14441,.T.);
#19850=ORIENTED_EDGE('',*,*,#14509,.F.);
#19851=ORIENTED_EDGE('',*,*,#14510,.F.);
#19852=ORIENTED_EDGE('',*,*,#14511,.T.);
#19853=ORIENTED_EDGE('',*,*,#14512,.F.);
#19854=ORIENTED_EDGE('',*,*,#14513,.T.);
#19855=ORIENTED_EDGE('',*,*,#14514,.F.);
#19856=ORIENTED_EDGE('',*,*,#14515,.T.);
#19857=ORIENTED_EDGE('',*,*,#14516,.F.);
#19858=ORIENTED_EDGE('',*,*,#14517,.T.);
#19859=ORIENTED_EDGE('',*,*,#14518,.T.);
#19860=ORIENTED_EDGE('',*,*,#14519,.T.);
#19861=ORIENTED_EDGE('',*,*,#14520,.F.);
#19862=ORIENTED_EDGE('',*,*,#14521,.T.);
#19863=ORIENTED_EDGE('',*,*,#14522,.F.);
#19864=ORIENTED_EDGE('',*,*,#14523,.T.);
#19865=ORIENTED_EDGE('',*,*,#14524,.F.);
#19866=ORIENTED_EDGE('',*,*,#14525,.T.);
#19867=ORIENTED_EDGE('',*,*,#14526,.T.);
#19868=ORIENTED_EDGE('',*,*,#14527,.T.);
#19869=ORIENTED_EDGE('',*,*,#14528,.F.);
#19870=ORIENTED_EDGE('',*,*,#14529,.T.);
#19871=ORIENTED_EDGE('',*,*,#14530,.T.);
#19872=ORIENTED_EDGE('',*,*,#14531,.T.);
#19873=ORIENTED_EDGE('',*,*,#14532,.F.);
#19874=ORIENTED_EDGE('',*,*,#14533,.T.);
#19875=ORIENTED_EDGE('',*,*,#14534,.T.);
#19876=ORIENTED_EDGE('',*,*,#14535,.T.);
#19877=ORIENTED_EDGE('',*,*,#14536,.T.);
#19878=ORIENTED_EDGE('',*,*,#14537,.T.);
#19879=ORIENTED_EDGE('',*,*,#14538,.T.);
#19880=ORIENTED_EDGE('',*,*,#14539,.T.);
#19881=ORIENTED_EDGE('',*,*,#14540,.F.);
#19882=ORIENTED_EDGE('',*,*,#14541,.T.);
#19883=ORIENTED_EDGE('',*,*,#14542,.T.);
#19884=ORIENTED_EDGE('',*,*,#14543,.T.);
#19885=ORIENTED_EDGE('',*,*,#14544,.T.);
#19886=ORIENTED_EDGE('',*,*,#14545,.T.);
#19887=ORIENTED_EDGE('',*,*,#14546,.T.);
#19888=ORIENTED_EDGE('',*,*,#14547,.T.);
#19889=ORIENTED_EDGE('',*,*,#14548,.T.);
#19890=ORIENTED_EDGE('',*,*,#14549,.T.);
#19891=ORIENTED_EDGE('',*,*,#14516,.T.);
#19892=ORIENTED_EDGE('',*,*,#14550,.T.);
#19893=ORIENTED_EDGE('',*,*,#14498,.F.);
#19894=ORIENTED_EDGE('',*,*,#14551,.T.);
#19895=ORIENTED_EDGE('',*,*,#14494,.F.);
#19896=ORIENTED_EDGE('',*,*,#14552,.T.);
#19897=ORIENTED_EDGE('',*,*,#14520,.T.);
#19898=ORIENTED_EDGE('',*,*,#14553,.T.);
#19899=ORIENTED_EDGE('',*,*,#14490,.F.);
#19900=ORIENTED_EDGE('',*,*,#14554,.T.);
#19901=ORIENTED_EDGE('',*,*,#14524,.T.);
#19902=ORIENTED_EDGE('',*,*,#14555,.T.);
#19903=ORIENTED_EDGE('',*,*,#14528,.T.);
#19904=ORIENTED_EDGE('',*,*,#14556,.T.);
#19905=ORIENTED_EDGE('',*,*,#14486,.F.);
#19906=ORIENTED_EDGE('',*,*,#14557,.T.);
#19907=ORIENTED_EDGE('',*,*,#14472,.T.);
#19908=ORIENTED_EDGE('',*,*,#14558,.T.);
#19909=ORIENTED_EDGE('',*,*,#14542,.F.);
#19910=ORIENTED_EDGE('',*,*,#14559,.T.);
#19911=ORIENTED_EDGE('',*,*,#14534,.F.);
#19912=ORIENTED_EDGE('',*,*,#14560,.T.);
#19913=ORIENTED_EDGE('',*,*,#14480,.T.);
#19914=ORIENTED_EDGE('',*,*,#14561,.T.);
#19915=ORIENTED_EDGE('',*,*,#14529,.F.);
#19916=ORIENTED_EDGE('',*,*,#14557,.F.);
#19917=ORIENTED_EDGE('',*,*,#14485,.T.);
#19918=ORIENTED_EDGE('',*,*,#14562,.T.);
#19919=ORIENTED_EDGE('',*,*,#14311,.F.);
#19920=ORIENTED_EDGE('',*,*,#14325,.F.);
#19921=ORIENTED_EDGE('',*,*,#14339,.F.);
#19922=ORIENTED_EDGE('',*,*,#14353,.F.);
#19923=ORIENTED_EDGE('',*,*,#14367,.F.);
#19924=ORIENTED_EDGE('',*,*,#14381,.F.);
#19925=ORIENTED_EDGE('',*,*,#14395,.F.);
#19926=ORIENTED_EDGE('',*,*,#14409,.F.);
#19927=ORIENTED_EDGE('',*,*,#14549,.F.);
#19928=ORIENTED_EDGE('',*,*,#14563,.F.);
#19929=ORIENTED_EDGE('',*,*,#14465,.T.);
#19930=ORIENTED_EDGE('',*,*,#14436,.T.);
#19931=ORIENTED_EDGE('',*,*,#14548,.F.);
#19932=ORIENTED_EDGE('',*,*,#14564,.T.);
#19933=ORIENTED_EDGE('',*,*,#14466,.T.);
#19934=ORIENTED_EDGE('',*,*,#14563,.T.);
#19935=ORIENTED_EDGE('',*,*,#14468,.T.);
#19936=ORIENTED_EDGE('',*,*,#14565,.T.);
#19937=ORIENTED_EDGE('',*,*,#14546,.F.);
#19938=ORIENTED_EDGE('',*,*,#14566,.T.);
#19939=ORIENTED_EDGE('',*,*,#14470,.T.);
#19940=ORIENTED_EDGE('',*,*,#14567,.T.);
#19941=ORIENTED_EDGE('',*,*,#14544,.F.);
#19942=ORIENTED_EDGE('',*,*,#14568,.T.);
#19943=ORIENTED_EDGE('',*,*,#14538,.F.);
#19944=ORIENTED_EDGE('',*,*,#14569,.T.);
#19945=ORIENTED_EDGE('',*,*,#14476,.T.);
#19946=ORIENTED_EDGE('',*,*,#14570,.T.);
#19947=ORIENTED_EDGE('',*,*,#14536,.F.);
#19948=ORIENTED_EDGE('',*,*,#14571,.T.);
#19949=ORIENTED_EDGE('',*,*,#14478,.T.);
#19950=ORIENTED_EDGE('',*,*,#14572,.T.);
#19951=ORIENTED_EDGE('',*,*,#14484,.T.);
#19952=ORIENTED_EDGE('',*,*,#14573,.T.);
#19953=ORIENTED_EDGE('',*,*,#14530,.F.);
#19954=ORIENTED_EDGE('',*,*,#14562,.F.);
#19955=ORIENTED_EDGE('',*,*,#14482,.F.);
#19956=ORIENTED_EDGE('',*,*,#14574,.T.);
#19957=ORIENTED_EDGE('',*,*,#14532,.T.);
#19958=ORIENTED_EDGE('',*,*,#14575,.T.);
#19959=ORIENTED_EDGE('',*,*,#14540,.T.);
#19960=ORIENTED_EDGE('',*,*,#14576,.T.);
#19961=ORIENTED_EDGE('',*,*,#14474,.F.);
#19962=ORIENTED_EDGE('',*,*,#14577,.T.);
#19963=ORIENTED_EDGE('',*,*,#14481,.F.);
#19964=ORIENTED_EDGE('',*,*,#14560,.F.);
#19965=ORIENTED_EDGE('',*,*,#14533,.F.);
#19966=ORIENTED_EDGE('',*,*,#14574,.F.);
#19967=ORIENTED_EDGE('',*,*,#14479,.F.);
#19968=ORIENTED_EDGE('',*,*,#14571,.F.);
#19969=ORIENTED_EDGE('',*,*,#14535,.F.);
#19970=ORIENTED_EDGE('',*,*,#14561,.F.);
#19971=ORIENTED_EDGE('',*,*,#14477,.F.);
#19972=ORIENTED_EDGE('',*,*,#14569,.F.);
#19973=ORIENTED_EDGE('',*,*,#14537,.F.);
#19974=ORIENTED_EDGE('',*,*,#14572,.F.);
#19975=ORIENTED_EDGE('',*,*,#14539,.F.);
#19976=ORIENTED_EDGE('',*,*,#14570,.F.);
#19977=ORIENTED_EDGE('',*,*,#14475,.F.);
#19978=ORIENTED_EDGE('',*,*,#14576,.F.);
#19979=ORIENTED_EDGE('',*,*,#14469,.F.);
#19980=ORIENTED_EDGE('',*,*,#14566,.F.);
#19981=ORIENTED_EDGE('',*,*,#14545,.F.);
#19982=ORIENTED_EDGE('',*,*,#14567,.F.);
#19983=ORIENTED_EDGE('',*,*,#14471,.F.);
#19984=ORIENTED_EDGE('',*,*,#14568,.F.);
#19985=ORIENTED_EDGE('',*,*,#14543,.F.);
#19986=ORIENTED_EDGE('',*,*,#14558,.F.);
#19987=ORIENTED_EDGE('',*,*,#14473,.F.);
#19988=ORIENTED_EDGE('',*,*,#14559,.F.);
#19989=ORIENTED_EDGE('',*,*,#14541,.F.);
#19990=ORIENTED_EDGE('',*,*,#14577,.F.);
#19991=ORIENTED_EDGE('',*,*,#14531,.F.);
#19992=ORIENTED_EDGE('',*,*,#14573,.F.);
#19993=ORIENTED_EDGE('',*,*,#14483,.F.);
#19994=ORIENTED_EDGE('',*,*,#14575,.F.);
#19995=ORIENTED_EDGE('',*,*,#14467,.F.);
#19996=ORIENTED_EDGE('',*,*,#14564,.F.);
#19997=ORIENTED_EDGE('',*,*,#14547,.F.);
#19998=ORIENTED_EDGE('',*,*,#14565,.F.);
#19999=ORIENTED_EDGE('',*,*,#14492,.F.);
#20000=ORIENTED_EDGE('',*,*,#14578,.T.);
#20001=ORIENTED_EDGE('',*,*,#14522,.T.);
#20002=ORIENTED_EDGE('',*,*,#14579,.T.);
#20003=ORIENTED_EDGE('',*,*,#14514,.T.);
#20004=ORIENTED_EDGE('',*,*,#14580,.T.);
#20005=ORIENTED_EDGE('',*,*,#14500,.F.);
#20006=ORIENTED_EDGE('',*,*,#14581,.T.);
#20007=ORIENTED_EDGE('',*,*,#14512,.T.);
#20008=ORIENTED_EDGE('',*,*,#14582,.T.);
#20009=ORIENTED_EDGE('',*,*,#14502,.F.);
#20010=ORIENTED_EDGE('',*,*,#14583,.T.);
#20011=ORIENTED_EDGE('',*,*,#14504,.F.);
#20012=ORIENTED_EDGE('',*,*,#14584,.T.);
#20013=ORIENTED_EDGE('',*,*,#14510,.T.);
#20014=ORIENTED_EDGE('',*,*,#14585,.F.);
#20015=ORIENTED_EDGE('',*,*,#14509,.T.);
#20016=ORIENTED_EDGE('',*,*,#14440,.F.);
#20017=ORIENTED_EDGE('',*,*,#14505,.F.);
#20018=ORIENTED_EDGE('',*,*,#14585,.T.);
#20019=ORIENTED_EDGE('',*,*,#14526,.F.);
#20020=ORIENTED_EDGE('',*,*,#14586,.T.);
#20021=ORIENTED_EDGE('',*,*,#14488,.T.);
#20022=ORIENTED_EDGE('',*,*,#14587,.T.);
#20023=ORIENTED_EDGE('',*,*,#14496,.T.);
#20024=ORIENTED_EDGE('',*,*,#14588,.T.);
#20025=ORIENTED_EDGE('',*,*,#14518,.F.);
#20026=ORIENTED_EDGE('',*,*,#14589,.T.);
#20027=ORIENTED_EDGE('',*,*,#14525,.F.);
#20028=ORIENTED_EDGE('',*,*,#14554,.F.);
#20029=ORIENTED_EDGE('',*,*,#14489,.F.);
#20030=ORIENTED_EDGE('',*,*,#14586,.F.);
#20031=ORIENTED_EDGE('',*,*,#14491,.F.);
#20032=ORIENTED_EDGE('',*,*,#14555,.F.);
#20033=ORIENTED_EDGE('',*,*,#14523,.F.);
#20034=ORIENTED_EDGE('',*,*,#14578,.F.);
#20035=ORIENTED_EDGE('',*,*,#14493,.F.);
#20036=ORIENTED_EDGE('',*,*,#14579,.F.);
#20037=ORIENTED_EDGE('',*,*,#14521,.F.);
#20038=ORIENTED_EDGE('',*,*,#14552,.F.);
#20039=ORIENTED_EDGE('',*,*,#14495,.F.);
#20040=ORIENTED_EDGE('',*,*,#14553,.F.);
#20041=ORIENTED_EDGE('',*,*,#14519,.F.);
#20042=ORIENTED_EDGE('',*,*,#14588,.F.);
#20043=ORIENTED_EDGE('',*,*,#14501,.F.);
#20044=ORIENTED_EDGE('',*,*,#14580,.F.);
#20045=ORIENTED_EDGE('',*,*,#14513,.F.);
#20046=ORIENTED_EDGE('',*,*,#14583,.F.);
#20047=ORIENTED_EDGE('',*,*,#14499,.F.);
#20048=ORIENTED_EDGE('',*,*,#14550,.F.);
#20049=ORIENTED_EDGE('',*,*,#14515,.F.);
#20050=ORIENTED_EDGE('',*,*,#14581,.F.);
#20051=ORIENTED_EDGE('',*,*,#14517,.F.);
#20052=ORIENTED_EDGE('',*,*,#14551,.F.);
#20053=ORIENTED_EDGE('',*,*,#14497,.F.);
#20054=ORIENTED_EDGE('',*,*,#14589,.F.);
#20055=ORIENTED_EDGE('',*,*,#14487,.F.);
#20056=ORIENTED_EDGE('',*,*,#14556,.F.);
#20057=ORIENTED_EDGE('',*,*,#14527,.F.);
#20058=ORIENTED_EDGE('',*,*,#14587,.F.);
#20059=ORIENTED_EDGE('',*,*,#14503,.F.);
#20060=ORIENTED_EDGE('',*,*,#14582,.F.);
#20061=ORIENTED_EDGE('',*,*,#14511,.F.);
#20062=ORIENTED_EDGE('',*,*,#14584,.F.);
#20063=ORIENTED_EDGE('',*,*,#14434,.F.);
#20064=ORIENTED_EDGE('',*,*,#14411,.T.);
#20065=ORIENTED_EDGE('',*,*,#14461,.T.);
#20066=ORIENTED_EDGE('',*,*,#14508,.T.);
#20067=ORIENTED_EDGE('',*,*,#14590,.T.);
#20068=ORIENTED_EDGE('',*,*,#14319,.T.);
#20069=ORIENTED_EDGE('',*,*,#14316,.T.);
#20070=ORIENTED_EDGE('',*,*,#14421,.F.);
#20071=ORIENTED_EDGE('',*,*,#14507,.F.);
#20072=ORIENTED_EDGE('',*,*,#14438,.T.);
#20073=ORIENTED_EDGE('',*,*,#14320,.T.);
#20074=ORIENTED_EDGE('',*,*,#14590,.F.);
#20075=ORIENTED_EDGE('',*,*,#14506,.F.);
#20076=ORIENTED_EDGE('',*,*,#14407,.T.);
#20077=ORIENTED_EDGE('',*,*,#14416,.F.);
#20078=ORIENTED_EDGE('',*,*,#14393,.T.);
#20079=ORIENTED_EDGE('',*,*,#14402,.F.);
#20080=ORIENTED_EDGE('',*,*,#14379,.T.);
#20081=ORIENTED_EDGE('',*,*,#14388,.F.);
#20082=ORIENTED_EDGE('',*,*,#14365,.T.);
#20083=ORIENTED_EDGE('',*,*,#14374,.F.);
#20084=ORIENTED_EDGE('',*,*,#14351,.T.);
#20085=ORIENTED_EDGE('',*,*,#14360,.F.);
#20086=ORIENTED_EDGE('',*,*,#14337,.T.);
#20087=ORIENTED_EDGE('',*,*,#14346,.F.);
#20088=ORIENTED_EDGE('',*,*,#14323,.T.);
#20089=ORIENTED_EDGE('',*,*,#14332,.F.);
#20090=ORIENTED_EDGE('',*,*,#14309,.T.);
#20091=ORIENTED_EDGE('',*,*,#14318,.F.);
#20092=ORIENTED_EDGE('',*,*,#14591,.F.);
#20093=ORIENTED_EDGE('',*,*,#14592,.T.);
#20094=ORIENTED_EDGE('',*,*,#14593,.T.);
#20095=ORIENTED_EDGE('',*,*,#14592,.F.);
#20096=ORIENTED_EDGE('',*,*,#14594,.F.);
#20097=ORIENTED_EDGE('',*,*,#14595,.T.);
#20098=ORIENTED_EDGE('',*,*,#14596,.T.);
#20099=ORIENTED_EDGE('',*,*,#14595,.F.);
#20100=ORIENTED_EDGE('',*,*,#14597,.F.);
#20101=ORIENTED_EDGE('',*,*,#14598,.T.);
#20102=ORIENTED_EDGE('',*,*,#14599,.T.);
#20103=ORIENTED_EDGE('',*,*,#14598,.F.);
#20104=ORIENTED_EDGE('',*,*,#14600,.T.);
#20105=ORIENTED_EDGE('',*,*,#14591,.T.);
#20106=ORIENTED_EDGE('',*,*,#14600,.F.);
#20107=ORIENTED_EDGE('',*,*,#14601,.T.);
#20108=ORIENTED_EDGE('',*,*,#14594,.T.);
#20109=ORIENTED_EDGE('',*,*,#14601,.F.);
#20110=ORIENTED_EDGE('',*,*,#14602,.F.);
#20111=ORIENTED_EDGE('',*,*,#14603,.T.);
#20112=ORIENTED_EDGE('',*,*,#14604,.T.);
#20113=ORIENTED_EDGE('',*,*,#14603,.F.);
#20114=ORIENTED_EDGE('',*,*,#14605,.F.);
#20115=ORIENTED_EDGE('',*,*,#14606,.T.);
#20116=ORIENTED_EDGE('',*,*,#14607,.T.);
#20117=ORIENTED_EDGE('',*,*,#14606,.F.);
#20118=ORIENTED_EDGE('',*,*,#14608,.F.);
#20119=ORIENTED_EDGE('',*,*,#14609,.T.);
#20120=ORIENTED_EDGE('',*,*,#14610,.T.);
#20121=ORIENTED_EDGE('',*,*,#14609,.F.);
#20122=ORIENTED_EDGE('',*,*,#14611,.F.);
#20123=ORIENTED_EDGE('',*,*,#14612,.T.);
#20124=ORIENTED_EDGE('',*,*,#14613,.T.);
#20125=ORIENTED_EDGE('',*,*,#14612,.F.);
#20126=ORIENTED_EDGE('',*,*,#14614,.F.);
#20127=ORIENTED_EDGE('',*,*,#14615,.T.);
#20128=ORIENTED_EDGE('',*,*,#14616,.T.);
#20129=ORIENTED_EDGE('',*,*,#14615,.F.);
#20130=ORIENTED_EDGE('',*,*,#14617,.F.);
#20131=ORIENTED_EDGE('',*,*,#14618,.T.);
#20132=ORIENTED_EDGE('',*,*,#14619,.T.);
#20133=ORIENTED_EDGE('',*,*,#14618,.F.);
#20134=ORIENTED_EDGE('',*,*,#14620,.F.);
#20135=ORIENTED_EDGE('',*,*,#14621,.T.);
#20136=ORIENTED_EDGE('',*,*,#14622,.T.);
#20137=ORIENTED_EDGE('',*,*,#14621,.F.);
#20138=ORIENTED_EDGE('',*,*,#14623,.F.);
#20139=ORIENTED_EDGE('',*,*,#14624,.T.);
#20140=ORIENTED_EDGE('',*,*,#14625,.T.);
#20141=ORIENTED_EDGE('',*,*,#14626,.T.);
#20142=ORIENTED_EDGE('',*,*,#14627,.T.);
#20143=ORIENTED_EDGE('',*,*,#14628,.F.);
#20144=ORIENTED_EDGE('',*,*,#14624,.F.);
#20145=ORIENTED_EDGE('',*,*,#14629,.T.);
#20146=ORIENTED_EDGE('',*,*,#14614,.T.);
#20147=ORIENTED_EDGE('',*,*,#14629,.F.);
#20148=ORIENTED_EDGE('',*,*,#14630,.T.);
#20149=ORIENTED_EDGE('',*,*,#14617,.T.);
#20150=ORIENTED_EDGE('',*,*,#14630,.F.);
#20151=ORIENTED_EDGE('',*,*,#14631,.F.);
#20152=ORIENTED_EDGE('',*,*,#14632,.T.);
#20153=ORIENTED_EDGE('',*,*,#14633,.T.);
#20154=ORIENTED_EDGE('',*,*,#14634,.T.);
#20155=ORIENTED_EDGE('',*,*,#14635,.F.);
#20156=ORIENTED_EDGE('',*,*,#14636,.T.);
#20157=ORIENTED_EDGE('',*,*,#14632,.F.);
#20158=ORIENTED_EDGE('',*,*,#14637,.F.);
#20159=ORIENTED_EDGE('',*,*,#14638,.F.);
#20160=ORIENTED_EDGE('',*,*,#14639,.F.);
#20161=ORIENTED_EDGE('',*,*,#14640,.T.);
#20162=ORIENTED_EDGE('',*,*,#14641,.F.);
#20163=ORIENTED_EDGE('',*,*,#14642,.F.);
#20164=ORIENTED_EDGE('',*,*,#14640,.F.);
#20165=ORIENTED_EDGE('',*,*,#14643,.F.);
#20166=ORIENTED_EDGE('',*,*,#14644,.F.);
#20167=ORIENTED_EDGE('',*,*,#14645,.F.);
#20168=ORIENTED_EDGE('',*,*,#14646,.T.);
#20169=ORIENTED_EDGE('',*,*,#14647,.T.);
#20170=ORIENTED_EDGE('',*,*,#14641,.T.);
#20171=ORIENTED_EDGE('',*,*,#14642,.T.);
#20172=ORIENTED_EDGE('',*,*,#14647,.F.);
#20173=ORIENTED_EDGE('',*,*,#14648,.F.);
#20174=ORIENTED_EDGE('',*,*,#14649,.T.);
#20175=ORIENTED_EDGE('',*,*,#14650,.T.);
#20176=ORIENTED_EDGE('',*,*,#14649,.F.);
#20177=ORIENTED_EDGE('',*,*,#14651,.F.);
#20178=ORIENTED_EDGE('',*,*,#14652,.F.);
#20179=ORIENTED_EDGE('',*,*,#14653,.T.);
#20180=ORIENTED_EDGE('',*,*,#14654,.T.);
#20181=ORIENTED_EDGE('',*,*,#14655,.F.);
#20182=ORIENTED_EDGE('',*,*,#14656,.T.);
#20183=ORIENTED_EDGE('',*,*,#14657,.F.);
#20184=ORIENTED_EDGE('',*,*,#14658,.F.);
#20185=ORIENTED_EDGE('',*,*,#14659,.F.);
#20186=ORIENTED_EDGE('',*,*,#14660,.T.);
#20187=ORIENTED_EDGE('',*,*,#14661,.F.);
#20188=ORIENTED_EDGE('',*,*,#14662,.F.);
#20189=ORIENTED_EDGE('',*,*,#14663,.F.);
#20190=ORIENTED_EDGE('',*,*,#14664,.T.);
#20191=ORIENTED_EDGE('',*,*,#14665,.F.);
#20192=ORIENTED_EDGE('',*,*,#14666,.F.);
#20193=ORIENTED_EDGE('',*,*,#14667,.F.);
#20194=ORIENTED_EDGE('',*,*,#14668,.T.);
#20195=ORIENTED_EDGE('',*,*,#14669,.T.);
#20196=ORIENTED_EDGE('',*,*,#14670,.T.);
#20197=ORIENTED_EDGE('',*,*,#14671,.F.);
#20198=ORIENTED_EDGE('',*,*,#14672,.T.);
#20199=ORIENTED_EDGE('',*,*,#14673,.T.);
#20200=ORIENTED_EDGE('',*,*,#14674,.T.);
#20201=ORIENTED_EDGE('',*,*,#14675,.F.);
#20202=ORIENTED_EDGE('',*,*,#14676,.T.);
#20203=ORIENTED_EDGE('',*,*,#14677,.T.);
#20204=ORIENTED_EDGE('',*,*,#14678,.T.);
#20205=ORIENTED_EDGE('',*,*,#14679,.F.);
#20206=ORIENTED_EDGE('',*,*,#14680,.T.);
#20207=ORIENTED_EDGE('',*,*,#14681,.T.);
#20208=ORIENTED_EDGE('',*,*,#14682,.T.);
#20209=ORIENTED_EDGE('',*,*,#14683,.F.);
#20210=ORIENTED_EDGE('',*,*,#14684,.T.);
#20211=ORIENTED_EDGE('',*,*,#14685,.T.);
#20212=ORIENTED_EDGE('',*,*,#14686,.T.);
#20213=ORIENTED_EDGE('',*,*,#14687,.F.);
#20214=ORIENTED_EDGE('',*,*,#14688,.T.);
#20215=ORIENTED_EDGE('',*,*,#14689,.T.);
#20216=ORIENTED_EDGE('',*,*,#14690,.T.);
#20217=ORIENTED_EDGE('',*,*,#14691,.F.);
#20218=ORIENTED_EDGE('',*,*,#14692,.T.);
#20219=ORIENTED_EDGE('',*,*,#14693,.T.);
#20220=ORIENTED_EDGE('',*,*,#14694,.T.);
#20221=ORIENTED_EDGE('',*,*,#14695,.F.);
#20222=ORIENTED_EDGE('',*,*,#14696,.T.);
#20223=ORIENTED_EDGE('',*,*,#14697,.T.);
#20224=ORIENTED_EDGE('',*,*,#14698,.T.);
#20225=ORIENTED_EDGE('',*,*,#14699,.F.);
#20226=ORIENTED_EDGE('',*,*,#14700,.F.);
#20227=ORIENTED_EDGE('',*,*,#14701,.T.);
#20228=ORIENTED_EDGE('',*,*,#14702,.T.);
#20229=ORIENTED_EDGE('',*,*,#14703,.F.);
#20230=ORIENTED_EDGE('',*,*,#14704,.F.);
#20231=ORIENTED_EDGE('',*,*,#14705,.T.);
#20232=ORIENTED_EDGE('',*,*,#14700,.T.);
#20233=ORIENTED_EDGE('',*,*,#14706,.F.);
#20234=ORIENTED_EDGE('',*,*,#14707,.F.);
#20235=ORIENTED_EDGE('',*,*,#14708,.T.);
#20236=ORIENTED_EDGE('',*,*,#14709,.T.);
#20237=ORIENTED_EDGE('',*,*,#14710,.F.);
#20238=ORIENTED_EDGE('',*,*,#14711,.T.);
#20239=ORIENTED_EDGE('',*,*,#14712,.T.);
#20240=ORIENTED_EDGE('',*,*,#14707,.T.);
#20241=ORIENTED_EDGE('',*,*,#14713,.F.);
#20242=ORIENTED_EDGE('',*,*,#14714,.T.);
#20243=ORIENTED_EDGE('',*,*,#14715,.T.);
#20244=ORIENTED_EDGE('',*,*,#14716,.T.);
#20245=ORIENTED_EDGE('',*,*,#14717,.F.);
#20246=ORIENTED_EDGE('',*,*,#14718,.T.);
#20247=ORIENTED_EDGE('',*,*,#14719,.T.);
#20248=ORIENTED_EDGE('',*,*,#14720,.T.);
#20249=ORIENTED_EDGE('',*,*,#14721,.F.);
#20250=ORIENTED_EDGE('',*,*,#14722,.T.);
#20251=ORIENTED_EDGE('',*,*,#14723,.T.);
#20252=ORIENTED_EDGE('',*,*,#14724,.T.);
#20253=ORIENTED_EDGE('',*,*,#14725,.F.);
#20254=ORIENTED_EDGE('',*,*,#14726,.F.);
#20255=ORIENTED_EDGE('',*,*,#14727,.T.);
#20256=ORIENTED_EDGE('',*,*,#14728,.T.);
#20257=ORIENTED_EDGE('',*,*,#14729,.F.);
#20258=ORIENTED_EDGE('',*,*,#14682,.F.);
#20259=ORIENTED_EDGE('',*,*,#14730,.T.);
#20260=ORIENTED_EDGE('',*,*,#14726,.T.);
#20261=ORIENTED_EDGE('',*,*,#14731,.F.);
#20262=ORIENTED_EDGE('',*,*,#14732,.T.);
#20263=ORIENTED_EDGE('',*,*,#14733,.T.);
#20264=ORIENTED_EDGE('',*,*,#14734,.T.);
#20265=ORIENTED_EDGE('',*,*,#14735,.F.);
#20266=ORIENTED_EDGE('',*,*,#14736,.T.);
#20267=ORIENTED_EDGE('',*,*,#14737,.T.);
#20268=ORIENTED_EDGE('',*,*,#14738,.T.);
#20269=ORIENTED_EDGE('',*,*,#14739,.F.);
#20270=ORIENTED_EDGE('',*,*,#14740,.T.);
#20271=ORIENTED_EDGE('',*,*,#14741,.T.);
#20272=ORIENTED_EDGE('',*,*,#14742,.T.);
#20273=ORIENTED_EDGE('',*,*,#14743,.F.);
#20274=ORIENTED_EDGE('',*,*,#14744,.T.);
#20275=ORIENTED_EDGE('',*,*,#14745,.T.);
#20276=ORIENTED_EDGE('',*,*,#14746,.T.);
#20277=ORIENTED_EDGE('',*,*,#14747,.F.);
#20278=ORIENTED_EDGE('',*,*,#14716,.F.);
#20279=ORIENTED_EDGE('',*,*,#14748,.F.);
#20280=ORIENTED_EDGE('',*,*,#14711,.F.);
#20281=ORIENTED_EDGE('',*,*,#14749,.F.);
#20282=ORIENTED_EDGE('',*,*,#14702,.F.);
#20283=ORIENTED_EDGE('',*,*,#14750,.F.);
#20284=ORIENTED_EDGE('',*,*,#14696,.F.);
#20285=ORIENTED_EDGE('',*,*,#14718,.F.);
#20286=ORIENTED_EDGE('',*,*,#14751,.F.);
#20287=ORIENTED_EDGE('',*,*,#14724,.F.);
#20288=ORIENTED_EDGE('',*,*,#14752,.F.);
#20289=ORIENTED_EDGE('',*,*,#14722,.F.);
#20290=ORIENTED_EDGE('',*,*,#14753,.F.);
#20291=ORIENTED_EDGE('',*,*,#14674,.F.);
#20292=ORIENTED_EDGE('',*,*,#14754,.F.);
#20293=ORIENTED_EDGE('',*,*,#14672,.F.);
#20294=ORIENTED_EDGE('',*,*,#14755,.F.);
#20295=ORIENTED_EDGE('',*,*,#14742,.F.);
#20296=ORIENTED_EDGE('',*,*,#14756,.F.);
#20297=ORIENTED_EDGE('',*,*,#14740,.F.);
#20298=ORIENTED_EDGE('',*,*,#14757,.F.);
#20299=ORIENTED_EDGE('',*,*,#14728,.F.);
#20300=ORIENTED_EDGE('',*,*,#14758,.F.);
#20301=ORIENTED_EDGE('',*,*,#14744,.F.);
#20302=ORIENTED_EDGE('',*,*,#14759,.F.);
#20303=ORIENTED_EDGE('',*,*,#14720,.F.);
#20304=ORIENTED_EDGE('',*,*,#14760,.F.);
#20305=ORIENTED_EDGE('',*,*,#14668,.F.);
#20306=ORIENTED_EDGE('',*,*,#14761,.F.);
#20307=ORIENTED_EDGE('',*,*,#14746,.F.);
#20308=ORIENTED_EDGE('',*,*,#14762,.F.);
#20309=ORIENTED_EDGE('',*,*,#14763,.F.);
#20310=ORIENTED_EDGE('',*,*,#14670,.F.);
#20311=ORIENTED_EDGE('',*,*,#14764,.F.);
#20312=ORIENTED_EDGE('',*,*,#14714,.F.);
#20313=ORIENTED_EDGE('',*,*,#14765,.F.);
#20314=ORIENTED_EDGE('',*,*,#14698,.F.);
#20315=ORIENTED_EDGE('',*,*,#14766,.F.);
#20316=ORIENTED_EDGE('',*,*,#14692,.F.);
#20317=ORIENTED_EDGE('',*,*,#14736,.F.);
#20318=ORIENTED_EDGE('',*,*,#14767,.F.);
#20319=ORIENTED_EDGE('',*,*,#14694,.F.);
#20320=ORIENTED_EDGE('',*,*,#14768,.F.);
#20321=ORIENTED_EDGE('',*,*,#14676,.F.);
#20322=ORIENTED_EDGE('',*,*,#14769,.F.);
#20323=ORIENTED_EDGE('',*,*,#14738,.F.);
#20324=ORIENTED_EDGE('',*,*,#14770,.F.);
#20325=ORIENTED_EDGE('',*,*,#14688,.F.);
#20326=ORIENTED_EDGE('',*,*,#14771,.F.);
#20327=ORIENTED_EDGE('',*,*,#14678,.F.);
#20328=ORIENTED_EDGE('',*,*,#14772,.F.);
#20329=ORIENTED_EDGE('',*,*,#14684,.F.);
#20330=ORIENTED_EDGE('',*,*,#14773,.F.);
#20331=ORIENTED_EDGE('',*,*,#14690,.F.);
#20332=ORIENTED_EDGE('',*,*,#14774,.F.);
#20333=ORIENTED_EDGE('',*,*,#14732,.F.);
#20334=ORIENTED_EDGE('',*,*,#14775,.F.);
#20335=ORIENTED_EDGE('',*,*,#14686,.F.);
#20336=ORIENTED_EDGE('',*,*,#14776,.F.);
#20337=ORIENTED_EDGE('',*,*,#14680,.F.);
#20338=ORIENTED_EDGE('',*,*,#14777,.F.);
#20339=ORIENTED_EDGE('',*,*,#14734,.F.);
#20340=ORIENTED_EDGE('',*,*,#14778,.F.);
#20341=ORIENTED_EDGE('',*,*,#14648,.T.);
#20342=ORIENTED_EDGE('',*,*,#14646,.F.);
#20343=ORIENTED_EDGE('',*,*,#14779,.T.);
#20344=ORIENTED_EDGE('',*,*,#14780,.F.);
#20345=ORIENTED_EDGE('',*,*,#14781,.F.);
#20346=ORIENTED_EDGE('',*,*,#14782,.F.);
#20347=ORIENTED_EDGE('',*,*,#14783,.T.);
#20348=ORIENTED_EDGE('',*,*,#14784,.T.);
#20349=ORIENTED_EDGE('',*,*,#14785,.T.);
#20350=ORIENTED_EDGE('',*,*,#14782,.T.);
#20351=ORIENTED_EDGE('',*,*,#14786,.T.);
#20352=ORIENTED_EDGE('',*,*,#14787,.T.);
#20353=ORIENTED_EDGE('',*,*,#14788,.T.);
#20354=ORIENTED_EDGE('',*,*,#14708,.F.);
#20355=ORIENTED_EDGE('',*,*,#14712,.F.);
#20356=ORIENTED_EDGE('',*,*,#14748,.T.);
#20357=ORIENTED_EDGE('',*,*,#14715,.F.);
#20358=ORIENTED_EDGE('',*,*,#14764,.T.);
#20359=ORIENTED_EDGE('',*,*,#14669,.F.);
#20360=ORIENTED_EDGE('',*,*,#14762,.T.);
#20361=ORIENTED_EDGE('',*,*,#14745,.F.);
#20362=ORIENTED_EDGE('',*,*,#14760,.T.);
#20363=ORIENTED_EDGE('',*,*,#14719,.F.);
#20364=ORIENTED_EDGE('',*,*,#14752,.T.);
#20365=ORIENTED_EDGE('',*,*,#14723,.F.);
#20366=ORIENTED_EDGE('',*,*,#14754,.T.);
#20367=ORIENTED_EDGE('',*,*,#14673,.F.);
#20368=ORIENTED_EDGE('',*,*,#14756,.T.);
#20369=ORIENTED_EDGE('',*,*,#14741,.F.);
#20370=ORIENTED_EDGE('',*,*,#14758,.T.);
#20371=ORIENTED_EDGE('',*,*,#14727,.F.);
#20372=ORIENTED_EDGE('',*,*,#14730,.F.);
#20373=ORIENTED_EDGE('',*,*,#14681,.F.);
#20374=ORIENTED_EDGE('',*,*,#14778,.T.);
#20375=ORIENTED_EDGE('',*,*,#14733,.F.);
#20376=ORIENTED_EDGE('',*,*,#14776,.T.);
#20377=ORIENTED_EDGE('',*,*,#14685,.F.);
#20378=ORIENTED_EDGE('',*,*,#14774,.T.);
#20379=ORIENTED_EDGE('',*,*,#14689,.F.);
#20380=ORIENTED_EDGE('',*,*,#14772,.T.);
#20381=ORIENTED_EDGE('',*,*,#14677,.F.);
#20382=ORIENTED_EDGE('',*,*,#14770,.T.);
#20383=ORIENTED_EDGE('',*,*,#14737,.F.);
#20384=ORIENTED_EDGE('',*,*,#14768,.T.);
#20385=ORIENTED_EDGE('',*,*,#14693,.F.);
#20386=ORIENTED_EDGE('',*,*,#14766,.T.);
#20387=ORIENTED_EDGE('',*,*,#14697,.F.);
#20388=ORIENTED_EDGE('',*,*,#14750,.T.);
#20389=ORIENTED_EDGE('',*,*,#14701,.F.);
#20390=ORIENTED_EDGE('',*,*,#14705,.F.);
#20391=ORIENTED_EDGE('',*,*,#14650,.F.);
#20392=ORIENTED_EDGE('',*,*,#14789,.T.);
#20393=ORIENTED_EDGE('',*,*,#14790,.F.);
#20394=ORIENTED_EDGE('',*,*,#14779,.F.);
#20395=ORIENTED_EDGE('',*,*,#14785,.F.);
#20396=ORIENTED_EDGE('',*,*,#14791,.T.);
#20397=ORIENTED_EDGE('',*,*,#14792,.F.);
#20398=ORIENTED_EDGE('',*,*,#14789,.F.);
#20399=ORIENTED_EDGE('',*,*,#14784,.F.);
#20400=ORIENTED_EDGE('',*,*,#14704,.T.);
#20401=ORIENTED_EDGE('',*,*,#14793,.F.);
#20402=ORIENTED_EDGE('',*,*,#14791,.F.);
#20403=ORIENTED_EDGE('',*,*,#14783,.F.);
#20404=ORIENTED_EDGE('',*,*,#14794,.T.);
#20405=ORIENTED_EDGE('',*,*,#14795,.F.);
#20406=ORIENTED_EDGE('',*,*,#14709,.F.);
#20407=ORIENTED_EDGE('',*,*,#14788,.F.);
#20408=ORIENTED_EDGE('',*,*,#14796,.T.);
#20409=ORIENTED_EDGE('',*,*,#14797,.F.);
#20410=ORIENTED_EDGE('',*,*,#14794,.F.);
#20411=ORIENTED_EDGE('',*,*,#14787,.F.);
#20412=ORIENTED_EDGE('',*,*,#14781,.T.);
#20413=ORIENTED_EDGE('',*,*,#14798,.F.);
#20414=ORIENTED_EDGE('',*,*,#14796,.F.);
#20415=ORIENTED_EDGE('',*,*,#14786,.F.);
#20416=ORIENTED_EDGE('',*,*,#14799,.T.);
#20417=ORIENTED_EDGE('',*,*,#14645,.T.);
#20418=ORIENTED_EDGE('',*,*,#14800,.F.);
#20419=ORIENTED_EDGE('',*,*,#14801,.F.);
#20420=ORIENTED_EDGE('',*,*,#14637,.T.);
#20421=ORIENTED_EDGE('',*,*,#14799,.F.);
#20422=ORIENTED_EDGE('',*,*,#14802,.F.);
#20423=ORIENTED_EDGE('',*,*,#14803,.T.);
#20424=ORIENTED_EDGE('',*,*,#14804,.T.);
#20425=ORIENTED_EDGE('',*,*,#14638,.T.);
#20426=ORIENTED_EDGE('',*,*,#14803,.F.);
#20427=ORIENTED_EDGE('',*,*,#14805,.F.);
#20428=ORIENTED_EDGE('',*,*,#14806,.T.);
#20429=ORIENTED_EDGE('',*,*,#14639,.T.);
#20430=ORIENTED_EDGE('',*,*,#14804,.F.);
#20431=ORIENTED_EDGE('',*,*,#14807,.F.);
#20432=ORIENTED_EDGE('',*,*,#14808,.T.);
#20433=ORIENTED_EDGE('',*,*,#14643,.T.);
#20434=ORIENTED_EDGE('',*,*,#14806,.F.);
#20435=ORIENTED_EDGE('',*,*,#14809,.F.);
#20436=ORIENTED_EDGE('',*,*,#14800,.T.);
#20437=ORIENTED_EDGE('',*,*,#14644,.T.);
#20438=ORIENTED_EDGE('',*,*,#14808,.F.);
#20439=ORIENTED_EDGE('',*,*,#14810,.F.);
#20440=ORIENTED_EDGE('',*,*,#14801,.T.);
#20441=ORIENTED_EDGE('',*,*,#14810,.T.);
#20442=ORIENTED_EDGE('',*,*,#14809,.T.);
#20443=ORIENTED_EDGE('',*,*,#14807,.T.);
#20444=ORIENTED_EDGE('',*,*,#14805,.T.);
#20445=ORIENTED_EDGE('',*,*,#14802,.T.);
#20446=ORIENTED_EDGE('',*,*,#14710,.T.);
#20447=ORIENTED_EDGE('',*,*,#14706,.T.);
#20448=ORIENTED_EDGE('',*,*,#14795,.T.);
#20449=ORIENTED_EDGE('',*,*,#14797,.T.);
#20450=ORIENTED_EDGE('',*,*,#14798,.T.);
#20451=ORIENTED_EDGE('',*,*,#14780,.T.);
#20452=ORIENTED_EDGE('',*,*,#14790,.T.);
#20453=ORIENTED_EDGE('',*,*,#14792,.T.);
#20454=ORIENTED_EDGE('',*,*,#14793,.T.);
#20455=ORIENTED_EDGE('',*,*,#14703,.T.);
#20456=ORIENTED_EDGE('',*,*,#14699,.T.);
#20457=ORIENTED_EDGE('',*,*,#14749,.T.);
#20458=ORIENTED_EDGE('',*,*,#14695,.T.);
#20459=ORIENTED_EDGE('',*,*,#14765,.T.);
#20460=ORIENTED_EDGE('',*,*,#14691,.T.);
#20461=ORIENTED_EDGE('',*,*,#14767,.T.);
#20462=ORIENTED_EDGE('',*,*,#14735,.T.);
#20463=ORIENTED_EDGE('',*,*,#14769,.T.);
#20464=ORIENTED_EDGE('',*,*,#14675,.T.);
#20465=ORIENTED_EDGE('',*,*,#14771,.T.);
#20466=ORIENTED_EDGE('',*,*,#14687,.T.);
#20467=ORIENTED_EDGE('',*,*,#14773,.T.);
#20468=ORIENTED_EDGE('',*,*,#14683,.T.);
#20469=ORIENTED_EDGE('',*,*,#14775,.T.);
#20470=ORIENTED_EDGE('',*,*,#14731,.T.);
#20471=ORIENTED_EDGE('',*,*,#14777,.T.);
#20472=ORIENTED_EDGE('',*,*,#14679,.T.);
#20473=ORIENTED_EDGE('',*,*,#14729,.T.);
#20474=ORIENTED_EDGE('',*,*,#14725,.T.);
#20475=ORIENTED_EDGE('',*,*,#14757,.T.);
#20476=ORIENTED_EDGE('',*,*,#14739,.T.);
#20477=ORIENTED_EDGE('',*,*,#14755,.T.);
#20478=ORIENTED_EDGE('',*,*,#14671,.T.);
#20479=ORIENTED_EDGE('',*,*,#14753,.T.);
#20480=ORIENTED_EDGE('',*,*,#14721,.T.);
#20481=ORIENTED_EDGE('',*,*,#14751,.T.);
#20482=ORIENTED_EDGE('',*,*,#14717,.T.);
#20483=ORIENTED_EDGE('',*,*,#14759,.T.);
#20484=ORIENTED_EDGE('',*,*,#14743,.T.);
#20485=ORIENTED_EDGE('',*,*,#14761,.T.);
#20486=ORIENTED_EDGE('',*,*,#14667,.T.);
#20487=ORIENTED_EDGE('',*,*,#14763,.T.);
#20488=ORIENTED_EDGE('',*,*,#14713,.T.);
#20489=ORIENTED_EDGE('',*,*,#14747,.T.);
#20490=ORIENTED_EDGE('',*,*,#14811,.F.);
#20491=ORIENTED_EDGE('',*,*,#14812,.F.);
#20492=ORIENTED_EDGE('',*,*,#14813,.F.);
#20493=ORIENTED_EDGE('',*,*,#14814,.F.);
#20494=ORIENTED_EDGE('',*,*,#14815,.F.);
#20495=ORIENTED_EDGE('',*,*,#14816,.F.);
#20496=ORIENTED_EDGE('',*,*,#14817,.F.);
#20497=ORIENTED_EDGE('',*,*,#14818,.F.);
#20498=ORIENTED_EDGE('',*,*,#14819,.F.);
#20499=ORIENTED_EDGE('',*,*,#14820,.F.);
#20500=ORIENTED_EDGE('',*,*,#14821,.F.);
#20501=ORIENTED_EDGE('',*,*,#14822,.F.);
#20502=ORIENTED_EDGE('',*,*,#14823,.F.);
#20503=ORIENTED_EDGE('',*,*,#14824,.F.);
#20504=ORIENTED_EDGE('',*,*,#14825,.F.);
#20505=ORIENTED_EDGE('',*,*,#14826,.F.);
#20506=ORIENTED_EDGE('',*,*,#14827,.F.);
#20507=ORIENTED_EDGE('',*,*,#14828,.F.);
#20508=ORIENTED_EDGE('',*,*,#14829,.F.);
#20509=ORIENTED_EDGE('',*,*,#14830,.F.);
#20510=ORIENTED_EDGE('',*,*,#14831,.F.);
#20511=ORIENTED_EDGE('',*,*,#14832,.F.);
#20512=ORIENTED_EDGE('',*,*,#14833,.F.);
#20513=ORIENTED_EDGE('',*,*,#14834,.F.);
#20514=ORIENTED_EDGE('',*,*,#14835,.F.);
#20515=ORIENTED_EDGE('',*,*,#14836,.F.);
#20516=ORIENTED_EDGE('',*,*,#14837,.F.);
#20517=ORIENTED_EDGE('',*,*,#14838,.F.);
#20518=ORIENTED_EDGE('',*,*,#14839,.F.);
#20519=ORIENTED_EDGE('',*,*,#14840,.F.);
#20520=ORIENTED_EDGE('',*,*,#14841,.F.);
#20521=ORIENTED_EDGE('',*,*,#14842,.F.);
#20522=ORIENTED_EDGE('',*,*,#14843,.F.);
#20523=ORIENTED_EDGE('',*,*,#14844,.F.);
#20524=ORIENTED_EDGE('',*,*,#14845,.F.);
#20525=ORIENTED_EDGE('',*,*,#14846,.F.);
#20526=ORIENTED_EDGE('',*,*,#14847,.F.);
#20527=ORIENTED_EDGE('',*,*,#14848,.F.);
#20528=ORIENTED_EDGE('',*,*,#14849,.F.);
#20529=ORIENTED_EDGE('',*,*,#14850,.F.);
#20530=ORIENTED_EDGE('',*,*,#14851,.F.);
#20531=ORIENTED_EDGE('',*,*,#14852,.F.);
#20532=ORIENTED_EDGE('',*,*,#14853,.F.);
#20533=ORIENTED_EDGE('',*,*,#14854,.F.);
#20534=ORIENTED_EDGE('',*,*,#14855,.F.);
#20535=ORIENTED_EDGE('',*,*,#14856,.F.);
#20536=ORIENTED_EDGE('',*,*,#14811,.T.);
#20537=ORIENTED_EDGE('',*,*,#14857,.T.);
#20538=ORIENTED_EDGE('',*,*,#14858,.F.);
#20539=ORIENTED_EDGE('',*,*,#14859,.F.);
#20540=ORIENTED_EDGE('',*,*,#14812,.T.);
#20541=ORIENTED_EDGE('',*,*,#14856,.T.);
#20542=ORIENTED_EDGE('',*,*,#14860,.F.);
#20543=ORIENTED_EDGE('',*,*,#14861,.F.);
#20544=ORIENTED_EDGE('',*,*,#14813,.T.);
#20545=ORIENTED_EDGE('',*,*,#14859,.T.);
#20546=ORIENTED_EDGE('',*,*,#14862,.F.);
#20547=ORIENTED_EDGE('',*,*,#14863,.F.);
#20548=ORIENTED_EDGE('',*,*,#14814,.T.);
#20549=ORIENTED_EDGE('',*,*,#14861,.T.);
#20550=ORIENTED_EDGE('',*,*,#14864,.F.);
#20551=ORIENTED_EDGE('',*,*,#14865,.F.);
#20552=ORIENTED_EDGE('',*,*,#14815,.T.);
#20553=ORIENTED_EDGE('',*,*,#14863,.T.);
#20554=ORIENTED_EDGE('',*,*,#14866,.F.);
#20555=ORIENTED_EDGE('',*,*,#14867,.F.);
#20556=ORIENTED_EDGE('',*,*,#14816,.T.);
#20557=ORIENTED_EDGE('',*,*,#14865,.T.);
#20558=ORIENTED_EDGE('',*,*,#14868,.F.);
#20559=ORIENTED_EDGE('',*,*,#14869,.F.);
#20560=ORIENTED_EDGE('',*,*,#14817,.T.);
#20561=ORIENTED_EDGE('',*,*,#14867,.T.);
#20562=ORIENTED_EDGE('',*,*,#14870,.F.);
#20563=ORIENTED_EDGE('',*,*,#14871,.F.);
#20564=ORIENTED_EDGE('',*,*,#14818,.T.);
#20565=ORIENTED_EDGE('',*,*,#14869,.T.);
#20566=ORIENTED_EDGE('',*,*,#14872,.F.);
#20567=ORIENTED_EDGE('',*,*,#14873,.F.);
#20568=ORIENTED_EDGE('',*,*,#14819,.T.);
#20569=ORIENTED_EDGE('',*,*,#14871,.T.);
#20570=ORIENTED_EDGE('',*,*,#14874,.F.);
#20571=ORIENTED_EDGE('',*,*,#14875,.F.);
#20572=ORIENTED_EDGE('',*,*,#14820,.T.);
#20573=ORIENTED_EDGE('',*,*,#14873,.T.);
#20574=ORIENTED_EDGE('',*,*,#14876,.F.);
#20575=ORIENTED_EDGE('',*,*,#14877,.F.);
#20576=ORIENTED_EDGE('',*,*,#14821,.T.);
#20577=ORIENTED_EDGE('',*,*,#14875,.T.);
#20578=ORIENTED_EDGE('',*,*,#14878,.F.);
#20579=ORIENTED_EDGE('',*,*,#14879,.F.);
#20580=ORIENTED_EDGE('',*,*,#14822,.T.);
#20581=ORIENTED_EDGE('',*,*,#14877,.T.);
#20582=ORIENTED_EDGE('',*,*,#14880,.F.);
#20583=ORIENTED_EDGE('',*,*,#14881,.F.);
#20584=ORIENTED_EDGE('',*,*,#14823,.T.);
#20585=ORIENTED_EDGE('',*,*,#14879,.T.);
#20586=ORIENTED_EDGE('',*,*,#14882,.F.);
#20587=ORIENTED_EDGE('',*,*,#14883,.F.);
#20588=ORIENTED_EDGE('',*,*,#14824,.T.);
#20589=ORIENTED_EDGE('',*,*,#14881,.T.);
#20590=ORIENTED_EDGE('',*,*,#14884,.F.);
#20591=ORIENTED_EDGE('',*,*,#14885,.F.);
#20592=ORIENTED_EDGE('',*,*,#14825,.T.);
#20593=ORIENTED_EDGE('',*,*,#14883,.T.);
#20594=ORIENTED_EDGE('',*,*,#14886,.F.);
#20595=ORIENTED_EDGE('',*,*,#14887,.F.);
#20596=ORIENTED_EDGE('',*,*,#14826,.T.);
#20597=ORIENTED_EDGE('',*,*,#14885,.T.);
#20598=ORIENTED_EDGE('',*,*,#14888,.F.);
#20599=ORIENTED_EDGE('',*,*,#14889,.F.);
#20600=ORIENTED_EDGE('',*,*,#14827,.T.);
#20601=ORIENTED_EDGE('',*,*,#14887,.T.);
#20602=ORIENTED_EDGE('',*,*,#14890,.F.);
#20603=ORIENTED_EDGE('',*,*,#14891,.F.);
#20604=ORIENTED_EDGE('',*,*,#14828,.T.);
#20605=ORIENTED_EDGE('',*,*,#14889,.T.);
#20606=ORIENTED_EDGE('',*,*,#14892,.F.);
#20607=ORIENTED_EDGE('',*,*,#14893,.F.);
#20608=ORIENTED_EDGE('',*,*,#14829,.T.);
#20609=ORIENTED_EDGE('',*,*,#14891,.T.);
#20610=ORIENTED_EDGE('',*,*,#14894,.F.);
#20611=ORIENTED_EDGE('',*,*,#14895,.F.);
#20612=ORIENTED_EDGE('',*,*,#14830,.T.);
#20613=ORIENTED_EDGE('',*,*,#14893,.T.);
#20614=ORIENTED_EDGE('',*,*,#14896,.F.);
#20615=ORIENTED_EDGE('',*,*,#14897,.F.);
#20616=ORIENTED_EDGE('',*,*,#14831,.T.);
#20617=ORIENTED_EDGE('',*,*,#14895,.T.);
#20618=ORIENTED_EDGE('',*,*,#14898,.F.);
#20619=ORIENTED_EDGE('',*,*,#14899,.F.);
#20620=ORIENTED_EDGE('',*,*,#14832,.T.);
#20621=ORIENTED_EDGE('',*,*,#14897,.T.);
#20622=ORIENTED_EDGE('',*,*,#14900,.F.);
#20623=ORIENTED_EDGE('',*,*,#14901,.F.);
#20624=ORIENTED_EDGE('',*,*,#14833,.T.);
#20625=ORIENTED_EDGE('',*,*,#14899,.T.);
#20626=ORIENTED_EDGE('',*,*,#14902,.F.);
#20627=ORIENTED_EDGE('',*,*,#14903,.F.);
#20628=ORIENTED_EDGE('',*,*,#14834,.T.);
#20629=ORIENTED_EDGE('',*,*,#14901,.T.);
#20630=ORIENTED_EDGE('',*,*,#14904,.F.);
#20631=ORIENTED_EDGE('',*,*,#14905,.F.);
#20632=ORIENTED_EDGE('',*,*,#14835,.T.);
#20633=ORIENTED_EDGE('',*,*,#14903,.T.);
#20634=ORIENTED_EDGE('',*,*,#14906,.F.);
#20635=ORIENTED_EDGE('',*,*,#14907,.F.);
#20636=ORIENTED_EDGE('',*,*,#14836,.T.);
#20637=ORIENTED_EDGE('',*,*,#14905,.T.);
#20638=ORIENTED_EDGE('',*,*,#14908,.F.);
#20639=ORIENTED_EDGE('',*,*,#14909,.F.);
#20640=ORIENTED_EDGE('',*,*,#14837,.T.);
#20641=ORIENTED_EDGE('',*,*,#14907,.T.);
#20642=ORIENTED_EDGE('',*,*,#14910,.F.);
#20643=ORIENTED_EDGE('',*,*,#14911,.F.);
#20644=ORIENTED_EDGE('',*,*,#14838,.T.);
#20645=ORIENTED_EDGE('',*,*,#14909,.T.);
#20646=ORIENTED_EDGE('',*,*,#14912,.F.);
#20647=ORIENTED_EDGE('',*,*,#14913,.F.);
#20648=ORIENTED_EDGE('',*,*,#14839,.T.);
#20649=ORIENTED_EDGE('',*,*,#14911,.T.);
#20650=ORIENTED_EDGE('',*,*,#14914,.F.);
#20651=ORIENTED_EDGE('',*,*,#14915,.F.);
#20652=ORIENTED_EDGE('',*,*,#14840,.T.);
#20653=ORIENTED_EDGE('',*,*,#14913,.T.);
#20654=ORIENTED_EDGE('',*,*,#14916,.F.);
#20655=ORIENTED_EDGE('',*,*,#14917,.F.);
#20656=ORIENTED_EDGE('',*,*,#14841,.T.);
#20657=ORIENTED_EDGE('',*,*,#14915,.T.);
#20658=ORIENTED_EDGE('',*,*,#14918,.F.);
#20659=ORIENTED_EDGE('',*,*,#14919,.F.);
#20660=ORIENTED_EDGE('',*,*,#14842,.T.);
#20661=ORIENTED_EDGE('',*,*,#14917,.T.);
#20662=ORIENTED_EDGE('',*,*,#14920,.F.);
#20663=ORIENTED_EDGE('',*,*,#14921,.F.);
#20664=ORIENTED_EDGE('',*,*,#14843,.T.);
#20665=ORIENTED_EDGE('',*,*,#14919,.T.);
#20666=ORIENTED_EDGE('',*,*,#14922,.F.);
#20667=ORIENTED_EDGE('',*,*,#14923,.F.);
#20668=ORIENTED_EDGE('',*,*,#14844,.T.);
#20669=ORIENTED_EDGE('',*,*,#14921,.T.);
#20670=ORIENTED_EDGE('',*,*,#14924,.F.);
#20671=ORIENTED_EDGE('',*,*,#14925,.F.);
#20672=ORIENTED_EDGE('',*,*,#14845,.T.);
#20673=ORIENTED_EDGE('',*,*,#14923,.T.);
#20674=ORIENTED_EDGE('',*,*,#14926,.F.);
#20675=ORIENTED_EDGE('',*,*,#14927,.F.);
#20676=ORIENTED_EDGE('',*,*,#14846,.T.);
#20677=ORIENTED_EDGE('',*,*,#14925,.T.);
#20678=ORIENTED_EDGE('',*,*,#14928,.F.);
#20679=ORIENTED_EDGE('',*,*,#14929,.F.);
#20680=ORIENTED_EDGE('',*,*,#14847,.T.);
#20681=ORIENTED_EDGE('',*,*,#14927,.T.);
#20682=ORIENTED_EDGE('',*,*,#14930,.F.);
#20683=ORIENTED_EDGE('',*,*,#14931,.F.);
#20684=ORIENTED_EDGE('',*,*,#14848,.T.);
#20685=ORIENTED_EDGE('',*,*,#14929,.T.);
#20686=ORIENTED_EDGE('',*,*,#14932,.F.);
#20687=ORIENTED_EDGE('',*,*,#14933,.F.);
#20688=ORIENTED_EDGE('',*,*,#14849,.T.);
#20689=ORIENTED_EDGE('',*,*,#14931,.T.);
#20690=ORIENTED_EDGE('',*,*,#14934,.F.);
#20691=ORIENTED_EDGE('',*,*,#14935,.F.);
#20692=ORIENTED_EDGE('',*,*,#14850,.T.);
#20693=ORIENTED_EDGE('',*,*,#14933,.T.);
#20694=ORIENTED_EDGE('',*,*,#14936,.F.);
#20695=ORIENTED_EDGE('',*,*,#14937,.F.);
#20696=ORIENTED_EDGE('',*,*,#14851,.T.);
#20697=ORIENTED_EDGE('',*,*,#14935,.T.);
#20698=ORIENTED_EDGE('',*,*,#14938,.F.);
#20699=ORIENTED_EDGE('',*,*,#14939,.F.);
#20700=ORIENTED_EDGE('',*,*,#14852,.T.);
#20701=ORIENTED_EDGE('',*,*,#14937,.T.);
#20702=ORIENTED_EDGE('',*,*,#14940,.F.);
#20703=ORIENTED_EDGE('',*,*,#14941,.F.);
#20704=ORIENTED_EDGE('',*,*,#14853,.T.);
#20705=ORIENTED_EDGE('',*,*,#14939,.T.);
#20706=ORIENTED_EDGE('',*,*,#14942,.F.);
#20707=ORIENTED_EDGE('',*,*,#14857,.F.);
#20708=ORIENTED_EDGE('',*,*,#14854,.T.);
#20709=ORIENTED_EDGE('',*,*,#14941,.T.);
#20710=ORIENTED_EDGE('',*,*,#14631,.T.);
#20711=ORIENTED_EDGE('',*,*,#14636,.F.);
#20712=ORIENTED_EDGE('',*,*,#14943,.T.);
#20713=ORIENTED_EDGE('',*,*,#14944,.T.);
#20714=ORIENTED_EDGE('',*,*,#14945,.T.);
#20715=ORIENTED_EDGE('',*,*,#14946,.F.);
#20716=ORIENTED_EDGE('',*,*,#14947,.F.);
#20717=ORIENTED_EDGE('',*,*,#14948,.F.);
#20718=ORIENTED_EDGE('',*,*,#14949,.F.);
#20719=ORIENTED_EDGE('',*,*,#14950,.F.);
#20720=ORIENTED_EDGE('',*,*,#14951,.F.);
#20721=ORIENTED_EDGE('',*,*,#14952,.F.);
#20722=ORIENTED_EDGE('',*,*,#14953,.F.);
#20723=ORIENTED_EDGE('',*,*,#14954,.T.);
#20724=ORIENTED_EDGE('',*,*,#14955,.T.);
#20725=ORIENTED_EDGE('',*,*,#14956,.T.);
#20726=ORIENTED_EDGE('',*,*,#14957,.T.);
#20727=ORIENTED_EDGE('',*,*,#14958,.T.);
#20728=ORIENTED_EDGE('',*,*,#14959,.T.);
#20729=ORIENTED_EDGE('',*,*,#14960,.T.);
#20730=ORIENTED_EDGE('',*,*,#14961,.T.);
#20731=ORIENTED_EDGE('',*,*,#14962,.T.);
#20732=ORIENTED_EDGE('',*,*,#14963,.T.);
#20733=ORIENTED_EDGE('',*,*,#14964,.T.);
#20734=ORIENTED_EDGE('',*,*,#14965,.T.);
#20735=ORIENTED_EDGE('',*,*,#14966,.T.);
#20736=ORIENTED_EDGE('',*,*,#14967,.T.);
#20737=ORIENTED_EDGE('',*,*,#14968,.T.);
#20738=ORIENTED_EDGE('',*,*,#14969,.T.);
#20739=ORIENTED_EDGE('',*,*,#14970,.T.);
#20740=ORIENTED_EDGE('',*,*,#14971,.T.);
#20741=ORIENTED_EDGE('',*,*,#14972,.T.);
#20742=ORIENTED_EDGE('',*,*,#14973,.T.);
#20743=ORIENTED_EDGE('',*,*,#14974,.T.);
#20744=ORIENTED_EDGE('',*,*,#14975,.T.);
#20745=ORIENTED_EDGE('',*,*,#14976,.T.);
#20746=ORIENTED_EDGE('',*,*,#14977,.T.);
#20747=ORIENTED_EDGE('',*,*,#14978,.T.);
#20748=ORIENTED_EDGE('',*,*,#14979,.T.);
#20749=ORIENTED_EDGE('',*,*,#14980,.T.);
#20750=ORIENTED_EDGE('',*,*,#14981,.T.);
#20751=ORIENTED_EDGE('',*,*,#14982,.T.);
#20752=ORIENTED_EDGE('',*,*,#14983,.T.);
#20753=ORIENTED_EDGE('',*,*,#14984,.T.);
#20754=ORIENTED_EDGE('',*,*,#14985,.T.);
#20755=ORIENTED_EDGE('',*,*,#14986,.T.);
#20756=ORIENTED_EDGE('',*,*,#14987,.T.);
#20757=ORIENTED_EDGE('',*,*,#14988,.T.);
#20758=ORIENTED_EDGE('',*,*,#14989,.T.);
#20759=ORIENTED_EDGE('',*,*,#14990,.T.);
#20760=ORIENTED_EDGE('',*,*,#14991,.F.);
#20761=ORIENTED_EDGE('',*,*,#14992,.F.);
#20762=ORIENTED_EDGE('',*,*,#14993,.F.);
#20763=ORIENTED_EDGE('',*,*,#14994,.T.);
#20764=ORIENTED_EDGE('',*,*,#14633,.F.);
#20765=ORIENTED_EDGE('',*,*,#14945,.F.);
#20766=ORIENTED_EDGE('',*,*,#14995,.T.);
#20767=ORIENTED_EDGE('',*,*,#14996,.T.);
#20768=ORIENTED_EDGE('',*,*,#14997,.F.);
#20769=ORIENTED_EDGE('',*,*,#14943,.F.);
#20770=ORIENTED_EDGE('',*,*,#14635,.T.);
#20771=ORIENTED_EDGE('',*,*,#14998,.T.);
#20772=ORIENTED_EDGE('',*,*,#14995,.F.);
#20773=ORIENTED_EDGE('',*,*,#14944,.F.);
#20774=ORIENTED_EDGE('',*,*,#14997,.T.);
#20775=ORIENTED_EDGE('',*,*,#14623,.T.);
#20776=ORIENTED_EDGE('',*,*,#14625,.F.);
#20777=ORIENTED_EDGE('',*,*,#14999,.T.);
#20778=ORIENTED_EDGE('',*,*,#15000,.T.);
#20779=ORIENTED_EDGE('',*,*,#15001,.T.);
#20780=ORIENTED_EDGE('',*,*,#15002,.T.);
#20781=ORIENTED_EDGE('',*,*,#15003,.T.);
#20782=ORIENTED_EDGE('',*,*,#14990,.F.);
#20783=ORIENTED_EDGE('',*,*,#15004,.F.);
#20784=ORIENTED_EDGE('',*,*,#15003,.F.);
#20785=ORIENTED_EDGE('',*,*,#15005,.T.);
#20786=ORIENTED_EDGE('',*,*,#15006,.T.);
#20787=ORIENTED_EDGE('',*,*,#14991,.T.);
#20788=ORIENTED_EDGE('',*,*,#15006,.F.);
#20789=ORIENTED_EDGE('',*,*,#15007,.T.);
#20790=ORIENTED_EDGE('',*,*,#15008,.T.);
#20791=ORIENTED_EDGE('',*,*,#14992,.T.);
#20792=ORIENTED_EDGE('',*,*,#15008,.F.);
#20793=ORIENTED_EDGE('',*,*,#15009,.T.);
#20794=ORIENTED_EDGE('',*,*,#15010,.T.);
#20795=ORIENTED_EDGE('',*,*,#14993,.T.);
#20796=ORIENTED_EDGE('',*,*,#15011,.F.);
#20797=ORIENTED_EDGE('',*,*,#15012,.T.);
#20798=ORIENTED_EDGE('',*,*,#14946,.T.);
#20799=ORIENTED_EDGE('',*,*,#15010,.F.);
#20800=ORIENTED_EDGE('',*,*,#15013,.T.);
#20801=ORIENTED_EDGE('',*,*,#15014,.T.);
#20802=ORIENTED_EDGE('',*,*,#14950,.T.);
#20803=ORIENTED_EDGE('',*,*,#15015,.F.);
#20804=ORIENTED_EDGE('',*,*,#15014,.F.);
#20805=ORIENTED_EDGE('',*,*,#15016,.T.);
#20806=ORIENTED_EDGE('',*,*,#15017,.T.);
#20807=ORIENTED_EDGE('',*,*,#14951,.T.);
#20808=ORIENTED_EDGE('',*,*,#15017,.F.);
#20809=ORIENTED_EDGE('',*,*,#15018,.T.);
#20810=ORIENTED_EDGE('',*,*,#15019,.T.);
#20811=ORIENTED_EDGE('',*,*,#14952,.T.);
#20812=ORIENTED_EDGE('',*,*,#15019,.F.);
#20813=ORIENTED_EDGE('',*,*,#15020,.T.);
#20814=ORIENTED_EDGE('',*,*,#15021,.T.);
#20815=ORIENTED_EDGE('',*,*,#14953,.T.);
#20816=ORIENTED_EDGE('',*,*,#15022,.T.);
#20817=ORIENTED_EDGE('',*,*,#15023,.T.);
#20818=ORIENTED_EDGE('',*,*,#14954,.F.);
#20819=ORIENTED_EDGE('',*,*,#15021,.F.);
#20820=ORIENTED_EDGE('',*,*,#15024,.T.);
#20821=ORIENTED_EDGE('',*,*,#15025,.T.);
#20822=ORIENTED_EDGE('',*,*,#14955,.F.);
#20823=ORIENTED_EDGE('',*,*,#15023,.F.);
#20824=ORIENTED_EDGE('',*,*,#15026,.T.);
#20825=ORIENTED_EDGE('',*,*,#15027,.F.);
#20826=ORIENTED_EDGE('',*,*,#14956,.F.);
#20827=ORIENTED_EDGE('',*,*,#15025,.F.);
#20828=ORIENTED_EDGE('',*,*,#15028,.T.);
#20829=ORIENTED_EDGE('',*,*,#15029,.T.);
#20830=ORIENTED_EDGE('',*,*,#14957,.F.);
#20831=ORIENTED_EDGE('',*,*,#15027,.T.);
#20832=ORIENTED_EDGE('',*,*,#15030,.T.);
#20833=ORIENTED_EDGE('',*,*,#15031,.F.);
#20834=ORIENTED_EDGE('',*,*,#14958,.F.);
#20835=ORIENTED_EDGE('',*,*,#15029,.F.);
#20836=ORIENTED_EDGE('',*,*,#15032,.T.);
#20837=ORIENTED_EDGE('',*,*,#15033,.T.);
#20838=ORIENTED_EDGE('',*,*,#14959,.F.);
#20839=ORIENTED_EDGE('',*,*,#15031,.T.);
#20840=ORIENTED_EDGE('',*,*,#15033,.F.);
#20841=ORIENTED_EDGE('',*,*,#15034,.T.);
#20842=ORIENTED_EDGE('',*,*,#15035,.F.);
#20843=ORIENTED_EDGE('',*,*,#14960,.F.);
#20844=ORIENTED_EDGE('',*,*,#15036,.T.);
#20845=ORIENTED_EDGE('',*,*,#15037,.T.);
#20846=ORIENTED_EDGE('',*,*,#14961,.F.);
#20847=ORIENTED_EDGE('',*,*,#15035,.T.);
#20848=ORIENTED_EDGE('',*,*,#15037,.F.);
#20849=ORIENTED_EDGE('',*,*,#15038,.T.);
#20850=ORIENTED_EDGE('',*,*,#15039,.F.);
#20851=ORIENTED_EDGE('',*,*,#14962,.F.);
#20852=ORIENTED_EDGE('',*,*,#15040,.T.);
#20853=ORIENTED_EDGE('',*,*,#15041,.T.);
#20854=ORIENTED_EDGE('',*,*,#14963,.F.);
#20855=ORIENTED_EDGE('',*,*,#15039,.T.);
#20856=ORIENTED_EDGE('',*,*,#15041,.F.);
#20857=ORIENTED_EDGE('',*,*,#15042,.T.);
#20858=ORIENTED_EDGE('',*,*,#15043,.F.);
#20859=ORIENTED_EDGE('',*,*,#14964,.F.);
#20860=ORIENTED_EDGE('',*,*,#15044,.T.);
#20861=ORIENTED_EDGE('',*,*,#15045,.T.);
#20862=ORIENTED_EDGE('',*,*,#14965,.F.);
#20863=ORIENTED_EDGE('',*,*,#15043,.T.);
#20864=ORIENTED_EDGE('',*,*,#15045,.F.);
#20865=ORIENTED_EDGE('',*,*,#15046,.T.);
#20866=ORIENTED_EDGE('',*,*,#15047,.F.);
#20867=ORIENTED_EDGE('',*,*,#14966,.F.);
#20868=ORIENTED_EDGE('',*,*,#15048,.T.);
#20869=ORIENTED_EDGE('',*,*,#15049,.T.);
#20870=ORIENTED_EDGE('',*,*,#14967,.F.);
#20871=ORIENTED_EDGE('',*,*,#15047,.T.);
#20872=ORIENTED_EDGE('',*,*,#15049,.F.);
#20873=ORIENTED_EDGE('',*,*,#15050,.T.);
#20874=ORIENTED_EDGE('',*,*,#15051,.F.);
#20875=ORIENTED_EDGE('',*,*,#14968,.F.);
#20876=ORIENTED_EDGE('',*,*,#15052,.T.);
#20877=ORIENTED_EDGE('',*,*,#15053,.T.);
#20878=ORIENTED_EDGE('',*,*,#14969,.F.);
#20879=ORIENTED_EDGE('',*,*,#15051,.T.);
#20880=ORIENTED_EDGE('',*,*,#15053,.F.);
#20881=ORIENTED_EDGE('',*,*,#15054,.T.);
#20882=ORIENTED_EDGE('',*,*,#15055,.F.);
#20883=ORIENTED_EDGE('',*,*,#14970,.F.);
#20884=ORIENTED_EDGE('',*,*,#15056,.T.);
#20885=ORIENTED_EDGE('',*,*,#15057,.T.);
#20886=ORIENTED_EDGE('',*,*,#14971,.F.);
#20887=ORIENTED_EDGE('',*,*,#15055,.T.);
#20888=ORIENTED_EDGE('',*,*,#15058,.T.);
#20889=ORIENTED_EDGE('',*,*,#15059,.T.);
#20890=ORIENTED_EDGE('',*,*,#14972,.F.);
#20891=ORIENTED_EDGE('',*,*,#15057,.F.);
#20892=ORIENTED_EDGE('',*,*,#15060,.T.);
#20893=ORIENTED_EDGE('',*,*,#15061,.T.);
#20894=ORIENTED_EDGE('',*,*,#14973,.F.);
#20895=ORIENTED_EDGE('',*,*,#15059,.F.);
#20896=ORIENTED_EDGE('',*,*,#15061,.F.);
#20897=ORIENTED_EDGE('',*,*,#15062,.T.);
#20898=ORIENTED_EDGE('',*,*,#15063,.F.);
#20899=ORIENTED_EDGE('',*,*,#14974,.F.);
#20900=ORIENTED_EDGE('',*,*,#15064,.T.);
#20901=ORIENTED_EDGE('',*,*,#15065,.T.);
#20902=ORIENTED_EDGE('',*,*,#14975,.F.);
#20903=ORIENTED_EDGE('',*,*,#15063,.T.);
#20904=ORIENTED_EDGE('',*,*,#15065,.F.);
#20905=ORIENTED_EDGE('',*,*,#15066,.T.);
#20906=ORIENTED_EDGE('',*,*,#15067,.F.);
#20907=ORIENTED_EDGE('',*,*,#14976,.F.);
#20908=ORIENTED_EDGE('',*,*,#15068,.T.);
#20909=ORIENTED_EDGE('',*,*,#15069,.T.);
#20910=ORIENTED_EDGE('',*,*,#14977,.F.);
#20911=ORIENTED_EDGE('',*,*,#15067,.T.);
#20912=ORIENTED_EDGE('',*,*,#15069,.F.);
#20913=ORIENTED_EDGE('',*,*,#15070,.T.);
#20914=ORIENTED_EDGE('',*,*,#15071,.F.);
#20915=ORIENTED_EDGE('',*,*,#14978,.F.);
#20916=ORIENTED_EDGE('',*,*,#15072,.T.);
#20917=ORIENTED_EDGE('',*,*,#15073,.T.);
#20918=ORIENTED_EDGE('',*,*,#14979,.F.);
#20919=ORIENTED_EDGE('',*,*,#15071,.T.);
#20920=ORIENTED_EDGE('',*,*,#15073,.F.);
#20921=ORIENTED_EDGE('',*,*,#15074,.T.);
#20922=ORIENTED_EDGE('',*,*,#15075,.F.);
#20923=ORIENTED_EDGE('',*,*,#14980,.F.);
#20924=ORIENTED_EDGE('',*,*,#15076,.T.);
#20925=ORIENTED_EDGE('',*,*,#15077,.T.);
#20926=ORIENTED_EDGE('',*,*,#14981,.F.);
#20927=ORIENTED_EDGE('',*,*,#15075,.T.);
#20928=ORIENTED_EDGE('',*,*,#15077,.F.);
#20929=ORIENTED_EDGE('',*,*,#15078,.T.);
#20930=ORIENTED_EDGE('',*,*,#15079,.F.);
#20931=ORIENTED_EDGE('',*,*,#14982,.F.);
#20932=ORIENTED_EDGE('',*,*,#15080,.T.);
#20933=ORIENTED_EDGE('',*,*,#15081,.T.);
#20934=ORIENTED_EDGE('',*,*,#14983,.F.);
#20935=ORIENTED_EDGE('',*,*,#15079,.T.);
#20936=ORIENTED_EDGE('',*,*,#15081,.F.);
#20937=ORIENTED_EDGE('',*,*,#15082,.T.);
#20938=ORIENTED_EDGE('',*,*,#15083,.F.);
#20939=ORIENTED_EDGE('',*,*,#14984,.F.);
#20940=ORIENTED_EDGE('',*,*,#15084,.T.);
#20941=ORIENTED_EDGE('',*,*,#15085,.T.);
#20942=ORIENTED_EDGE('',*,*,#14985,.F.);
#20943=ORIENTED_EDGE('',*,*,#15083,.T.);
#20944=ORIENTED_EDGE('',*,*,#15086,.T.);
#20945=ORIENTED_EDGE('',*,*,#15087,.F.);
#20946=ORIENTED_EDGE('',*,*,#14986,.F.);
#20947=ORIENTED_EDGE('',*,*,#15085,.F.);
#20948=ORIENTED_EDGE('',*,*,#15088,.T.);
#20949=ORIENTED_EDGE('',*,*,#15089,.T.);
#20950=ORIENTED_EDGE('',*,*,#14987,.F.);
#20951=ORIENTED_EDGE('',*,*,#15087,.T.);
#20952=ORIENTED_EDGE('',*,*,#15090,.T.);
#20953=ORIENTED_EDGE('',*,*,#15091,.F.);
#20954=ORIENTED_EDGE('',*,*,#14988,.F.);
#20955=ORIENTED_EDGE('',*,*,#15089,.F.);
#20956=ORIENTED_EDGE('',*,*,#15092,.T.);
#20957=ORIENTED_EDGE('',*,*,#15004,.T.);
#20958=ORIENTED_EDGE('',*,*,#14989,.F.);
#20959=ORIENTED_EDGE('',*,*,#15091,.T.);
#20960=ORIENTED_EDGE('',*,*,#14620,.T.);
#20961=ORIENTED_EDGE('',*,*,#14998,.F.);
#20962=ORIENTED_EDGE('',*,*,#14996,.F.);
#20963=ORIENTED_EDGE('',*,*,#14634,.F.);
#20964=ORIENTED_EDGE('',*,*,#14994,.F.);
#20965=ORIENTED_EDGE('',*,*,#15093,.T.);
#20966=ORIENTED_EDGE('',*,*,#15094,.T.);
#20967=ORIENTED_EDGE('',*,*,#15095,.T.);
#20968=ORIENTED_EDGE('',*,*,#15096,.T.);
#20969=ORIENTED_EDGE('',*,*,#15097,.T.);
#20970=ORIENTED_EDGE('',*,*,#15098,.T.);
#20971=ORIENTED_EDGE('',*,*,#15099,.T.);
#20972=ORIENTED_EDGE('',*,*,#15100,.F.);
#20973=ORIENTED_EDGE('',*,*,#15101,.T.);
#20974=ORIENTED_EDGE('',*,*,#14626,.F.);
#20975=ORIENTED_EDGE('',*,*,#15001,.F.);
#20976=ORIENTED_EDGE('',*,*,#15102,.T.);
#20977=ORIENTED_EDGE('',*,*,#15103,.T.);
#20978=ORIENTED_EDGE('',*,*,#15104,.F.);
#20979=ORIENTED_EDGE('',*,*,#14999,.F.);
#20980=ORIENTED_EDGE('',*,*,#14628,.T.);
#20981=ORIENTED_EDGE('',*,*,#15105,.T.);
#20982=ORIENTED_EDGE('',*,*,#15102,.F.);
#20983=ORIENTED_EDGE('',*,*,#15000,.F.);
#20984=ORIENTED_EDGE('',*,*,#15104,.T.);
#20985=ORIENTED_EDGE('',*,*,#15106,.F.);
#20986=ORIENTED_EDGE('',*,*,#15093,.F.);
#20987=ORIENTED_EDGE('',*,*,#15107,.F.);
#20988=ORIENTED_EDGE('',*,*,#15108,.F.);
#20989=ORIENTED_EDGE('',*,*,#15106,.T.);
#20990=ORIENTED_EDGE('',*,*,#15109,.F.);
#20991=ORIENTED_EDGE('',*,*,#15110,.T.);
#20992=ORIENTED_EDGE('',*,*,#15111,.T.);
#20993=ORIENTED_EDGE('',*,*,#15112,.F.);
#20994=ORIENTED_EDGE('',*,*,#15094,.F.);
#20995=ORIENTED_EDGE('',*,*,#15113,.T.);
#20996=ORIENTED_EDGE('',*,*,#15114,.T.);
#20997=ORIENTED_EDGE('',*,*,#15115,.F.);
#20998=ORIENTED_EDGE('',*,*,#15110,.F.);
#20999=ORIENTED_EDGE('',*,*,#15116,.T.);
#21000=ORIENTED_EDGE('',*,*,#15117,.T.);
#21001=ORIENTED_EDGE('',*,*,#15118,.T.);
#21002=ORIENTED_EDGE('',*,*,#15119,.F.);
#21003=ORIENTED_EDGE('',*,*,#15119,.T.);
#21004=ORIENTED_EDGE('',*,*,#15120,.F.);
#21005=ORIENTED_EDGE('',*,*,#15121,.T.);
#21006=ORIENTED_EDGE('',*,*,#15098,.F.);
#21007=ORIENTED_EDGE('',*,*,#15122,.F.);
#21008=ORIENTED_EDGE('',*,*,#15123,.T.);
#21009=ORIENTED_EDGE('',*,*,#15121,.F.);
#21010=ORIENTED_EDGE('',*,*,#15124,.F.);
#21011=ORIENTED_EDGE('',*,*,#15125,.T.);
#21012=ORIENTED_EDGE('',*,*,#15099,.F.);
#21013=ORIENTED_EDGE('',*,*,#15092,.F.);
#21014=ORIENTED_EDGE('',*,*,#15090,.F.);
#21015=ORIENTED_EDGE('',*,*,#15088,.F.);
#21016=ORIENTED_EDGE('',*,*,#15086,.F.);
#21017=ORIENTED_EDGE('',*,*,#15084,.F.);
#21018=ORIENTED_EDGE('',*,*,#15082,.F.);
#21019=ORIENTED_EDGE('',*,*,#15080,.F.);
#21020=ORIENTED_EDGE('',*,*,#15078,.F.);
#21021=ORIENTED_EDGE('',*,*,#15076,.F.);
#21022=ORIENTED_EDGE('',*,*,#15074,.F.);
#21023=ORIENTED_EDGE('',*,*,#15072,.F.);
#21024=ORIENTED_EDGE('',*,*,#15070,.F.);
#21025=ORIENTED_EDGE('',*,*,#15068,.F.);
#21026=ORIENTED_EDGE('',*,*,#15066,.F.);
#21027=ORIENTED_EDGE('',*,*,#15064,.F.);
#21028=ORIENTED_EDGE('',*,*,#15062,.F.);
#21029=ORIENTED_EDGE('',*,*,#15060,.F.);
#21030=ORIENTED_EDGE('',*,*,#15058,.F.);
#21031=ORIENTED_EDGE('',*,*,#15056,.F.);
#21032=ORIENTED_EDGE('',*,*,#15054,.F.);
#21033=ORIENTED_EDGE('',*,*,#15052,.F.);
#21034=ORIENTED_EDGE('',*,*,#15050,.F.);
#21035=ORIENTED_EDGE('',*,*,#15048,.F.);
#21036=ORIENTED_EDGE('',*,*,#15046,.F.);
#21037=ORIENTED_EDGE('',*,*,#15044,.F.);
#21038=ORIENTED_EDGE('',*,*,#15042,.F.);
#21039=ORIENTED_EDGE('',*,*,#15040,.F.);
#21040=ORIENTED_EDGE('',*,*,#15038,.F.);
#21041=ORIENTED_EDGE('',*,*,#15036,.F.);
#21042=ORIENTED_EDGE('',*,*,#15034,.F.);
#21043=ORIENTED_EDGE('',*,*,#15032,.F.);
#21044=ORIENTED_EDGE('',*,*,#15030,.F.);
#21045=ORIENTED_EDGE('',*,*,#15028,.F.);
#21046=ORIENTED_EDGE('',*,*,#15026,.F.);
#21047=ORIENTED_EDGE('',*,*,#15024,.F.);
#21048=ORIENTED_EDGE('',*,*,#15022,.F.);
#21049=ORIENTED_EDGE('',*,*,#15020,.F.);
#21050=ORIENTED_EDGE('',*,*,#15018,.F.);
#21051=ORIENTED_EDGE('',*,*,#15016,.F.);
#21052=ORIENTED_EDGE('',*,*,#15013,.F.);
#21053=ORIENTED_EDGE('',*,*,#15009,.F.);
#21054=ORIENTED_EDGE('',*,*,#15007,.F.);
#21055=ORIENTED_EDGE('',*,*,#15005,.F.);
#21056=ORIENTED_EDGE('',*,*,#15002,.F.);
#21057=ORIENTED_EDGE('',*,*,#15126,.T.);
#21058=ORIENTED_EDGE('',*,*,#15127,.T.);
#21059=ORIENTED_EDGE('',*,*,#15128,.T.);
#21060=ORIENTED_EDGE('',*,*,#15129,.T.);
#21061=ORIENTED_EDGE('',*,*,#15130,.T.);
#21062=ORIENTED_EDGE('',*,*,#15131,.T.);
#21063=ORIENTED_EDGE('',*,*,#15132,.T.);
#21064=ORIENTED_EDGE('',*,*,#15133,.T.);
#21065=ORIENTED_EDGE('',*,*,#15134,.T.);
#21066=ORIENTED_EDGE('',*,*,#15135,.T.);
#21067=ORIENTED_EDGE('',*,*,#15136,.T.);
#21068=ORIENTED_EDGE('',*,*,#15137,.T.);
#21069=ORIENTED_EDGE('',*,*,#15138,.T.);
#21070=ORIENTED_EDGE('',*,*,#15139,.T.);
#21071=ORIENTED_EDGE('',*,*,#15140,.T.);
#21072=ORIENTED_EDGE('',*,*,#15141,.T.);
#21073=ORIENTED_EDGE('',*,*,#15142,.T.);
#21074=ORIENTED_EDGE('',*,*,#15143,.T.);
#21075=ORIENTED_EDGE('',*,*,#15144,.T.);
#21076=ORIENTED_EDGE('',*,*,#15145,.T.);
#21077=ORIENTED_EDGE('',*,*,#15146,.T.);
#21078=ORIENTED_EDGE('',*,*,#15147,.T.);
#21079=ORIENTED_EDGE('',*,*,#15148,.T.);
#21080=ORIENTED_EDGE('',*,*,#15149,.T.);
#21081=ORIENTED_EDGE('',*,*,#15150,.T.);
#21082=ORIENTED_EDGE('',*,*,#15151,.T.);
#21083=ORIENTED_EDGE('',*,*,#15152,.T.);
#21084=ORIENTED_EDGE('',*,*,#15153,.T.);
#21085=ORIENTED_EDGE('',*,*,#15154,.T.);
#21086=ORIENTED_EDGE('',*,*,#15155,.T.);
#21087=ORIENTED_EDGE('',*,*,#15156,.T.);
#21088=ORIENTED_EDGE('',*,*,#15157,.T.);
#21089=ORIENTED_EDGE('',*,*,#15158,.T.);
#21090=ORIENTED_EDGE('',*,*,#15159,.T.);
#21091=ORIENTED_EDGE('',*,*,#15160,.T.);
#21092=ORIENTED_EDGE('',*,*,#15161,.T.);
#21093=ORIENTED_EDGE('',*,*,#15162,.T.);
#21094=ORIENTED_EDGE('',*,*,#15163,.T.);
#21095=ORIENTED_EDGE('',*,*,#15164,.T.);
#21096=ORIENTED_EDGE('',*,*,#15165,.T.);
#21097=ORIENTED_EDGE('',*,*,#15166,.T.);
#21098=ORIENTED_EDGE('',*,*,#15167,.T.);
#21099=ORIENTED_EDGE('',*,*,#15168,.T.);
#21100=ORIENTED_EDGE('',*,*,#15169,.T.);
#21101=ORIENTED_EDGE('',*,*,#15170,.F.);
#21102=ORIENTED_EDGE('',*,*,#15122,.T.);
#21103=ORIENTED_EDGE('',*,*,#15097,.F.);
#21104=ORIENTED_EDGE('',*,*,#15171,.F.);
#21105=ORIENTED_EDGE('',*,*,#15095,.F.);
#21106=ORIENTED_EDGE('',*,*,#15112,.T.);
#21107=ORIENTED_EDGE('',*,*,#15172,.F.);
#21108=ORIENTED_EDGE('',*,*,#15173,.T.);
#21109=ORIENTED_EDGE('',*,*,#15174,.T.);
#21110=ORIENTED_EDGE('',*,*,#15175,.F.);
#21111=ORIENTED_EDGE('',*,*,#15107,.T.);
#21112=ORIENTED_EDGE('',*,*,#15096,.F.);
#21113=ORIENTED_EDGE('',*,*,#15173,.F.);
#21114=ORIENTED_EDGE('',*,*,#15176,.T.);
#21115=ORIENTED_EDGE('',*,*,#15177,.T.);
#21116=ORIENTED_EDGE('',*,*,#15178,.T.);
#21117=ORIENTED_EDGE('',*,*,#15179,.T.);
#21118=ORIENTED_EDGE('',*,*,#15174,.F.);
#21119=ORIENTED_EDGE('',*,*,#15180,.T.);
#21120=ORIENTED_EDGE('',*,*,#15171,.T.);
#21121=ORIENTED_EDGE('',*,*,#15100,.T.);
#21122=ORIENTED_EDGE('',*,*,#15125,.F.);
#21123=ORIENTED_EDGE('',*,*,#15181,.T.);
#21124=ORIENTED_EDGE('',*,*,#15182,.T.);
#21125=ORIENTED_EDGE('',*,*,#15183,.T.);
#21126=ORIENTED_EDGE('',*,*,#15184,.T.);
#21127=ORIENTED_EDGE('',*,*,#15185,.F.);
#21128=ORIENTED_EDGE('',*,*,#15182,.F.);
#21129=ORIENTED_EDGE('',*,*,#14597,.T.);
#21130=ORIENTED_EDGE('',*,*,#15105,.F.);
#21131=ORIENTED_EDGE('',*,*,#15103,.F.);
#21132=ORIENTED_EDGE('',*,*,#14627,.F.);
#21133=ORIENTED_EDGE('',*,*,#15101,.F.);
#21134=ORIENTED_EDGE('',*,*,#15186,.F.);
#21135=ORIENTED_EDGE('',*,*,#14662,.T.);
#21136=ORIENTED_EDGE('',*,*,#15187,.F.);
#21137=ORIENTED_EDGE('',*,*,#15113,.F.);
#21138=ORIENTED_EDGE('',*,*,#15109,.T.);
#21139=ORIENTED_EDGE('',*,*,#15108,.T.);
#21140=ORIENTED_EDGE('',*,*,#15175,.T.);
#21141=ORIENTED_EDGE('',*,*,#15179,.F.);
#21142=ORIENTED_EDGE('',*,*,#15188,.T.);
#21143=ORIENTED_EDGE('',*,*,#15116,.F.);
#21144=ORIENTED_EDGE('',*,*,#15123,.F.);
#21145=ORIENTED_EDGE('',*,*,#15189,.F.);
#21146=ORIENTED_EDGE('',*,*,#15190,.T.);
#21147=ORIENTED_EDGE('',*,*,#15191,.F.);
#21148=ORIENTED_EDGE('',*,*,#14605,.T.);
#21149=ORIENTED_EDGE('',*,*,#15192,.T.);
#21150=ORIENTED_EDGE('',*,*,#15193,.T.);
#21151=ORIENTED_EDGE('',*,*,#15191,.T.);
#21152=ORIENTED_EDGE('',*,*,#15194,.T.);
#21153=ORIENTED_EDGE('',*,*,#15195,.F.);
#21154=ORIENTED_EDGE('',*,*,#14666,.T.);
#21155=ORIENTED_EDGE('',*,*,#15196,.F.);
#21156=ORIENTED_EDGE('',*,*,#15197,.F.);
#21157=ORIENTED_EDGE('',*,*,#15198,.F.);
#21158=ORIENTED_EDGE('',*,*,#15199,.T.);
#21159=ORIENTED_EDGE('',*,*,#15197,.T.);
#21160=ORIENTED_EDGE('',*,*,#15200,.T.);
#21161=ORIENTED_EDGE('',*,*,#15201,.T.);
#21162=ORIENTED_EDGE('',*,*,#15202,.F.);
#21163=ORIENTED_EDGE('',*,*,#15111,.F.);
#21164=ORIENTED_EDGE('',*,*,#15115,.T.);
#21165=ORIENTED_EDGE('',*,*,#15203,.T.);
#21166=ORIENTED_EDGE('',*,*,#15198,.T.);
#21167=ORIENTED_EDGE('',*,*,#14611,.T.);
#21168=ORIENTED_EDGE('',*,*,#15204,.F.);
#21169=ORIENTED_EDGE('',*,*,#15192,.F.);
#21170=ORIENTED_EDGE('',*,*,#15205,.F.);
#21171=ORIENTED_EDGE('',*,*,#15206,.F.);
#21172=ORIENTED_EDGE('',*,*,#15207,.F.);
#21173=ORIENTED_EDGE('',*,*,#15183,.F.);
#21174=ORIENTED_EDGE('',*,*,#15181,.F.);
#21175=ORIENTED_EDGE('',*,*,#15124,.T.);
#21176=ORIENTED_EDGE('',*,*,#15120,.T.);
#21177=ORIENTED_EDGE('',*,*,#15118,.F.);
#21178=ORIENTED_EDGE('',*,*,#15208,.F.);
#21179=ORIENTED_EDGE('',*,*,#14656,.F.);
#21180=ORIENTED_EDGE('',*,*,#15209,.T.);
#21181=ORIENTED_EDGE('',*,*,#15210,.F.);
#21182=ORIENTED_EDGE('',*,*,#15126,.F.);
#21183=ORIENTED_EDGE('',*,*,#15211,.T.);
#21184=ORIENTED_EDGE('',*,*,#15212,.T.);
#21185=ORIENTED_EDGE('',*,*,#15213,.F.);
#21186=ORIENTED_EDGE('',*,*,#15127,.F.);
#21187=ORIENTED_EDGE('',*,*,#15210,.T.);
#21188=ORIENTED_EDGE('',*,*,#15214,.T.);
#21189=ORIENTED_EDGE('',*,*,#15215,.F.);
#21190=ORIENTED_EDGE('',*,*,#15128,.F.);
#21191=ORIENTED_EDGE('',*,*,#15213,.T.);
#21192=ORIENTED_EDGE('',*,*,#15216,.T.);
#21193=ORIENTED_EDGE('',*,*,#15217,.F.);
#21194=ORIENTED_EDGE('',*,*,#15129,.F.);
#21195=ORIENTED_EDGE('',*,*,#15215,.T.);
#21196=ORIENTED_EDGE('',*,*,#15218,.T.);
#21197=ORIENTED_EDGE('',*,*,#15219,.F.);
#21198=ORIENTED_EDGE('',*,*,#15130,.F.);
#21199=ORIENTED_EDGE('',*,*,#15217,.T.);
#21200=ORIENTED_EDGE('',*,*,#15220,.T.);
#21201=ORIENTED_EDGE('',*,*,#15221,.F.);
#21202=ORIENTED_EDGE('',*,*,#15131,.F.);
#21203=ORIENTED_EDGE('',*,*,#15219,.T.);
#21204=ORIENTED_EDGE('',*,*,#15222,.T.);
#21205=ORIENTED_EDGE('',*,*,#15223,.F.);
#21206=ORIENTED_EDGE('',*,*,#15132,.F.);
#21207=ORIENTED_EDGE('',*,*,#15221,.T.);
#21208=ORIENTED_EDGE('',*,*,#15224,.T.);
#21209=ORIENTED_EDGE('',*,*,#15225,.F.);
#21210=ORIENTED_EDGE('',*,*,#15133,.F.);
#21211=ORIENTED_EDGE('',*,*,#15223,.T.);
#21212=ORIENTED_EDGE('',*,*,#15226,.T.);
#21213=ORIENTED_EDGE('',*,*,#15227,.F.);
#21214=ORIENTED_EDGE('',*,*,#15134,.F.);
#21215=ORIENTED_EDGE('',*,*,#15225,.T.);
#21216=ORIENTED_EDGE('',*,*,#15228,.T.);
#21217=ORIENTED_EDGE('',*,*,#15229,.F.);
#21218=ORIENTED_EDGE('',*,*,#15135,.F.);
#21219=ORIENTED_EDGE('',*,*,#15227,.T.);
#21220=ORIENTED_EDGE('',*,*,#15230,.T.);
#21221=ORIENTED_EDGE('',*,*,#15231,.F.);
#21222=ORIENTED_EDGE('',*,*,#15136,.F.);
#21223=ORIENTED_EDGE('',*,*,#15229,.T.);
#21224=ORIENTED_EDGE('',*,*,#15232,.T.);
#21225=ORIENTED_EDGE('',*,*,#15233,.F.);
#21226=ORIENTED_EDGE('',*,*,#15137,.F.);
#21227=ORIENTED_EDGE('',*,*,#15231,.T.);
#21228=ORIENTED_EDGE('',*,*,#15234,.T.);
#21229=ORIENTED_EDGE('',*,*,#15235,.F.);
#21230=ORIENTED_EDGE('',*,*,#15138,.F.);
#21231=ORIENTED_EDGE('',*,*,#15233,.T.);
#21232=ORIENTED_EDGE('',*,*,#15236,.T.);
#21233=ORIENTED_EDGE('',*,*,#15237,.F.);
#21234=ORIENTED_EDGE('',*,*,#15139,.F.);
#21235=ORIENTED_EDGE('',*,*,#15235,.T.);
#21236=ORIENTED_EDGE('',*,*,#15238,.T.);
#21237=ORIENTED_EDGE('',*,*,#15239,.F.);
#21238=ORIENTED_EDGE('',*,*,#15140,.F.);
#21239=ORIENTED_EDGE('',*,*,#15237,.T.);
#21240=ORIENTED_EDGE('',*,*,#15240,.T.);
#21241=ORIENTED_EDGE('',*,*,#15241,.F.);
#21242=ORIENTED_EDGE('',*,*,#15141,.F.);
#21243=ORIENTED_EDGE('',*,*,#15239,.T.);
#21244=ORIENTED_EDGE('',*,*,#15242,.T.);
#21245=ORIENTED_EDGE('',*,*,#15243,.F.);
#21246=ORIENTED_EDGE('',*,*,#15142,.F.);
#21247=ORIENTED_EDGE('',*,*,#15241,.T.);
#21248=ORIENTED_EDGE('',*,*,#15244,.T.);
#21249=ORIENTED_EDGE('',*,*,#15245,.F.);
#21250=ORIENTED_EDGE('',*,*,#15143,.F.);
#21251=ORIENTED_EDGE('',*,*,#15243,.T.);
#21252=ORIENTED_EDGE('',*,*,#15246,.T.);
#21253=ORIENTED_EDGE('',*,*,#15247,.F.);
#21254=ORIENTED_EDGE('',*,*,#15144,.F.);
#21255=ORIENTED_EDGE('',*,*,#15245,.T.);
#21256=ORIENTED_EDGE('',*,*,#15248,.T.);
#21257=ORIENTED_EDGE('',*,*,#15249,.F.);
#21258=ORIENTED_EDGE('',*,*,#15145,.F.);
#21259=ORIENTED_EDGE('',*,*,#15247,.T.);
#21260=ORIENTED_EDGE('',*,*,#15250,.T.);
#21261=ORIENTED_EDGE('',*,*,#15251,.F.);
#21262=ORIENTED_EDGE('',*,*,#15146,.F.);
#21263=ORIENTED_EDGE('',*,*,#15249,.T.);
#21264=ORIENTED_EDGE('',*,*,#15252,.T.);
#21265=ORIENTED_EDGE('',*,*,#15253,.F.);
#21266=ORIENTED_EDGE('',*,*,#15147,.F.);
#21267=ORIENTED_EDGE('',*,*,#15251,.T.);
#21268=ORIENTED_EDGE('',*,*,#15254,.T.);
#21269=ORIENTED_EDGE('',*,*,#15255,.F.);
#21270=ORIENTED_EDGE('',*,*,#15148,.F.);
#21271=ORIENTED_EDGE('',*,*,#15253,.T.);
#21272=ORIENTED_EDGE('',*,*,#15256,.T.);
#21273=ORIENTED_EDGE('',*,*,#15257,.F.);
#21274=ORIENTED_EDGE('',*,*,#15149,.F.);
#21275=ORIENTED_EDGE('',*,*,#15255,.T.);
#21276=ORIENTED_EDGE('',*,*,#15258,.T.);
#21277=ORIENTED_EDGE('',*,*,#15259,.F.);
#21278=ORIENTED_EDGE('',*,*,#15150,.F.);
#21279=ORIENTED_EDGE('',*,*,#15257,.T.);
#21280=ORIENTED_EDGE('',*,*,#15260,.T.);
#21281=ORIENTED_EDGE('',*,*,#15261,.F.);
#21282=ORIENTED_EDGE('',*,*,#15151,.F.);
#21283=ORIENTED_EDGE('',*,*,#15259,.T.);
#21284=ORIENTED_EDGE('',*,*,#15262,.T.);
#21285=ORIENTED_EDGE('',*,*,#15263,.F.);
#21286=ORIENTED_EDGE('',*,*,#15152,.F.);
#21287=ORIENTED_EDGE('',*,*,#15261,.T.);
#21288=ORIENTED_EDGE('',*,*,#15264,.T.);
#21289=ORIENTED_EDGE('',*,*,#15265,.F.);
#21290=ORIENTED_EDGE('',*,*,#15153,.F.);
#21291=ORIENTED_EDGE('',*,*,#15263,.T.);
#21292=ORIENTED_EDGE('',*,*,#15266,.T.);
#21293=ORIENTED_EDGE('',*,*,#15267,.F.);
#21294=ORIENTED_EDGE('',*,*,#15154,.F.);
#21295=ORIENTED_EDGE('',*,*,#15265,.T.);
#21296=ORIENTED_EDGE('',*,*,#15268,.T.);
#21297=ORIENTED_EDGE('',*,*,#15269,.F.);
#21298=ORIENTED_EDGE('',*,*,#15155,.F.);
#21299=ORIENTED_EDGE('',*,*,#15267,.T.);
#21300=ORIENTED_EDGE('',*,*,#15270,.T.);
#21301=ORIENTED_EDGE('',*,*,#15271,.F.);
#21302=ORIENTED_EDGE('',*,*,#15156,.F.);
#21303=ORIENTED_EDGE('',*,*,#15269,.T.);
#21304=ORIENTED_EDGE('',*,*,#15272,.T.);
#21305=ORIENTED_EDGE('',*,*,#15273,.F.);
#21306=ORIENTED_EDGE('',*,*,#15157,.F.);
#21307=ORIENTED_EDGE('',*,*,#15271,.T.);
#21308=ORIENTED_EDGE('',*,*,#15274,.T.);
#21309=ORIENTED_EDGE('',*,*,#15275,.F.);
#21310=ORIENTED_EDGE('',*,*,#15158,.F.);
#21311=ORIENTED_EDGE('',*,*,#15273,.T.);
#21312=ORIENTED_EDGE('',*,*,#15276,.T.);
#21313=ORIENTED_EDGE('',*,*,#15277,.F.);
#21314=ORIENTED_EDGE('',*,*,#15159,.F.);
#21315=ORIENTED_EDGE('',*,*,#15275,.T.);
#21316=ORIENTED_EDGE('',*,*,#15278,.T.);
#21317=ORIENTED_EDGE('',*,*,#15279,.F.);
#21318=ORIENTED_EDGE('',*,*,#15160,.F.);
#21319=ORIENTED_EDGE('',*,*,#15277,.T.);
#21320=ORIENTED_EDGE('',*,*,#15280,.T.);
#21321=ORIENTED_EDGE('',*,*,#15281,.F.);
#21322=ORIENTED_EDGE('',*,*,#15161,.F.);
#21323=ORIENTED_EDGE('',*,*,#15279,.T.);
#21324=ORIENTED_EDGE('',*,*,#15282,.T.);
#21325=ORIENTED_EDGE('',*,*,#15283,.F.);
#21326=ORIENTED_EDGE('',*,*,#15162,.F.);
#21327=ORIENTED_EDGE('',*,*,#15281,.T.);
#21328=ORIENTED_EDGE('',*,*,#15284,.T.);
#21329=ORIENTED_EDGE('',*,*,#15285,.F.);
#21330=ORIENTED_EDGE('',*,*,#15163,.F.);
#21331=ORIENTED_EDGE('',*,*,#15283,.T.);
#21332=ORIENTED_EDGE('',*,*,#15286,.T.);
#21333=ORIENTED_EDGE('',*,*,#15287,.F.);
#21334=ORIENTED_EDGE('',*,*,#15164,.F.);
#21335=ORIENTED_EDGE('',*,*,#15285,.T.);
#21336=ORIENTED_EDGE('',*,*,#15288,.T.);
#21337=ORIENTED_EDGE('',*,*,#15289,.F.);
#21338=ORIENTED_EDGE('',*,*,#15165,.F.);
#21339=ORIENTED_EDGE('',*,*,#15287,.T.);
#21340=ORIENTED_EDGE('',*,*,#15290,.T.);
#21341=ORIENTED_EDGE('',*,*,#15291,.F.);
#21342=ORIENTED_EDGE('',*,*,#15166,.F.);
#21343=ORIENTED_EDGE('',*,*,#15289,.T.);
#21344=ORIENTED_EDGE('',*,*,#15292,.T.);
#21345=ORIENTED_EDGE('',*,*,#15293,.F.);
#21346=ORIENTED_EDGE('',*,*,#15167,.F.);
#21347=ORIENTED_EDGE('',*,*,#15291,.T.);
#21348=ORIENTED_EDGE('',*,*,#15294,.T.);
#21349=ORIENTED_EDGE('',*,*,#15295,.F.);
#21350=ORIENTED_EDGE('',*,*,#15168,.F.);
#21351=ORIENTED_EDGE('',*,*,#15293,.T.);
#21352=ORIENTED_EDGE('',*,*,#15296,.T.);
#21353=ORIENTED_EDGE('',*,*,#15211,.F.);
#21354=ORIENTED_EDGE('',*,*,#15169,.F.);
#21355=ORIENTED_EDGE('',*,*,#15295,.T.);
#21356=ORIENTED_EDGE('',*,*,#15297,.T.);
#21357=ORIENTED_EDGE('',*,*,#15298,.T.);
#21358=ORIENTED_EDGE('',*,*,#15299,.T.);
#21359=ORIENTED_EDGE('',*,*,#15300,.T.);
#21360=ORIENTED_EDGE('',*,*,#14622,.F.);
#21361=ORIENTED_EDGE('',*,*,#15301,.F.);
#21362=ORIENTED_EDGE('',*,*,#15302,.T.);
#21363=ORIENTED_EDGE('',*,*,#15303,.F.);
#21364=ORIENTED_EDGE('',*,*,#15298,.F.);
#21365=ORIENTED_EDGE('',*,*,#15304,.F.);
#21366=ORIENTED_EDGE('',*,*,#15305,.F.);
#21367=ORIENTED_EDGE('',*,*,#15306,.F.);
#21368=ORIENTED_EDGE('',*,*,#15302,.F.);
#21369=ORIENTED_EDGE('',*,*,#15307,.F.);
#21370=ORIENTED_EDGE('',*,*,#15308,.F.);
#21371=ORIENTED_EDGE('',*,*,#15309,.F.);
#21372=ORIENTED_EDGE('',*,*,#15305,.T.);
#21373=ORIENTED_EDGE('',*,*,#15310,.F.);
#21374=ORIENTED_EDGE('',*,*,#15311,.F.);
#21375=ORIENTED_EDGE('',*,*,#15312,.F.);
#21376=ORIENTED_EDGE('',*,*,#15308,.T.);
#21377=ORIENTED_EDGE('',*,*,#14619,.F.);
#21378=ORIENTED_EDGE('',*,*,#15313,.F.);
#21379=ORIENTED_EDGE('',*,*,#15314,.F.);
#21380=ORIENTED_EDGE('',*,*,#15315,.F.);
#21381=ORIENTED_EDGE('',*,*,#15316,.T.);
#21382=ORIENTED_EDGE('',*,*,#14616,.F.);
#21383=ORIENTED_EDGE('',*,*,#15317,.F.);
#21384=ORIENTED_EDGE('',*,*,#15318,.F.);
#21385=ORIENTED_EDGE('',*,*,#15319,.F.);
#21386=ORIENTED_EDGE('',*,*,#15314,.T.);
#21387=ORIENTED_EDGE('',*,*,#15320,.F.);
#21388=ORIENTED_EDGE('',*,*,#15321,.F.);
#21389=ORIENTED_EDGE('',*,*,#15322,.F.);
#21390=ORIENTED_EDGE('',*,*,#15318,.T.);
#21391=ORIENTED_EDGE('',*,*,#15323,.F.);
#21392=ORIENTED_EDGE('',*,*,#15321,.T.);
#21393=ORIENTED_EDGE('',*,*,#15324,.F.);
#21394=ORIENTED_EDGE('',*,*,#15300,.F.);
#21395=ORIENTED_EDGE('',*,*,#15325,.F.);
#21396=ORIENTED_EDGE('',*,*,#15189,.T.);
#21397=ORIENTED_EDGE('',*,*,#15170,.T.);
#21398=ORIENTED_EDGE('',*,*,#15326,.T.);
#21399=ORIENTED_EDGE('',*,*,#15327,.T.);
#21400=ORIENTED_EDGE('',*,*,#15328,.T.);
#21401=ORIENTED_EDGE('',*,*,#15328,.F.);
#21402=ORIENTED_EDGE('',*,*,#15329,.T.);
#21403=ORIENTED_EDGE('',*,*,#15330,.T.);
#21404=ORIENTED_EDGE('',*,*,#15331,.F.);
#21405=ORIENTED_EDGE('',*,*,#15332,.T.);
#21406=ORIENTED_EDGE('',*,*,#15333,.F.);
#21407=ORIENTED_EDGE('',*,*,#15330,.F.);
#21408=ORIENTED_EDGE('',*,*,#15334,.T.);
#21409=ORIENTED_EDGE('',*,*,#14604,.F.);
#21410=ORIENTED_EDGE('',*,*,#14607,.F.);
#21411=ORIENTED_EDGE('',*,*,#15335,.T.);
#21412=ORIENTED_EDGE('',*,*,#15336,.T.);
#21413=ORIENTED_EDGE('',*,*,#15332,.F.);
#21414=ORIENTED_EDGE('',*,*,#15337,.F.);
#21415=ORIENTED_EDGE('',*,*,#15338,.T.);
#21416=ORIENTED_EDGE('',*,*,#15339,.T.);
#21417=ORIENTED_EDGE('',*,*,#15335,.F.);
#21418=ORIENTED_EDGE('',*,*,#15340,.F.);
#21419=ORIENTED_EDGE('',*,*,#15341,.T.);
#21420=ORIENTED_EDGE('',*,*,#15342,.T.);
#21421=ORIENTED_EDGE('',*,*,#15338,.F.);
#21422=ORIENTED_EDGE('',*,*,#15343,.F.);
#21423=ORIENTED_EDGE('',*,*,#15341,.F.);
#21424=ORIENTED_EDGE('',*,*,#15344,.T.);
#21425=ORIENTED_EDGE('',*,*,#15345,.T.);
#21426=ORIENTED_EDGE('',*,*,#15346,.F.);
#21427=ORIENTED_EDGE('',*,*,#15347,.T.);
#21428=ORIENTED_EDGE('',*,*,#15348,.T.);
#21429=ORIENTED_EDGE('',*,*,#15345,.F.);
#21430=ORIENTED_EDGE('',*,*,#15349,.F.);
#21431=ORIENTED_EDGE('',*,*,#15350,.T.);
#21432=ORIENTED_EDGE('',*,*,#15351,.T.);
#21433=ORIENTED_EDGE('',*,*,#15347,.F.);
#21434=ORIENTED_EDGE('',*,*,#15352,.F.);
#21435=ORIENTED_EDGE('',*,*,#15353,.T.);
#21436=ORIENTED_EDGE('',*,*,#15354,.T.);
#21437=ORIENTED_EDGE('',*,*,#15350,.F.);
#21438=ORIENTED_EDGE('',*,*,#15355,.F.);
#21439=ORIENTED_EDGE('',*,*,#15353,.F.);
#21440=ORIENTED_EDGE('',*,*,#15356,.T.);
#21441=ORIENTED_EDGE('',*,*,#15357,.T.);
#21442=ORIENTED_EDGE('',*,*,#15358,.F.);
#21443=ORIENTED_EDGE('',*,*,#14610,.F.);
#21444=ORIENTED_EDGE('',*,*,#14613,.F.);
#21445=ORIENTED_EDGE('',*,*,#15357,.F.);
#21446=ORIENTED_EDGE('',*,*,#15359,.T.);
#21447=ORIENTED_EDGE('',*,*,#15360,.T.);
#21448=ORIENTED_EDGE('',*,*,#15361,.F.);
#21449=ORIENTED_EDGE('',*,*,#15360,.F.);
#21450=ORIENTED_EDGE('',*,*,#15362,.T.);
#21451=ORIENTED_EDGE('',*,*,#15363,.T.);
#21452=ORIENTED_EDGE('',*,*,#15364,.F.);
#21453=ORIENTED_EDGE('',*,*,#15363,.F.);
#21454=ORIENTED_EDGE('',*,*,#15365,.T.);
#21455=ORIENTED_EDGE('',*,*,#15366,.T.);
#21456=ORIENTED_EDGE('',*,*,#15367,.F.);
#21457=ORIENTED_EDGE('',*,*,#15368,.T.);
#21458=ORIENTED_EDGE('',*,*,#15369,.T.);
#21459=ORIENTED_EDGE('',*,*,#15172,.T.);
#21460=ORIENTED_EDGE('',*,*,#15202,.T.);
#21461=ORIENTED_EDGE('',*,*,#15370,.F.);
#21462=ORIENTED_EDGE('',*,*,#15366,.F.);
#21463=ORIENTED_EDGE('',*,*,#15371,.T.);
#21464=ORIENTED_EDGE('',*,*,#15177,.F.);
#21465=ORIENTED_EDGE('',*,*,#15176,.F.);
#21466=ORIENTED_EDGE('',*,*,#15369,.F.);
#21467=ORIENTED_EDGE('',*,*,#15372,.T.);
#21468=ORIENTED_EDGE('',*,*,#15373,.F.);
#21469=ORIENTED_EDGE('',*,*,#14608,.T.);
#21470=ORIENTED_EDGE('',*,*,#15374,.T.);
#21471=ORIENTED_EDGE('',*,*,#15375,.T.);
#21472=ORIENTED_EDGE('',*,*,#15373,.T.);
#21473=ORIENTED_EDGE('',*,*,#15376,.T.);
#21474=ORIENTED_EDGE('',*,*,#15377,.F.);
#21475=ORIENTED_EDGE('',*,*,#15374,.F.);
#21476=ORIENTED_EDGE('',*,*,#15378,.T.);
#21477=ORIENTED_EDGE('',*,*,#15379,.T.);
#21478=ORIENTED_EDGE('',*,*,#15380,.F.);
#21479=ORIENTED_EDGE('',*,*,#14654,.F.);
#21480=ORIENTED_EDGE('',*,*,#15381,.T.);
#21481=ORIENTED_EDGE('',*,*,#15382,.F.);
#21482=ORIENTED_EDGE('',*,*,#15383,.F.);
#21483=ORIENTED_EDGE('',*,*,#15384,.T.);
#21484=ORIENTED_EDGE('',*,*,#15382,.T.);
#21485=ORIENTED_EDGE('',*,*,#15385,.T.);
#21486=ORIENTED_EDGE('',*,*,#15386,.T.);
#21487=ORIENTED_EDGE('',*,*,#15326,.F.);
#21488=ORIENTED_EDGE('',*,*,#15180,.F.);
#21489=ORIENTED_EDGE('',*,*,#15185,.T.);
#21490=ORIENTED_EDGE('',*,*,#15387,.T.);
#21491=ORIENTED_EDGE('',*,*,#15383,.T.);
#21492=ORIENTED_EDGE('',*,*,#14602,.T.);
#21493=ORIENTED_EDGE('',*,*,#15388,.F.);
#21494=ORIENTED_EDGE('',*,*,#15379,.F.);
#21495=ORIENTED_EDGE('',*,*,#15389,.T.);
#21496=ORIENTED_EDGE('',*,*,#15390,.T.);
#21497=ORIENTED_EDGE('',*,*,#15391,.F.);
#21498=ORIENTED_EDGE('',*,*,#15316,.F.);
#21499=ORIENTED_EDGE('',*,*,#15392,.F.);
#21500=ORIENTED_EDGE('',*,*,#15393,.T.);
#21501=ORIENTED_EDGE('',*,*,#15394,.F.);
#21502=ORIENTED_EDGE('',*,*,#15395,.F.);
#21503=ORIENTED_EDGE('',*,*,#15396,.F.);
#21504=ORIENTED_EDGE('',*,*,#15311,.T.);
#21505=ORIENTED_EDGE('',*,*,#15201,.F.);
#21506=ORIENTED_EDGE('',*,*,#15200,.F.);
#21507=ORIENTED_EDGE('',*,*,#15196,.T.);
#21508=ORIENTED_EDGE('',*,*,#14665,.T.);
#21509=ORIENTED_EDGE('',*,*,#15397,.T.);
#21510=ORIENTED_EDGE('',*,*,#15392,.T.);
#21511=ORIENTED_EDGE('',*,*,#15315,.T.);
#21512=ORIENTED_EDGE('',*,*,#15319,.T.);
#21513=ORIENTED_EDGE('',*,*,#15322,.T.);
#21514=ORIENTED_EDGE('',*,*,#15323,.T.);
#21515=ORIENTED_EDGE('',*,*,#15299,.F.);
#21516=ORIENTED_EDGE('',*,*,#15303,.T.);
#21517=ORIENTED_EDGE('',*,*,#15306,.T.);
#21518=ORIENTED_EDGE('',*,*,#15309,.T.);
#21519=ORIENTED_EDGE('',*,*,#15312,.T.);
#21520=ORIENTED_EDGE('',*,*,#15396,.T.);
#21521=ORIENTED_EDGE('',*,*,#15398,.T.);
#21522=ORIENTED_EDGE('',*,*,#15399,.T.);
#21523=ORIENTED_EDGE('',*,*,#15205,.T.);
#21524=ORIENTED_EDGE('',*,*,#15194,.F.);
#21525=ORIENTED_EDGE('',*,*,#15190,.F.);
#21526=ORIENTED_EDGE('',*,*,#15325,.T.);
#21527=ORIENTED_EDGE('',*,*,#15331,.T.);
#21528=ORIENTED_EDGE('',*,*,#15333,.T.);
#21529=ORIENTED_EDGE('',*,*,#15336,.F.);
#21530=ORIENTED_EDGE('',*,*,#15339,.F.);
#21531=ORIENTED_EDGE('',*,*,#15342,.F.);
#21532=ORIENTED_EDGE('',*,*,#15346,.T.);
#21533=ORIENTED_EDGE('',*,*,#15348,.F.);
#21534=ORIENTED_EDGE('',*,*,#15351,.F.);
#21535=ORIENTED_EDGE('',*,*,#15354,.F.);
#21536=ORIENTED_EDGE('',*,*,#15358,.T.);
#21537=ORIENTED_EDGE('',*,*,#15361,.T.);
#21538=ORIENTED_EDGE('',*,*,#15364,.T.);
#21539=ORIENTED_EDGE('',*,*,#15367,.T.);
#21540=ORIENTED_EDGE('',*,*,#15370,.T.);
#21541=ORIENTED_EDGE('',*,*,#15400,.F.);
#21542=ORIENTED_EDGE('',*,*,#15206,.T.);
#21543=ORIENTED_EDGE('',*,*,#15399,.F.);
#21544=ORIENTED_EDGE('',*,*,#15401,.F.);
#21545=ORIENTED_EDGE('',*,*,#15324,.T.);
#21546=ORIENTED_EDGE('',*,*,#15320,.T.);
#21547=ORIENTED_EDGE('',*,*,#15317,.T.);
#21548=ORIENTED_EDGE('',*,*,#15313,.T.);
#21549=ORIENTED_EDGE('',*,*,#15391,.T.);
#21550=ORIENTED_EDGE('',*,*,#15402,.T.);
#21551=ORIENTED_EDGE('',*,*,#15403,.T.);
#21552=ORIENTED_EDGE('',*,*,#15404,.T.);
#21553=ORIENTED_EDGE('',*,*,#15405,.T.);
#21554=ORIENTED_EDGE('',*,*,#15406,.T.);
#21555=ORIENTED_EDGE('',*,*,#15407,.T.);
#21556=ORIENTED_EDGE('',*,*,#15408,.T.);
#21557=ORIENTED_EDGE('',*,*,#15409,.T.);
#21558=ORIENTED_EDGE('',*,*,#15410,.T.);
#21559=ORIENTED_EDGE('',*,*,#15411,.T.);
#21560=ORIENTED_EDGE('',*,*,#15412,.T.);
#21561=ORIENTED_EDGE('',*,*,#15413,.T.);
#21562=ORIENTED_EDGE('',*,*,#15414,.T.);
#21563=ORIENTED_EDGE('',*,*,#15415,.T.);
#21564=ORIENTED_EDGE('',*,*,#15416,.T.);
#21565=ORIENTED_EDGE('',*,*,#15417,.T.);
#21566=ORIENTED_EDGE('',*,*,#15418,.T.);
#21567=ORIENTED_EDGE('',*,*,#15419,.T.);
#21568=ORIENTED_EDGE('',*,*,#15420,.T.);
#21569=ORIENTED_EDGE('',*,*,#15421,.T.);
#21570=ORIENTED_EDGE('',*,*,#15422,.T.);
#21571=ORIENTED_EDGE('',*,*,#15423,.T.);
#21572=ORIENTED_EDGE('',*,*,#15424,.T.);
#21573=ORIENTED_EDGE('',*,*,#15425,.T.);
#21574=ORIENTED_EDGE('',*,*,#15426,.T.);
#21575=ORIENTED_EDGE('',*,*,#15427,.T.);
#21576=ORIENTED_EDGE('',*,*,#15428,.T.);
#21577=ORIENTED_EDGE('',*,*,#15429,.T.);
#21578=ORIENTED_EDGE('',*,*,#15430,.T.);
#21579=ORIENTED_EDGE('',*,*,#15431,.T.);
#21580=ORIENTED_EDGE('',*,*,#15432,.T.);
#21581=ORIENTED_EDGE('',*,*,#15433,.T.);
#21582=ORIENTED_EDGE('',*,*,#15434,.T.);
#21583=ORIENTED_EDGE('',*,*,#15435,.T.);
#21584=ORIENTED_EDGE('',*,*,#15436,.T.);
#21585=ORIENTED_EDGE('',*,*,#15437,.T.);
#21586=ORIENTED_EDGE('',*,*,#15438,.T.);
#21587=ORIENTED_EDGE('',*,*,#15394,.T.);
#21588=ORIENTED_EDGE('',*,*,#15310,.T.);
#21589=ORIENTED_EDGE('',*,*,#15307,.T.);
#21590=ORIENTED_EDGE('',*,*,#15304,.T.);
#21591=ORIENTED_EDGE('',*,*,#15301,.T.);
#21592=ORIENTED_EDGE('',*,*,#15297,.F.);
#21593=ORIENTED_EDGE('',*,*,#15296,.F.);
#21594=ORIENTED_EDGE('',*,*,#15294,.F.);
#21595=ORIENTED_EDGE('',*,*,#15292,.F.);
#21596=ORIENTED_EDGE('',*,*,#15290,.F.);
#21597=ORIENTED_EDGE('',*,*,#15288,.F.);
#21598=ORIENTED_EDGE('',*,*,#15286,.F.);
#21599=ORIENTED_EDGE('',*,*,#15284,.F.);
#21600=ORIENTED_EDGE('',*,*,#15282,.F.);
#21601=ORIENTED_EDGE('',*,*,#15280,.F.);
#21602=ORIENTED_EDGE('',*,*,#15278,.F.);
#21603=ORIENTED_EDGE('',*,*,#15276,.F.);
#21604=ORIENTED_EDGE('',*,*,#15274,.F.);
#21605=ORIENTED_EDGE('',*,*,#15272,.F.);
#21606=ORIENTED_EDGE('',*,*,#15270,.F.);
#21607=ORIENTED_EDGE('',*,*,#15268,.F.);
#21608=ORIENTED_EDGE('',*,*,#15266,.F.);
#21609=ORIENTED_EDGE('',*,*,#15264,.F.);
#21610=ORIENTED_EDGE('',*,*,#15262,.F.);
#21611=ORIENTED_EDGE('',*,*,#15260,.F.);
#21612=ORIENTED_EDGE('',*,*,#15258,.F.);
#21613=ORIENTED_EDGE('',*,*,#15256,.F.);
#21614=ORIENTED_EDGE('',*,*,#15254,.F.);
#21615=ORIENTED_EDGE('',*,*,#15252,.F.);
#21616=ORIENTED_EDGE('',*,*,#15250,.F.);
#21617=ORIENTED_EDGE('',*,*,#15248,.F.);
#21618=ORIENTED_EDGE('',*,*,#15246,.F.);
#21619=ORIENTED_EDGE('',*,*,#15244,.F.);
#21620=ORIENTED_EDGE('',*,*,#15242,.F.);
#21621=ORIENTED_EDGE('',*,*,#15240,.F.);
#21622=ORIENTED_EDGE('',*,*,#15238,.F.);
#21623=ORIENTED_EDGE('',*,*,#15236,.F.);
#21624=ORIENTED_EDGE('',*,*,#15234,.F.);
#21625=ORIENTED_EDGE('',*,*,#15232,.F.);
#21626=ORIENTED_EDGE('',*,*,#15230,.F.);
#21627=ORIENTED_EDGE('',*,*,#15228,.F.);
#21628=ORIENTED_EDGE('',*,*,#15226,.F.);
#21629=ORIENTED_EDGE('',*,*,#15224,.F.);
#21630=ORIENTED_EDGE('',*,*,#15222,.F.);
#21631=ORIENTED_EDGE('',*,*,#15220,.F.);
#21632=ORIENTED_EDGE('',*,*,#15218,.F.);
#21633=ORIENTED_EDGE('',*,*,#15216,.F.);
#21634=ORIENTED_EDGE('',*,*,#15214,.F.);
#21635=ORIENTED_EDGE('',*,*,#15212,.F.);
#21636=ORIENTED_EDGE('',*,*,#15209,.F.);
#21637=ORIENTED_EDGE('',*,*,#15386,.F.);
#21638=ORIENTED_EDGE('',*,*,#15385,.F.);
#21639=ORIENTED_EDGE('',*,*,#15381,.F.);
#21640=ORIENTED_EDGE('',*,*,#14653,.F.);
#21641=ORIENTED_EDGE('',*,*,#15439,.F.);
#21642=ORIENTED_EDGE('',*,*,#15440,.F.);
#21643=ORIENTED_EDGE('',*,*,#15441,.F.);
#21644=ORIENTED_EDGE('',*,*,#15442,.F.);
#21645=ORIENTED_EDGE('',*,*,#15443,.F.);
#21646=ORIENTED_EDGE('',*,*,#15444,.T.);
#21647=ORIENTED_EDGE('',*,*,#15445,.F.);
#21648=ORIENTED_EDGE('',*,*,#15446,.T.);
#21649=ORIENTED_EDGE('',*,*,#15447,.F.);
#21650=ORIENTED_EDGE('',*,*,#15448,.F.);
#21651=ORIENTED_EDGE('',*,*,#15449,.F.);
#21652=ORIENTED_EDGE('',*,*,#15450,.F.);
#21653=ORIENTED_EDGE('',*,*,#15451,.F.);
#21654=ORIENTED_EDGE('',*,*,#15389,.F.);
#21655=ORIENTED_EDGE('',*,*,#15378,.F.);
#21656=ORIENTED_EDGE('',*,*,#15376,.F.);
#21657=ORIENTED_EDGE('',*,*,#15372,.F.);
#21658=ORIENTED_EDGE('',*,*,#15368,.F.);
#21659=ORIENTED_EDGE('',*,*,#15365,.F.);
#21660=ORIENTED_EDGE('',*,*,#15362,.F.);
#21661=ORIENTED_EDGE('',*,*,#15359,.F.);
#21662=ORIENTED_EDGE('',*,*,#15356,.F.);
#21663=ORIENTED_EDGE('',*,*,#15355,.T.);
#21664=ORIENTED_EDGE('',*,*,#15352,.T.);
#21665=ORIENTED_EDGE('',*,*,#15349,.T.);
#21666=ORIENTED_EDGE('',*,*,#15344,.F.);
#21667=ORIENTED_EDGE('',*,*,#15343,.T.);
#21668=ORIENTED_EDGE('',*,*,#15340,.T.);
#21669=ORIENTED_EDGE('',*,*,#15337,.T.);
#21670=ORIENTED_EDGE('',*,*,#15334,.F.);
#21671=ORIENTED_EDGE('',*,*,#15329,.F.);
#21672=ORIENTED_EDGE('',*,*,#15327,.F.);
#21673=ORIENTED_EDGE('',*,*,#15452,.F.);
#21674=ORIENTED_EDGE('',*,*,#15453,.T.);
#21675=ORIENTED_EDGE('',*,*,#15446,.F.);
#21676=ORIENTED_EDGE('',*,*,#15454,.F.);
#21677=ORIENTED_EDGE('',*,*,#15455,.T.);
#21678=ORIENTED_EDGE('',*,*,#15456,.T.);
#21679=ORIENTED_EDGE('',*,*,#15442,.T.);
#21680=ORIENTED_EDGE('',*,*,#15457,.F.);
#21681=ORIENTED_EDGE('',*,*,#15458,.T.);
#21682=ORIENTED_EDGE('',*,*,#15457,.T.);
#21683=ORIENTED_EDGE('',*,*,#15441,.T.);
#21684=ORIENTED_EDGE('',*,*,#15459,.F.);
#21685=ORIENTED_EDGE('',*,*,#14593,.F.);
#21686=ORIENTED_EDGE('',*,*,#15460,.T.);
#21687=ORIENTED_EDGE('',*,*,#15459,.T.);
#21688=ORIENTED_EDGE('',*,*,#15440,.T.);
#21689=ORIENTED_EDGE('',*,*,#15461,.F.);
#21690=ORIENTED_EDGE('',*,*,#15462,.T.);
#21691=ORIENTED_EDGE('',*,*,#15463,.F.);
#21692=ORIENTED_EDGE('',*,*,#15443,.T.);
#21693=ORIENTED_EDGE('',*,*,#15456,.F.);
#21694=ORIENTED_EDGE('',*,*,#15464,.F.);
#21695=ORIENTED_EDGE('',*,*,#15465,.T.);
#21696=ORIENTED_EDGE('',*,*,#15466,.F.);
#21697=ORIENTED_EDGE('',*,*,#15436,.F.);
#21698=ORIENTED_EDGE('',*,*,#15467,.F.);
#21699=ORIENTED_EDGE('',*,*,#15468,.T.);
#21700=ORIENTED_EDGE('',*,*,#15469,.F.);
#21701=ORIENTED_EDGE('',*,*,#15434,.F.);
#21702=ORIENTED_EDGE('',*,*,#15469,.T.);
#21703=ORIENTED_EDGE('',*,*,#15470,.T.);
#21704=ORIENTED_EDGE('',*,*,#15464,.T.);
#21705=ORIENTED_EDGE('',*,*,#15435,.F.);
#21706=ORIENTED_EDGE('',*,*,#15466,.T.);
#21707=ORIENTED_EDGE('',*,*,#15471,.T.);
#21708=ORIENTED_EDGE('',*,*,#15472,.T.);
#21709=ORIENTED_EDGE('',*,*,#15437,.F.);
#21710=ORIENTED_EDGE('',*,*,#15472,.F.);
#21711=ORIENTED_EDGE('',*,*,#15473,.T.);
#21712=ORIENTED_EDGE('',*,*,#15461,.T.);
#21713=ORIENTED_EDGE('',*,*,#15439,.T.);
#21714=ORIENTED_EDGE('',*,*,#14652,.T.);
#21715=ORIENTED_EDGE('',*,*,#14658,.T.);
#21716=ORIENTED_EDGE('',*,*,#15401,.T.);
#21717=ORIENTED_EDGE('',*,*,#15398,.F.);
#21718=ORIENTED_EDGE('',*,*,#15395,.T.);
#21719=ORIENTED_EDGE('',*,*,#15438,.F.);
#21720=ORIENTED_EDGE('',*,*,#15474,.T.);
#21721=ORIENTED_EDGE('',*,*,#15475,.F.);
#21722=ORIENTED_EDGE('',*,*,#15432,.F.);
#21723=ORIENTED_EDGE('',*,*,#15476,.F.);
#21724=ORIENTED_EDGE('',*,*,#15477,.T.);
#21725=ORIENTED_EDGE('',*,*,#15478,.F.);
#21726=ORIENTED_EDGE('',*,*,#15430,.F.);
#21727=ORIENTED_EDGE('',*,*,#15479,.F.);
#21728=ORIENTED_EDGE('',*,*,#15478,.T.);
#21729=ORIENTED_EDGE('',*,*,#15480,.T.);
#21730=ORIENTED_EDGE('',*,*,#15476,.T.);
#21731=ORIENTED_EDGE('',*,*,#15431,.F.);
#21732=ORIENTED_EDGE('',*,*,#15481,.T.);
#21733=ORIENTED_EDGE('',*,*,#15482,.F.);
#21734=ORIENTED_EDGE('',*,*,#15428,.F.);
#21735=ORIENTED_EDGE('',*,*,#15483,.F.);
#21736=ORIENTED_EDGE('',*,*,#15484,.T.);
#21737=ORIENTED_EDGE('',*,*,#15485,.F.);
#21738=ORIENTED_EDGE('',*,*,#15426,.F.);
#21739=ORIENTED_EDGE('',*,*,#15486,.F.);
#21740=ORIENTED_EDGE('',*,*,#15485,.T.);
#21741=ORIENTED_EDGE('',*,*,#15487,.T.);
#21742=ORIENTED_EDGE('',*,*,#15483,.T.);
#21743=ORIENTED_EDGE('',*,*,#15427,.F.);
#21744=ORIENTED_EDGE('',*,*,#15482,.T.);
#21745=ORIENTED_EDGE('',*,*,#15488,.T.);
#21746=ORIENTED_EDGE('',*,*,#15479,.T.);
#21747=ORIENTED_EDGE('',*,*,#15429,.F.);
#21748=ORIENTED_EDGE('',*,*,#15489,.T.);
#21749=ORIENTED_EDGE('',*,*,#15490,.F.);
#21750=ORIENTED_EDGE('',*,*,#15424,.F.);
#21751=ORIENTED_EDGE('',*,*,#15491,.F.);
#21752=ORIENTED_EDGE('',*,*,#15492,.T.);
#21753=ORIENTED_EDGE('',*,*,#15493,.F.);
#21754=ORIENTED_EDGE('',*,*,#15422,.F.);
#21755=ORIENTED_EDGE('',*,*,#15494,.F.);
#21756=ORIENTED_EDGE('',*,*,#15493,.T.);
#21757=ORIENTED_EDGE('',*,*,#15495,.T.);
#21758=ORIENTED_EDGE('',*,*,#15491,.T.);
#21759=ORIENTED_EDGE('',*,*,#15423,.F.);
#21760=ORIENTED_EDGE('',*,*,#15496,.F.);
#21761=ORIENTED_EDGE('',*,*,#15497,.T.);
#21762=ORIENTED_EDGE('',*,*,#15498,.T.);
#21763=ORIENTED_EDGE('',*,*,#15420,.F.);
#21764=ORIENTED_EDGE('',*,*,#15498,.F.);
#21765=ORIENTED_EDGE('',*,*,#15499,.T.);
#21766=ORIENTED_EDGE('',*,*,#15494,.T.);
#21767=ORIENTED_EDGE('',*,*,#15421,.F.);
#21768=ORIENTED_EDGE('',*,*,#15500,.T.);
#21769=ORIENTED_EDGE('',*,*,#15501,.F.);
#21770=ORIENTED_EDGE('',*,*,#15418,.F.);
#21771=ORIENTED_EDGE('',*,*,#15502,.F.);
#21772=ORIENTED_EDGE('',*,*,#15503,.T.);
#21773=ORIENTED_EDGE('',*,*,#15504,.F.);
#21774=ORIENTED_EDGE('',*,*,#15416,.F.);
#21775=ORIENTED_EDGE('',*,*,#15505,.F.);
#21776=ORIENTED_EDGE('',*,*,#15504,.T.);
#21777=ORIENTED_EDGE('',*,*,#15506,.T.);
#21778=ORIENTED_EDGE('',*,*,#15502,.T.);
#21779=ORIENTED_EDGE('',*,*,#15417,.F.);
#21780=ORIENTED_EDGE('',*,*,#15507,.T.);
#21781=ORIENTED_EDGE('',*,*,#15508,.F.);
#21782=ORIENTED_EDGE('',*,*,#15414,.F.);
#21783=ORIENTED_EDGE('',*,*,#15509,.F.);
#21784=ORIENTED_EDGE('',*,*,#15510,.T.);
#21785=ORIENTED_EDGE('',*,*,#15511,.F.);
#21786=ORIENTED_EDGE('',*,*,#15412,.F.);
#21787=ORIENTED_EDGE('',*,*,#15512,.F.);
#21788=ORIENTED_EDGE('',*,*,#15511,.T.);
#21789=ORIENTED_EDGE('',*,*,#15513,.T.);
#21790=ORIENTED_EDGE('',*,*,#15509,.T.);
#21791=ORIENTED_EDGE('',*,*,#15413,.F.);
#21792=ORIENTED_EDGE('',*,*,#15508,.T.);
#21793=ORIENTED_EDGE('',*,*,#15514,.T.);
#21794=ORIENTED_EDGE('',*,*,#15505,.T.);
#21795=ORIENTED_EDGE('',*,*,#15415,.F.);
#21796=ORIENTED_EDGE('',*,*,#15501,.T.);
#21797=ORIENTED_EDGE('',*,*,#15515,.T.);
#21798=ORIENTED_EDGE('',*,*,#15496,.T.);
#21799=ORIENTED_EDGE('',*,*,#15419,.F.);
#21800=ORIENTED_EDGE('',*,*,#15516,.T.);
#21801=ORIENTED_EDGE('',*,*,#15517,.F.);
#21802=ORIENTED_EDGE('',*,*,#15410,.F.);
#21803=ORIENTED_EDGE('',*,*,#15518,.F.);
#21804=ORIENTED_EDGE('',*,*,#15519,.T.);
#21805=ORIENTED_EDGE('',*,*,#15520,.F.);
#21806=ORIENTED_EDGE('',*,*,#15408,.F.);
#21807=ORIENTED_EDGE('',*,*,#15521,.F.);
#21808=ORIENTED_EDGE('',*,*,#15520,.T.);
#21809=ORIENTED_EDGE('',*,*,#15522,.T.);
#21810=ORIENTED_EDGE('',*,*,#15518,.T.);
#21811=ORIENTED_EDGE('',*,*,#15409,.F.);
#21812=ORIENTED_EDGE('',*,*,#15523,.F.);
#21813=ORIENTED_EDGE('',*,*,#15524,.T.);
#21814=ORIENTED_EDGE('',*,*,#15525,.F.);
#21815=ORIENTED_EDGE('',*,*,#15406,.F.);
#21816=ORIENTED_EDGE('',*,*,#15526,.F.);
#21817=ORIENTED_EDGE('',*,*,#15527,.T.);
#21818=ORIENTED_EDGE('',*,*,#15528,.F.);
#21819=ORIENTED_EDGE('',*,*,#15404,.F.);
#21820=ORIENTED_EDGE('',*,*,#15529,.T.);
#21821=ORIENTED_EDGE('',*,*,#15530,.T.);
#21822=ORIENTED_EDGE('',*,*,#15450,.T.);
#21823=ORIENTED_EDGE('',*,*,#15531,.F.);
#21824=ORIENTED_EDGE('',*,*,#15532,.T.);
#21825=ORIENTED_EDGE('',*,*,#15531,.T.);
#21826=ORIENTED_EDGE('',*,*,#15449,.T.);
#21827=ORIENTED_EDGE('',*,*,#15533,.F.);
#21828=ORIENTED_EDGE('',*,*,#14596,.F.);
#21829=ORIENTED_EDGE('',*,*,#15534,.T.);
#21830=ORIENTED_EDGE('',*,*,#15533,.T.);
#21831=ORIENTED_EDGE('',*,*,#15448,.T.);
#21832=ORIENTED_EDGE('',*,*,#15535,.F.);
#21833=ORIENTED_EDGE('',*,*,#15536,.T.);
#21834=ORIENTED_EDGE('',*,*,#15535,.T.);
#21835=ORIENTED_EDGE('',*,*,#15447,.T.);
#21836=ORIENTED_EDGE('',*,*,#15453,.F.);
#21837=ORIENTED_EDGE('',*,*,#15530,.F.);
#21838=ORIENTED_EDGE('',*,*,#15537,.T.);
#21839=ORIENTED_EDGE('',*,*,#15538,.T.);
#21840=ORIENTED_EDGE('',*,*,#15402,.F.);
#21841=ORIENTED_EDGE('',*,*,#15393,.F.);
#21842=ORIENTED_EDGE('',*,*,#15397,.F.);
#21843=ORIENTED_EDGE('',*,*,#14664,.F.);
#21844=ORIENTED_EDGE('',*,*,#14660,.F.);
#21845=ORIENTED_EDGE('',*,*,#15390,.F.);
#21846=ORIENTED_EDGE('',*,*,#15451,.T.);
#21847=ORIENTED_EDGE('',*,*,#15538,.F.);
#21848=ORIENTED_EDGE('',*,*,#15539,.T.);
#21849=ORIENTED_EDGE('',*,*,#15526,.T.);
#21850=ORIENTED_EDGE('',*,*,#15403,.F.);
#21851=ORIENTED_EDGE('',*,*,#15528,.T.);
#21852=ORIENTED_EDGE('',*,*,#15540,.T.);
#21853=ORIENTED_EDGE('',*,*,#15523,.T.);
#21854=ORIENTED_EDGE('',*,*,#15405,.F.);
#21855=ORIENTED_EDGE('',*,*,#15525,.T.);
#21856=ORIENTED_EDGE('',*,*,#15541,.T.);
#21857=ORIENTED_EDGE('',*,*,#15521,.T.);
#21858=ORIENTED_EDGE('',*,*,#15407,.F.);
#21859=ORIENTED_EDGE('',*,*,#15517,.T.);
#21860=ORIENTED_EDGE('',*,*,#15542,.T.);
#21861=ORIENTED_EDGE('',*,*,#15512,.T.);
#21862=ORIENTED_EDGE('',*,*,#15411,.F.);
#21863=ORIENTED_EDGE('',*,*,#15490,.T.);
#21864=ORIENTED_EDGE('',*,*,#15543,.T.);
#21865=ORIENTED_EDGE('',*,*,#15486,.T.);
#21866=ORIENTED_EDGE('',*,*,#15425,.F.);
#21867=ORIENTED_EDGE('',*,*,#15475,.T.);
#21868=ORIENTED_EDGE('',*,*,#15544,.T.);
#21869=ORIENTED_EDGE('',*,*,#15467,.T.);
#21870=ORIENTED_EDGE('',*,*,#15433,.F.);
#21871=ORIENTED_EDGE('',*,*,#15444,.F.);
#21872=ORIENTED_EDGE('',*,*,#15463,.T.);
#21873=ORIENTED_EDGE('',*,*,#15545,.F.);
#21874=ORIENTED_EDGE('',*,*,#15546,.F.);
#21875=ORIENTED_EDGE('',*,*,#15445,.T.);
#21876=ORIENTED_EDGE('',*,*,#15546,.T.);
#21877=ORIENTED_EDGE('',*,*,#15547,.T.);
#21878=ORIENTED_EDGE('',*,*,#15454,.T.);
#21879=ORIENTED_EDGE('',*,*,#14599,.F.);
#21880=ORIENTED_EDGE('',*,*,#15547,.F.);
#21881=ORIENTED_EDGE('',*,*,#15545,.T.);
#21882=ORIENTED_EDGE('',*,*,#15462,.F.);
#21883=ORIENTED_EDGE('',*,*,#15455,.F.);
#21884=ORIENTED_EDGE('',*,*,#15458,.F.);
#21885=ORIENTED_EDGE('',*,*,#15460,.F.);
#21886=ORIENTED_EDGE('',*,*,#15473,.F.);
#21887=ORIENTED_EDGE('',*,*,#15471,.F.);
#21888=ORIENTED_EDGE('',*,*,#15465,.F.);
#21889=ORIENTED_EDGE('',*,*,#15470,.F.);
#21890=ORIENTED_EDGE('',*,*,#15468,.F.);
#21891=ORIENTED_EDGE('',*,*,#15544,.F.);
#21892=ORIENTED_EDGE('',*,*,#15474,.F.);
#21893=ORIENTED_EDGE('',*,*,#15480,.F.);
#21894=ORIENTED_EDGE('',*,*,#15477,.F.);
#21895=ORIENTED_EDGE('',*,*,#15488,.F.);
#21896=ORIENTED_EDGE('',*,*,#15481,.F.);
#21897=ORIENTED_EDGE('',*,*,#15487,.F.);
#21898=ORIENTED_EDGE('',*,*,#15484,.F.);
#21899=ORIENTED_EDGE('',*,*,#15543,.F.);
#21900=ORIENTED_EDGE('',*,*,#15489,.F.);
#21901=ORIENTED_EDGE('',*,*,#15495,.F.);
#21902=ORIENTED_EDGE('',*,*,#15492,.F.);
#21903=ORIENTED_EDGE('',*,*,#15499,.F.);
#21904=ORIENTED_EDGE('',*,*,#15497,.F.);
#21905=ORIENTED_EDGE('',*,*,#15515,.F.);
#21906=ORIENTED_EDGE('',*,*,#15500,.F.);
#21907=ORIENTED_EDGE('',*,*,#15506,.F.);
#21908=ORIENTED_EDGE('',*,*,#15503,.F.);
#21909=ORIENTED_EDGE('',*,*,#15514,.F.);
#21910=ORIENTED_EDGE('',*,*,#15507,.F.);
#21911=ORIENTED_EDGE('',*,*,#15513,.F.);
#21912=ORIENTED_EDGE('',*,*,#15510,.F.);
#21913=ORIENTED_EDGE('',*,*,#15542,.F.);
#21914=ORIENTED_EDGE('',*,*,#15516,.F.);
#21915=ORIENTED_EDGE('',*,*,#15522,.F.);
#21916=ORIENTED_EDGE('',*,*,#15519,.F.);
#21917=ORIENTED_EDGE('',*,*,#15541,.F.);
#21918=ORIENTED_EDGE('',*,*,#15524,.F.);
#21919=ORIENTED_EDGE('',*,*,#15540,.F.);
#21920=ORIENTED_EDGE('',*,*,#15527,.F.);
#21921=ORIENTED_EDGE('',*,*,#15539,.F.);
#21922=ORIENTED_EDGE('',*,*,#15537,.F.);
#21923=ORIENTED_EDGE('',*,*,#15529,.F.);
#21924=ORIENTED_EDGE('',*,*,#15532,.F.);
#21925=ORIENTED_EDGE('',*,*,#15534,.F.);
#21926=ORIENTED_EDGE('',*,*,#15536,.F.);
#21927=ORIENTED_EDGE('',*,*,#15452,.T.);
#21928=ORIENTED_EDGE('',*,*,#14942,.T.);
#21929=ORIENTED_EDGE('',*,*,#14940,.T.);
#21930=ORIENTED_EDGE('',*,*,#14938,.T.);
#21931=ORIENTED_EDGE('',*,*,#14936,.T.);
#21932=ORIENTED_EDGE('',*,*,#14934,.T.);
#21933=ORIENTED_EDGE('',*,*,#14932,.T.);
#21934=ORIENTED_EDGE('',*,*,#14930,.T.);
#21935=ORIENTED_EDGE('',*,*,#14928,.T.);
#21936=ORIENTED_EDGE('',*,*,#14926,.T.);
#21937=ORIENTED_EDGE('',*,*,#14924,.T.);
#21938=ORIENTED_EDGE('',*,*,#14922,.T.);
#21939=ORIENTED_EDGE('',*,*,#14920,.T.);
#21940=ORIENTED_EDGE('',*,*,#14918,.T.);
#21941=ORIENTED_EDGE('',*,*,#14916,.T.);
#21942=ORIENTED_EDGE('',*,*,#14914,.T.);
#21943=ORIENTED_EDGE('',*,*,#14912,.T.);
#21944=ORIENTED_EDGE('',*,*,#14910,.T.);
#21945=ORIENTED_EDGE('',*,*,#14908,.T.);
#21946=ORIENTED_EDGE('',*,*,#14906,.T.);
#21947=ORIENTED_EDGE('',*,*,#14904,.T.);
#21948=ORIENTED_EDGE('',*,*,#14902,.T.);
#21949=ORIENTED_EDGE('',*,*,#14900,.T.);
#21950=ORIENTED_EDGE('',*,*,#14898,.T.);
#21951=ORIENTED_EDGE('',*,*,#14896,.T.);
#21952=ORIENTED_EDGE('',*,*,#14894,.T.);
#21953=ORIENTED_EDGE('',*,*,#14892,.T.);
#21954=ORIENTED_EDGE('',*,*,#14890,.T.);
#21955=ORIENTED_EDGE('',*,*,#14888,.T.);
#21956=ORIENTED_EDGE('',*,*,#14886,.T.);
#21957=ORIENTED_EDGE('',*,*,#14884,.T.);
#21958=ORIENTED_EDGE('',*,*,#14882,.T.);
#21959=ORIENTED_EDGE('',*,*,#14880,.T.);
#21960=ORIENTED_EDGE('',*,*,#14878,.T.);
#21961=ORIENTED_EDGE('',*,*,#14876,.T.);
#21962=ORIENTED_EDGE('',*,*,#14874,.T.);
#21963=ORIENTED_EDGE('',*,*,#14872,.T.);
#21964=ORIENTED_EDGE('',*,*,#14870,.T.);
#21965=ORIENTED_EDGE('',*,*,#14868,.T.);
#21966=ORIENTED_EDGE('',*,*,#14866,.T.);
#21967=ORIENTED_EDGE('',*,*,#14864,.T.);
#21968=ORIENTED_EDGE('',*,*,#14862,.T.);
#21969=ORIENTED_EDGE('',*,*,#14860,.T.);
#21970=ORIENTED_EDGE('',*,*,#14858,.T.);
#21971=ORIENTED_EDGE('',*,*,#14855,.T.);
#21972=ORIENTED_EDGE('',*,*,#14947,.T.);
#21973=ORIENTED_EDGE('',*,*,#15012,.F.);
#21974=ORIENTED_EDGE('',*,*,#15548,.F.);
#21975=ORIENTED_EDGE('',*,*,#15549,.T.);
#21976=ORIENTED_EDGE('',*,*,#14948,.T.);
#21977=ORIENTED_EDGE('',*,*,#15549,.F.);
#21978=ORIENTED_EDGE('',*,*,#15550,.F.);
#21979=ORIENTED_EDGE('',*,*,#15551,.T.);
#21980=ORIENTED_EDGE('',*,*,#14949,.T.);
#21981=ORIENTED_EDGE('',*,*,#15551,.F.);
#21982=ORIENTED_EDGE('',*,*,#15552,.F.);
#21983=ORIENTED_EDGE('',*,*,#15015,.T.);
#21984=ORIENTED_EDGE('',*,*,#15011,.T.);
#21985=ORIENTED_EDGE('',*,*,#15552,.T.);
#21986=ORIENTED_EDGE('',*,*,#15550,.T.);
#21987=ORIENTED_EDGE('',*,*,#15548,.T.);
#21988=ORIENTED_EDGE('',*,*,#15203,.F.);
#21989=ORIENTED_EDGE('',*,*,#15114,.F.);
#21990=ORIENTED_EDGE('',*,*,#15187,.T.);
#21991=ORIENTED_EDGE('',*,*,#14661,.T.);
#21992=ORIENTED_EDGE('',*,*,#14663,.T.);
#21993=ORIENTED_EDGE('',*,*,#15195,.T.);
#21994=ORIENTED_EDGE('',*,*,#15199,.F.);
#21995=ORIENTED_EDGE('',*,*,#15371,.F.);
#21996=ORIENTED_EDGE('',*,*,#15375,.F.);
#21997=ORIENTED_EDGE('',*,*,#15377,.T.);
#21998=ORIENTED_EDGE('',*,*,#15388,.T.);
#21999=ORIENTED_EDGE('',*,*,#14659,.T.);
#22000=ORIENTED_EDGE('',*,*,#15186,.T.);
#22001=ORIENTED_EDGE('',*,*,#15178,.F.);
#22002=ORIENTED_EDGE('',*,*,#15188,.F.);
#22003=ORIENTED_EDGE('',*,*,#15193,.F.);
#22004=ORIENTED_EDGE('',*,*,#15204,.T.);
#22005=ORIENTED_EDGE('',*,*,#15400,.T.);
#22006=ORIENTED_EDGE('',*,*,#14657,.T.);
#22007=ORIENTED_EDGE('',*,*,#15208,.T.);
#22008=ORIENTED_EDGE('',*,*,#15117,.F.);
#22009=ORIENTED_EDGE('',*,*,#15207,.T.);
#22010=ORIENTED_EDGE('',*,*,#14655,.T.);
#22011=ORIENTED_EDGE('',*,*,#14651,.T.);
#22012=ORIENTED_EDGE('',*,*,#15380,.T.);
#22013=ORIENTED_EDGE('',*,*,#15384,.F.);
#22014=ORIENTED_EDGE('',*,*,#15387,.F.);
#22015=ORIENTED_EDGE('',*,*,#15184,.F.);
#22016=ORIENTED_EDGE('',*,*,#15553,.T.);
#22017=ORIENTED_EDGE('',*,*,#15554,.T.);
#22018=ORIENTED_EDGE('',*,*,#15555,.T.);
#22019=ORIENTED_EDGE('',*,*,#15554,.F.);
#22020=ORIENTED_EDGE('',*,*,#15555,.F.);
#22021=ORIENTED_EDGE('',*,*,#15556,.T.);
#22022=ORIENTED_EDGE('',*,*,#15557,.T.);
#22023=ORIENTED_EDGE('',*,*,#15556,.F.);
#22024=ORIENTED_EDGE('',*,*,#15557,.F.);
#22025=ORIENTED_EDGE('',*,*,#15558,.T.);
#22026=ORIENTED_EDGE('',*,*,#15559,.T.);
#22027=ORIENTED_EDGE('',*,*,#15558,.F.);
#22028=ORIENTED_EDGE('',*,*,#15560,.F.);
#22029=ORIENTED_EDGE('',*,*,#15561,.T.);
#22030=ORIENTED_EDGE('',*,*,#15562,.F.);
#22031=ORIENTED_EDGE('',*,*,#15563,.F.);
#22032=ORIENTED_EDGE('',*,*,#15564,.T.);
#22033=ORIENTED_EDGE('',*,*,#15565,.F.);
#22034=ORIENTED_EDGE('',*,*,#15566,.F.);
#22035=ORIENTED_EDGE('',*,*,#15567,.F.);
#22036=ORIENTED_EDGE('',*,*,#15568,.F.);
#22037=ORIENTED_EDGE('',*,*,#15569,.T.);
#22038=ORIENTED_EDGE('',*,*,#15570,.T.);
#22039=ORIENTED_EDGE('',*,*,#15569,.F.);
#22040=ORIENTED_EDGE('',*,*,#15571,.F.);
#22041=ORIENTED_EDGE('',*,*,#15572,.F.);
#22042=ORIENTED_EDGE('',*,*,#15571,.T.);
#22043=ORIENTED_EDGE('',*,*,#15568,.T.);
#22044=ORIENTED_EDGE('',*,*,#15573,.F.);
#22045=ORIENTED_EDGE('',*,*,#15574,.F.);
#22046=ORIENTED_EDGE('',*,*,#15575,.T.);
#22047=ORIENTED_EDGE('',*,*,#15576,.T.);
#22048=ORIENTED_EDGE('',*,*,#15577,.T.);
#22049=ORIENTED_EDGE('',*,*,#15578,.T.);
#22050=ORIENTED_EDGE('',*,*,#15579,.T.);
#22051=ORIENTED_EDGE('',*,*,#15580,.T.);
#22052=ORIENTED_EDGE('',*,*,#15581,.T.);
#22053=ORIENTED_EDGE('',*,*,#15575,.F.);
#22054=ORIENTED_EDGE('',*,*,#15572,.T.);
#22055=ORIENTED_EDGE('',*,*,#15574,.T.);
#22056=ORIENTED_EDGE('',*,*,#15582,.T.);
#22057=ORIENTED_EDGE('',*,*,#15582,.F.);
#22058=ORIENTED_EDGE('',*,*,#15573,.T.);
#22059=ORIENTED_EDGE('',*,*,#15567,.T.);
#22060=ORIENTED_EDGE('',*,*,#15583,.F.);
#22061=ORIENTED_EDGE('',*,*,#15561,.F.);
#22062=ORIENTED_EDGE('',*,*,#15584,.F.);
#22063=ORIENTED_EDGE('',*,*,#15585,.F.);
#22064=ORIENTED_EDGE('',*,*,#15586,.F.);
#22065=ORIENTED_EDGE('',*,*,#15587,.F.);
#22066=ORIENTED_EDGE('',*,*,#15553,.F.);
#22067=ORIENTED_EDGE('',*,*,#15588,.F.);
#22068=ORIENTED_EDGE('',*,*,#15564,.F.);
#22069=ORIENTED_EDGE('',*,*,#15589,.F.);
#22070=ORIENTED_EDGE('',*,*,#15590,.F.);
#22071=ORIENTED_EDGE('',*,*,#15591,.F.);
#22072=ORIENTED_EDGE('',*,*,#15592,.T.);
#22073=ORIENTED_EDGE('',*,*,#15570,.F.);
#22074=ORIENTED_EDGE('',*,*,#15579,.F.);
#22075=ORIENTED_EDGE('',*,*,#15593,.F.);
#22076=ORIENTED_EDGE('',*,*,#15594,.F.);
#22077=ORIENTED_EDGE('',*,*,#15580,.F.);
#22078=ORIENTED_EDGE('',*,*,#15595,.F.);
#22079=ORIENTED_EDGE('',*,*,#15596,.F.);
#22080=ORIENTED_EDGE('',*,*,#15581,.F.);
#22081=ORIENTED_EDGE('',*,*,#15597,.F.);
#22082=ORIENTED_EDGE('',*,*,#15598,.F.);
#22083=ORIENTED_EDGE('',*,*,#15576,.F.);
#22084=ORIENTED_EDGE('',*,*,#15599,.F.);
#22085=ORIENTED_EDGE('',*,*,#15600,.F.);
#22086=ORIENTED_EDGE('',*,*,#15577,.F.);
#22087=ORIENTED_EDGE('',*,*,#15601,.F.);
#22088=ORIENTED_EDGE('',*,*,#15602,.F.);
#22089=ORIENTED_EDGE('',*,*,#15578,.F.);
#22090=ORIENTED_EDGE('',*,*,#15603,.F.);
#22091=ORIENTED_EDGE('',*,*,#15604,.F.);
#22092=ORIENTED_EDGE('',*,*,#15605,.F.);
#22093=ORIENTED_EDGE('',*,*,#15606,.F.);
#22094=ORIENTED_EDGE('',*,*,#15597,.T.);
#22095=ORIENTED_EDGE('',*,*,#15596,.T.);
#22096=ORIENTED_EDGE('',*,*,#15607,.T.);
#22097=ORIENTED_EDGE('',*,*,#15608,.F.);
#22098=ORIENTED_EDGE('',*,*,#15609,.F.);
#22099=ORIENTED_EDGE('',*,*,#15599,.T.);
#22100=ORIENTED_EDGE('',*,*,#15598,.T.);
#22101=ORIENTED_EDGE('',*,*,#15606,.T.);
#22102=ORIENTED_EDGE('',*,*,#15610,.F.);
#22103=ORIENTED_EDGE('',*,*,#15611,.F.);
#22104=ORIENTED_EDGE('',*,*,#15601,.T.);
#22105=ORIENTED_EDGE('',*,*,#15600,.T.);
#22106=ORIENTED_EDGE('',*,*,#15609,.T.);
#22107=ORIENTED_EDGE('',*,*,#15612,.F.);
#22108=ORIENTED_EDGE('',*,*,#15613,.F.);
#22109=ORIENTED_EDGE('',*,*,#15603,.T.);
#22110=ORIENTED_EDGE('',*,*,#15602,.T.);
#22111=ORIENTED_EDGE('',*,*,#15611,.T.);
#22112=ORIENTED_EDGE('',*,*,#15614,.F.);
#22113=ORIENTED_EDGE('',*,*,#15615,.F.);
#22114=ORIENTED_EDGE('',*,*,#15593,.T.);
#22115=ORIENTED_EDGE('',*,*,#15604,.T.);
#22116=ORIENTED_EDGE('',*,*,#15613,.T.);
#22117=ORIENTED_EDGE('',*,*,#15616,.F.);
#22118=ORIENTED_EDGE('',*,*,#15607,.F.);
#22119=ORIENTED_EDGE('',*,*,#15595,.T.);
#22120=ORIENTED_EDGE('',*,*,#15594,.T.);
#22121=ORIENTED_EDGE('',*,*,#15615,.T.);
#22122=ORIENTED_EDGE('',*,*,#15605,.T.);
#22123=ORIENTED_EDGE('',*,*,#15616,.T.);
#22124=ORIENTED_EDGE('',*,*,#15614,.T.);
#22125=ORIENTED_EDGE('',*,*,#15612,.T.);
#22126=ORIENTED_EDGE('',*,*,#15610,.T.);
#22127=ORIENTED_EDGE('',*,*,#15608,.T.);
#22128=ORIENTED_EDGE('',*,*,#15617,.F.);
#22129=ORIENTED_EDGE('',*,*,#15589,.T.);
#22130=ORIENTED_EDGE('',*,*,#15618,.F.);
#22131=ORIENTED_EDGE('',*,*,#15619,.F.);
#22132=ORIENTED_EDGE('',*,*,#15590,.T.);
#22133=ORIENTED_EDGE('',*,*,#15620,.F.);
#22134=ORIENTED_EDGE('',*,*,#15591,.T.);
#22135=ORIENTED_EDGE('',*,*,#15621,.F.);
#22136=ORIENTED_EDGE('',*,*,#15622,.F.);
#22137=ORIENTED_EDGE('',*,*,#15592,.F.);
#22138=ORIENTED_EDGE('',*,*,#15623,.F.);
#22139=ORIENTED_EDGE('',*,*,#15624,.F.);
#22140=ORIENTED_EDGE('',*,*,#15588,.T.);
#22141=ORIENTED_EDGE('',*,*,#15625,.F.);
#22142=ORIENTED_EDGE('',*,*,#15626,.F.);
#22143=ORIENTED_EDGE('',*,*,#15583,.T.);
#22144=ORIENTED_EDGE('',*,*,#15627,.F.);
#22145=ORIENTED_EDGE('',*,*,#15628,.F.);
#22146=ORIENTED_EDGE('',*,*,#15587,.T.);
#22147=ORIENTED_EDGE('',*,*,#15629,.F.);
#22148=ORIENTED_EDGE('',*,*,#15630,.F.);
#22149=ORIENTED_EDGE('',*,*,#15586,.T.);
#22150=ORIENTED_EDGE('',*,*,#15631,.F.);
#22151=ORIENTED_EDGE('',*,*,#15632,.F.);
#22152=ORIENTED_EDGE('',*,*,#15585,.T.);
#22153=ORIENTED_EDGE('',*,*,#15633,.F.);
#22154=ORIENTED_EDGE('',*,*,#15634,.F.);
#22155=ORIENTED_EDGE('',*,*,#15584,.T.);
#22156=ORIENTED_EDGE('',*,*,#15635,.F.);
#22157=ORIENTED_EDGE('',*,*,#15636,.F.);
#22158=ORIENTED_EDGE('',*,*,#15637,.F.);
#22159=ORIENTED_EDGE('',*,*,#15621,.T.);
#22160=ORIENTED_EDGE('',*,*,#15619,.T.);
#22161=ORIENTED_EDGE('',*,*,#15638,.T.);
#22162=ORIENTED_EDGE('',*,*,#15635,.T.);
#22163=ORIENTED_EDGE('',*,*,#15563,.T.);
#22164=ORIENTED_EDGE('',*,*,#15638,.F.);
#22165=ORIENTED_EDGE('',*,*,#15620,.T.);
#22166=ORIENTED_EDGE('',*,*,#15617,.T.);
#22167=ORIENTED_EDGE('',*,*,#15639,.T.);
#22168=ORIENTED_EDGE('',*,*,#15633,.T.);
#22169=ORIENTED_EDGE('',*,*,#15636,.T.);
#22170=ORIENTED_EDGE('',*,*,#15639,.F.);
#22171=ORIENTED_EDGE('',*,*,#15618,.T.);
#22172=ORIENTED_EDGE('',*,*,#15566,.T.);
#22173=ORIENTED_EDGE('',*,*,#15640,.T.);
#22174=ORIENTED_EDGE('',*,*,#15631,.T.);
#22175=ORIENTED_EDGE('',*,*,#15634,.T.);
#22176=ORIENTED_EDGE('',*,*,#15640,.F.);
#22177=ORIENTED_EDGE('',*,*,#15565,.T.);
#22178=ORIENTED_EDGE('',*,*,#15626,.T.);
#22179=ORIENTED_EDGE('',*,*,#15641,.T.);
#22180=ORIENTED_EDGE('',*,*,#15629,.T.);
#22181=ORIENTED_EDGE('',*,*,#15632,.T.);
#22182=ORIENTED_EDGE('',*,*,#15641,.F.);
#22183=ORIENTED_EDGE('',*,*,#15625,.T.);
#22184=ORIENTED_EDGE('',*,*,#15624,.T.);
#22185=ORIENTED_EDGE('',*,*,#15642,.T.);
#22186=ORIENTED_EDGE('',*,*,#15627,.T.);
#22187=ORIENTED_EDGE('',*,*,#15630,.T.);
#22188=ORIENTED_EDGE('',*,*,#15642,.F.);
#22189=ORIENTED_EDGE('',*,*,#15623,.T.);
#22190=ORIENTED_EDGE('',*,*,#15622,.T.);
#22191=ORIENTED_EDGE('',*,*,#15637,.T.);
#22192=ORIENTED_EDGE('',*,*,#15562,.T.);
#22193=ORIENTED_EDGE('',*,*,#15628,.T.);
#22194=ORIENTED_EDGE('',*,*,#15559,.F.);
#22195=ORIENTED_EDGE('',*,*,#15560,.T.);
#22196=ORIENTED_EDGE('',*,*,#15643,.F.);
#22197=ORIENTED_EDGE('',*,*,#15644,.T.);
#22198=ORIENTED_EDGE('',*,*,#15645,.T.);
#22199=ORIENTED_EDGE('',*,*,#15644,.F.);
#22200=ORIENTED_EDGE('',*,*,#15646,.T.);
#22201=ORIENTED_EDGE('',*,*,#15643,.T.);
#22202=ORIENTED_EDGE('',*,*,#15646,.F.);
#22203=ORIENTED_EDGE('',*,*,#15647,.F.);
#22204=ORIENTED_EDGE('',*,*,#15648,.T.);
#22205=ORIENTED_EDGE('',*,*,#15649,.T.);
#22206=ORIENTED_EDGE('',*,*,#15648,.F.);
#22207=ORIENTED_EDGE('',*,*,#15650,.T.);
#22208=ORIENTED_EDGE('',*,*,#15647,.T.);
#22209=ORIENTED_EDGE('',*,*,#15650,.F.);
#22210=ORIENTED_EDGE('',*,*,#15651,.F.);
#22211=ORIENTED_EDGE('',*,*,#15652,.T.);
#22212=ORIENTED_EDGE('',*,*,#15653,.T.);
#22213=ORIENTED_EDGE('',*,*,#15652,.F.);
#22214=ORIENTED_EDGE('',*,*,#15654,.T.);
#22215=ORIENTED_EDGE('',*,*,#15651,.T.);
#22216=ORIENTED_EDGE('',*,*,#15654,.F.);
#22217=ORIENTED_EDGE('',*,*,#15655,.F.);
#22218=ORIENTED_EDGE('',*,*,#15656,.T.);
#22219=ORIENTED_EDGE('',*,*,#15657,.T.);
#22220=ORIENTED_EDGE('',*,*,#15656,.F.);
#22221=ORIENTED_EDGE('',*,*,#15658,.T.);
#22222=ORIENTED_EDGE('',*,*,#15655,.T.);
#22223=ORIENTED_EDGE('',*,*,#15658,.F.);
#22224=ORIENTED_EDGE('',*,*,#15659,.F.);
#22225=ORIENTED_EDGE('',*,*,#15660,.T.);
#22226=ORIENTED_EDGE('',*,*,#15661,.T.);
#22227=ORIENTED_EDGE('',*,*,#15660,.F.);
#22228=ORIENTED_EDGE('',*,*,#15662,.T.);
#22229=ORIENTED_EDGE('',*,*,#15659,.T.);
#22230=ORIENTED_EDGE('',*,*,#15662,.F.);
#22231=ORIENTED_EDGE('',*,*,#15663,.F.);
#22232=ORIENTED_EDGE('',*,*,#15664,.T.);
#22233=ORIENTED_EDGE('',*,*,#15665,.T.);
#22234=ORIENTED_EDGE('',*,*,#15664,.F.);
#22235=ORIENTED_EDGE('',*,*,#15666,.T.);
#22236=ORIENTED_EDGE('',*,*,#15663,.T.);
#22237=ORIENTED_EDGE('',*,*,#15666,.F.);
#22238=ORIENTED_EDGE('',*,*,#15667,.F.);
#22239=ORIENTED_EDGE('',*,*,#15668,.T.);
#22240=ORIENTED_EDGE('',*,*,#15669,.T.);
#22241=ORIENTED_EDGE('',*,*,#15668,.F.);
#22242=ORIENTED_EDGE('',*,*,#15670,.T.);
#22243=ORIENTED_EDGE('',*,*,#15667,.T.);
#22244=ORIENTED_EDGE('',*,*,#15670,.F.);
#22245=ORIENTED_EDGE('',*,*,#15671,.F.);
#22246=ORIENTED_EDGE('',*,*,#15672,.T.);
#22247=ORIENTED_EDGE('',*,*,#15673,.T.);
#22248=ORIENTED_EDGE('',*,*,#15672,.F.);
#22249=ORIENTED_EDGE('',*,*,#15674,.T.);
#22250=ORIENTED_EDGE('',*,*,#15671,.T.);
#22251=ORIENTED_EDGE('',*,*,#15674,.F.);
#22252=ORIENTED_EDGE('',*,*,#15675,.T.);
#22253=ORIENTED_EDGE('',*,*,#15676,.T.);
#22254=ORIENTED_EDGE('',*,*,#15677,.F.);
#22255=ORIENTED_EDGE('',*,*,#15678,.F.);
#22256=ORIENTED_EDGE('',*,*,#15677,.T.);
#22257=ORIENTED_EDGE('',*,*,#15679,.F.);
#22258=ORIENTED_EDGE('',*,*,#15680,.T.);
#22259=ORIENTED_EDGE('',*,*,#15681,.F.);
#22260=ORIENTED_EDGE('',*,*,#15682,.T.);
#22261=ORIENTED_EDGE('',*,*,#15683,.F.);
#22262=ORIENTED_EDGE('',*,*,#15684,.T.);
#22263=ORIENTED_EDGE('',*,*,#15685,.T.);
#22264=ORIENTED_EDGE('',*,*,#15686,.F.);
#22265=ORIENTED_EDGE('',*,*,#15687,.F.);
#22266=ORIENTED_EDGE('',*,*,#15688,.T.);
#22267=ORIENTED_EDGE('',*,*,#15689,.F.);
#22268=ORIENTED_EDGE('',*,*,#15690,.F.);
#22269=ORIENTED_EDGE('',*,*,#15686,.T.);
#22270=ORIENTED_EDGE('',*,*,#15691,.T.);
#22271=ORIENTED_EDGE('',*,*,#15692,.T.);
#22272=ORIENTED_EDGE('',*,*,#15693,.T.);
#22273=ORIENTED_EDGE('',*,*,#15694,.T.);
#22274=ORIENTED_EDGE('',*,*,#15695,.T.);
#22275=ORIENTED_EDGE('',*,*,#15675,.F.);
#22276=ORIENTED_EDGE('',*,*,#15696,.F.);
#22277=ORIENTED_EDGE('',*,*,#15689,.T.);
#22278=ORIENTED_EDGE('',*,*,#15697,.T.);
#22279=ORIENTED_EDGE('',*,*,#15698,.F.);
#22280=ORIENTED_EDGE('',*,*,#15684,.F.);
#22281=ORIENTED_EDGE('',*,*,#15699,.F.);
#22282=ORIENTED_EDGE('',*,*,#15698,.T.);
#22283=ORIENTED_EDGE('',*,*,#15700,.T.);
#22284=ORIENTED_EDGE('',*,*,#15687,.T.);
#22285=ORIENTED_EDGE('',*,*,#15690,.T.);
#22286=ORIENTED_EDGE('',*,*,#15696,.T.);
#22287=ORIENTED_EDGE('',*,*,#15678,.T.);
#22288=ORIENTED_EDGE('',*,*,#15685,.F.);
#22289=ORIENTED_EDGE('',*,*,#15700,.F.);
#22290=ORIENTED_EDGE('',*,*,#15697,.F.);
#22291=ORIENTED_EDGE('',*,*,#15688,.F.);
#22292=ORIENTED_EDGE('',*,*,#15695,.F.);
#22293=ORIENTED_EDGE('',*,*,#15701,.T.);
#22294=ORIENTED_EDGE('',*,*,#15679,.T.);
#22295=ORIENTED_EDGE('',*,*,#15676,.F.);
#22296=ORIENTED_EDGE('',*,*,#15693,.F.);
#22297=ORIENTED_EDGE('',*,*,#15702,.T.);
#22298=ORIENTED_EDGE('',*,*,#15681,.T.);
#22299=ORIENTED_EDGE('',*,*,#15703,.T.);
#22300=ORIENTED_EDGE('',*,*,#15645,.F.);
#22301=ORIENTED_EDGE('',*,*,#15649,.F.);
#22302=ORIENTED_EDGE('',*,*,#15653,.F.);
#22303=ORIENTED_EDGE('',*,*,#15657,.F.);
#22304=ORIENTED_EDGE('',*,*,#15661,.F.);
#22305=ORIENTED_EDGE('',*,*,#15665,.F.);
#22306=ORIENTED_EDGE('',*,*,#15669,.F.);
#22307=ORIENTED_EDGE('',*,*,#15673,.F.);
#22308=ORIENTED_EDGE('',*,*,#15683,.T.);
#22309=ORIENTED_EDGE('',*,*,#15704,.T.);
#22310=ORIENTED_EDGE('',*,*,#15691,.F.);
#22311=ORIENTED_EDGE('',*,*,#15699,.T.);
#22312=ORIENTED_EDGE('',*,*,#15692,.F.);
#22313=ORIENTED_EDGE('',*,*,#15704,.F.);
#22314=ORIENTED_EDGE('',*,*,#15682,.F.);
#22315=ORIENTED_EDGE('',*,*,#15702,.F.);
#22316=ORIENTED_EDGE('',*,*,#15694,.F.);
#22317=ORIENTED_EDGE('',*,*,#15703,.F.);
#22318=ORIENTED_EDGE('',*,*,#15680,.F.);
#22319=ORIENTED_EDGE('',*,*,#15701,.F.);
#22320=ORIENTED_EDGE('',*,*,#15705,.F.);
#22321=ORIENTED_EDGE('',*,*,#15706,.F.);
#22322=ORIENTED_EDGE('',*,*,#15707,.T.);
#22323=ORIENTED_EDGE('',*,*,#15708,.F.);
#22324=ORIENTED_EDGE('',*,*,#15707,.F.);
#22325=ORIENTED_EDGE('',*,*,#15709,.T.);
#22326=ORIENTED_EDGE('',*,*,#15710,.T.);
#22327=ORIENTED_EDGE('',*,*,#15711,.T.);
#22328=ORIENTED_EDGE('',*,*,#15712,.T.);
#22329=ORIENTED_EDGE('',*,*,#15713,.T.);
#22330=ORIENTED_EDGE('',*,*,#15714,.T.);
#22331=ORIENTED_EDGE('',*,*,#15715,.T.);
#22332=ORIENTED_EDGE('',*,*,#15716,.T.);
#22333=ORIENTED_EDGE('',*,*,#15709,.F.);
#22334=ORIENTED_EDGE('',*,*,#15705,.T.);
#22335=ORIENTED_EDGE('',*,*,#15706,.T.);
#22336=ORIENTED_EDGE('',*,*,#15717,.T.);
#22337=ORIENTED_EDGE('',*,*,#15718,.T.);
#22338=ORIENTED_EDGE('',*,*,#15717,.F.);
#22339=ORIENTED_EDGE('',*,*,#15719,.F.);
#22340=ORIENTED_EDGE('',*,*,#15720,.T.);
#22341=ORIENTED_EDGE('',*,*,#15721,.T.);
#22342=ORIENTED_EDGE('',*,*,#15720,.F.);
#22343=ORIENTED_EDGE('',*,*,#15722,.F.);
#22344=ORIENTED_EDGE('',*,*,#15723,.T.);
#22345=ORIENTED_EDGE('',*,*,#15724,.T.);
#22346=ORIENTED_EDGE('',*,*,#15723,.F.);
#22347=ORIENTED_EDGE('',*,*,#15708,.T.);
#22348=ORIENTED_EDGE('',*,*,#15725,.F.);
#22349=ORIENTED_EDGE('',*,*,#15726,.F.);
#22350=ORIENTED_EDGE('',*,*,#15727,.F.);
#22351=ORIENTED_EDGE('',*,*,#15728,.F.);
#22352=ORIENTED_EDGE('',*,*,#15729,.F.);
#22353=ORIENTED_EDGE('',*,*,#15730,.F.);
#22354=ORIENTED_EDGE('',*,*,#15724,.F.);
#22355=ORIENTED_EDGE('',*,*,#15722,.T.);
#22356=ORIENTED_EDGE('',*,*,#15721,.F.);
#22357=ORIENTED_EDGE('',*,*,#15718,.F.);
#22358=ORIENTED_EDGE('',*,*,#15719,.T.);
#22359=ORIENTED_EDGE('',*,*,#15731,.F.);
#22360=ORIENTED_EDGE('',*,*,#15732,.T.);
#22361=ORIENTED_EDGE('',*,*,#15726,.T.);
#22362=ORIENTED_EDGE('',*,*,#15733,.F.);
#22363=ORIENTED_EDGE('',*,*,#15734,.F.);
#22364=ORIENTED_EDGE('',*,*,#15735,.F.);
#22365=ORIENTED_EDGE('',*,*,#15736,.T.);
#22366=ORIENTED_EDGE('',*,*,#15727,.T.);
#22367=ORIENTED_EDGE('',*,*,#15732,.F.);
#22368=ORIENTED_EDGE('',*,*,#15737,.F.);
#22369=ORIENTED_EDGE('',*,*,#15738,.F.);
#22370=ORIENTED_EDGE('',*,*,#15739,.T.);
#22371=ORIENTED_EDGE('',*,*,#15728,.T.);
#22372=ORIENTED_EDGE('',*,*,#15736,.F.);
#22373=ORIENTED_EDGE('',*,*,#15740,.F.);
#22374=ORIENTED_EDGE('',*,*,#15741,.F.);
#22375=ORIENTED_EDGE('',*,*,#15742,.T.);
#22376=ORIENTED_EDGE('',*,*,#15729,.T.);
#22377=ORIENTED_EDGE('',*,*,#15739,.F.);
#22378=ORIENTED_EDGE('',*,*,#15743,.F.);
#22379=ORIENTED_EDGE('',*,*,#15744,.F.);
#22380=ORIENTED_EDGE('',*,*,#15745,.T.);
#22381=ORIENTED_EDGE('',*,*,#15730,.T.);
#22382=ORIENTED_EDGE('',*,*,#15742,.F.);
#22383=ORIENTED_EDGE('',*,*,#15746,.F.);
#22384=ORIENTED_EDGE('',*,*,#15747,.F.);
#22385=ORIENTED_EDGE('',*,*,#15733,.T.);
#22386=ORIENTED_EDGE('',*,*,#15725,.T.);
#22387=ORIENTED_EDGE('',*,*,#15745,.F.);
#22388=ORIENTED_EDGE('',*,*,#15748,.F.);
#22389=ORIENTED_EDGE('',*,*,#15734,.T.);
#22390=ORIENTED_EDGE('',*,*,#15747,.T.);
#22391=ORIENTED_EDGE('',*,*,#15715,.F.);
#22392=ORIENTED_EDGE('',*,*,#15748,.T.);
#22393=ORIENTED_EDGE('',*,*,#15744,.T.);
#22394=ORIENTED_EDGE('',*,*,#15710,.F.);
#22395=ORIENTED_EDGE('',*,*,#15716,.F.);
#22396=ORIENTED_EDGE('',*,*,#15746,.T.);
#22397=ORIENTED_EDGE('',*,*,#15741,.T.);
#22398=ORIENTED_EDGE('',*,*,#15711,.F.);
#22399=ORIENTED_EDGE('',*,*,#15743,.T.);
#22400=ORIENTED_EDGE('',*,*,#15738,.T.);
#22401=ORIENTED_EDGE('',*,*,#15712,.F.);
#22402=ORIENTED_EDGE('',*,*,#15740,.T.);
#22403=ORIENTED_EDGE('',*,*,#15735,.T.);
#22404=ORIENTED_EDGE('',*,*,#15713,.F.);
#22405=ORIENTED_EDGE('',*,*,#15737,.T.);
#22406=ORIENTED_EDGE('',*,*,#15731,.T.);
#22407=ORIENTED_EDGE('',*,*,#15714,.F.);
#22408=ORIENTED_EDGE('',*,*,#15749,.F.);
#22409=ORIENTED_EDGE('',*,*,#15750,.T.);
#22410=ORIENTED_EDGE('',*,*,#15751,.T.);
#22411=ORIENTED_EDGE('',*,*,#15750,.F.);
#22412=ORIENTED_EDGE('',*,*,#15752,.F.);
#22413=ORIENTED_EDGE('',*,*,#15753,.T.);
#22414=ORIENTED_EDGE('',*,*,#15754,.T.);
#22415=ORIENTED_EDGE('',*,*,#15753,.F.);
#22416=ORIENTED_EDGE('',*,*,#15749,.T.);
#22417=ORIENTED_EDGE('',*,*,#15754,.F.);
#22418=ORIENTED_EDGE('',*,*,#15751,.F.);
#22419=ORIENTED_EDGE('',*,*,#15752,.T.);
#22420=ORIENTED_EDGE('',*,*,#15755,.T.);
#22421=ORIENTED_EDGE('',*,*,#15756,.F.);
#22422=ORIENTED_EDGE('',*,*,#15757,.F.);
#22423=ORIENTED_EDGE('',*,*,#15758,.T.);
#22424=ORIENTED_EDGE('',*,*,#15759,.F.);
#22425=ORIENTED_EDGE('',*,*,#15760,.F.);
#22426=ORIENTED_EDGE('',*,*,#15761,.T.);
#22427=ORIENTED_EDGE('',*,*,#15762,.T.);
#22428=ORIENTED_EDGE('',*,*,#15757,.T.);
#22429=ORIENTED_EDGE('',*,*,#15763,.T.);
#22430=ORIENTED_EDGE('',*,*,#15761,.F.);
#22431=ORIENTED_EDGE('',*,*,#15764,.T.);
#22432=ORIENTED_EDGE('',*,*,#15759,.T.);
#22433=ORIENTED_EDGE('',*,*,#15765,.F.);
#22434=ORIENTED_EDGE('',*,*,#15755,.F.);
#22435=ORIENTED_EDGE('',*,*,#15766,.F.);
#22436=ORIENTED_EDGE('',*,*,#15766,.T.);
#22437=ORIENTED_EDGE('',*,*,#15758,.F.);
#22438=ORIENTED_EDGE('',*,*,#15764,.F.);
#22439=ORIENTED_EDGE('',*,*,#15760,.T.);
#22440=ORIENTED_EDGE('',*,*,#15765,.T.);
#22441=ORIENTED_EDGE('',*,*,#15762,.F.);
#22442=ORIENTED_EDGE('',*,*,#15763,.F.);
#22443=ORIENTED_EDGE('',*,*,#15756,.T.);
#22444=ORIENTED_EDGE('',*,*,#15767,.F.);
#22445=ORIENTED_EDGE('',*,*,#15768,.T.);
#22446=ORIENTED_EDGE('',*,*,#15769,.T.);
#22447=ORIENTED_EDGE('',*,*,#15768,.F.);
#22448=ORIENTED_EDGE('',*,*,#15769,.F.);
#22449=ORIENTED_EDGE('',*,*,#15770,.T.);
#22450=ORIENTED_EDGE('',*,*,#15771,.T.);
#22451=ORIENTED_EDGE('',*,*,#15770,.F.);
#22452=ORIENTED_EDGE('',*,*,#15772,.T.);
#22453=ORIENTED_EDGE('',*,*,#15773,.T.);
#22454=ORIENTED_EDGE('',*,*,#15774,.F.);
#22455=ORIENTED_EDGE('',*,*,#15773,.F.);
#22456=ORIENTED_EDGE('',*,*,#15775,.T.);
#22457=ORIENTED_EDGE('',*,*,#15772,.F.);
#22458=ORIENTED_EDGE('',*,*,#15776,.T.);
#22459=ORIENTED_EDGE('',*,*,#15777,.T.);
#22460=ORIENTED_EDGE('',*,*,#15776,.F.);
#22461=ORIENTED_EDGE('',*,*,#15775,.F.);
#22462=ORIENTED_EDGE('',*,*,#15774,.T.);
#22463=ORIENTED_EDGE('',*,*,#15771,.F.);
#22464=ORIENTED_EDGE('',*,*,#15778,.F.);
#22465=ORIENTED_EDGE('',*,*,#15779,.F.);
#22466=ORIENTED_EDGE('',*,*,#15780,.F.);
#22467=ORIENTED_EDGE('',*,*,#15781,.F.);
#22468=ORIENTED_EDGE('',*,*,#15782,.F.);
#22469=ORIENTED_EDGE('',*,*,#15783,.F.);
#22470=ORIENTED_EDGE('',*,*,#15767,.T.);
#22471=ORIENTED_EDGE('',*,*,#15777,.F.);
#22472=ORIENTED_EDGE('',*,*,#15778,.T.);
#22473=ORIENTED_EDGE('',*,*,#15784,.F.);
#22474=ORIENTED_EDGE('',*,*,#15785,.F.);
#22475=ORIENTED_EDGE('',*,*,#15786,.T.);
#22476=ORIENTED_EDGE('',*,*,#15779,.T.);
#22477=ORIENTED_EDGE('',*,*,#15786,.F.);
#22478=ORIENTED_EDGE('',*,*,#15787,.F.);
#22479=ORIENTED_EDGE('',*,*,#15788,.T.);
#22480=ORIENTED_EDGE('',*,*,#15780,.T.);
#22481=ORIENTED_EDGE('',*,*,#15788,.F.);
#22482=ORIENTED_EDGE('',*,*,#15789,.F.);
#22483=ORIENTED_EDGE('',*,*,#15790,.T.);
#22484=ORIENTED_EDGE('',*,*,#15781,.T.);
#22485=ORIENTED_EDGE('',*,*,#15790,.F.);
#22486=ORIENTED_EDGE('',*,*,#15791,.F.);
#22487=ORIENTED_EDGE('',*,*,#15792,.T.);
#22488=ORIENTED_EDGE('',*,*,#15782,.T.);
#22489=ORIENTED_EDGE('',*,*,#15792,.F.);
#22490=ORIENTED_EDGE('',*,*,#15793,.F.);
#22491=ORIENTED_EDGE('',*,*,#15794,.T.);
#22492=ORIENTED_EDGE('',*,*,#15783,.T.);
#22493=ORIENTED_EDGE('',*,*,#15794,.F.);
#22494=ORIENTED_EDGE('',*,*,#15795,.F.);
#22495=ORIENTED_EDGE('',*,*,#15784,.T.);
#22496=ORIENTED_EDGE('',*,*,#15785,.T.);
#22497=ORIENTED_EDGE('',*,*,#15795,.T.);
#22498=ORIENTED_EDGE('',*,*,#15793,.T.);
#22499=ORIENTED_EDGE('',*,*,#15791,.T.);
#22500=ORIENTED_EDGE('',*,*,#15789,.T.);
#22501=ORIENTED_EDGE('',*,*,#15787,.T.);
#22502=ORIENTED_EDGE('',*,*,#15796,.F.);
#22503=ORIENTED_EDGE('',*,*,#15797,.F.);
#22504=ORIENTED_EDGE('',*,*,#15798,.T.);
#22505=ORIENTED_EDGE('',*,*,#15799,.F.);
#22506=ORIENTED_EDGE('',*,*,#15798,.F.);
#22507=ORIENTED_EDGE('',*,*,#15800,.T.);
#22508=ORIENTED_EDGE('',*,*,#15801,.T.);
#22509=ORIENTED_EDGE('',*,*,#15802,.T.);
#22510=ORIENTED_EDGE('',*,*,#15803,.T.);
#22511=ORIENTED_EDGE('',*,*,#15804,.T.);
#22512=ORIENTED_EDGE('',*,*,#15805,.T.);
#22513=ORIENTED_EDGE('',*,*,#15806,.T.);
#22514=ORIENTED_EDGE('',*,*,#15807,.T.);
#22515=ORIENTED_EDGE('',*,*,#15800,.F.);
#22516=ORIENTED_EDGE('',*,*,#15796,.T.);
#22517=ORIENTED_EDGE('',*,*,#15797,.T.);
#22518=ORIENTED_EDGE('',*,*,#15808,.T.);
#22519=ORIENTED_EDGE('',*,*,#15809,.T.);
#22520=ORIENTED_EDGE('',*,*,#15808,.F.);
#22521=ORIENTED_EDGE('',*,*,#15810,.F.);
#22522=ORIENTED_EDGE('',*,*,#15811,.T.);
#22523=ORIENTED_EDGE('',*,*,#15812,.T.);
#22524=ORIENTED_EDGE('',*,*,#15811,.F.);
#22525=ORIENTED_EDGE('',*,*,#15813,.F.);
#22526=ORIENTED_EDGE('',*,*,#15814,.T.);
#22527=ORIENTED_EDGE('',*,*,#15815,.T.);
#22528=ORIENTED_EDGE('',*,*,#15814,.F.);
#22529=ORIENTED_EDGE('',*,*,#15799,.T.);
#22530=ORIENTED_EDGE('',*,*,#15816,.F.);
#22531=ORIENTED_EDGE('',*,*,#15817,.F.);
#22532=ORIENTED_EDGE('',*,*,#15818,.F.);
#22533=ORIENTED_EDGE('',*,*,#15819,.F.);
#22534=ORIENTED_EDGE('',*,*,#15820,.F.);
#22535=ORIENTED_EDGE('',*,*,#15821,.F.);
#22536=ORIENTED_EDGE('',*,*,#15815,.F.);
#22537=ORIENTED_EDGE('',*,*,#15813,.T.);
#22538=ORIENTED_EDGE('',*,*,#15812,.F.);
#22539=ORIENTED_EDGE('',*,*,#15809,.F.);
#22540=ORIENTED_EDGE('',*,*,#15810,.T.);
#22541=ORIENTED_EDGE('',*,*,#15822,.F.);
#22542=ORIENTED_EDGE('',*,*,#15823,.T.);
#22543=ORIENTED_EDGE('',*,*,#15817,.T.);
#22544=ORIENTED_EDGE('',*,*,#15824,.F.);
#22545=ORIENTED_EDGE('',*,*,#15825,.F.);
#22546=ORIENTED_EDGE('',*,*,#15826,.F.);
#22547=ORIENTED_EDGE('',*,*,#15827,.T.);
#22548=ORIENTED_EDGE('',*,*,#15818,.T.);
#22549=ORIENTED_EDGE('',*,*,#15823,.F.);
#22550=ORIENTED_EDGE('',*,*,#15828,.F.);
#22551=ORIENTED_EDGE('',*,*,#15829,.F.);
#22552=ORIENTED_EDGE('',*,*,#15830,.T.);
#22553=ORIENTED_EDGE('',*,*,#15819,.T.);
#22554=ORIENTED_EDGE('',*,*,#15827,.F.);
#22555=ORIENTED_EDGE('',*,*,#15831,.F.);
#22556=ORIENTED_EDGE('',*,*,#15832,.F.);
#22557=ORIENTED_EDGE('',*,*,#15833,.T.);
#22558=ORIENTED_EDGE('',*,*,#15820,.T.);
#22559=ORIENTED_EDGE('',*,*,#15830,.F.);
#22560=ORIENTED_EDGE('',*,*,#15834,.F.);
#22561=ORIENTED_EDGE('',*,*,#15835,.F.);
#22562=ORIENTED_EDGE('',*,*,#15836,.T.);
#22563=ORIENTED_EDGE('',*,*,#15821,.T.);
#22564=ORIENTED_EDGE('',*,*,#15833,.F.);
#22565=ORIENTED_EDGE('',*,*,#15837,.F.);
#22566=ORIENTED_EDGE('',*,*,#15838,.F.);
#22567=ORIENTED_EDGE('',*,*,#15824,.T.);
#22568=ORIENTED_EDGE('',*,*,#15816,.T.);
#22569=ORIENTED_EDGE('',*,*,#15836,.F.);
#22570=ORIENTED_EDGE('',*,*,#15839,.F.);
#22571=ORIENTED_EDGE('',*,*,#15825,.T.);
#22572=ORIENTED_EDGE('',*,*,#15838,.T.);
#22573=ORIENTED_EDGE('',*,*,#15806,.F.);
#22574=ORIENTED_EDGE('',*,*,#15839,.T.);
#22575=ORIENTED_EDGE('',*,*,#15835,.T.);
#22576=ORIENTED_EDGE('',*,*,#15801,.F.);
#22577=ORIENTED_EDGE('',*,*,#15807,.F.);
#22578=ORIENTED_EDGE('',*,*,#15837,.T.);
#22579=ORIENTED_EDGE('',*,*,#15832,.T.);
#22580=ORIENTED_EDGE('',*,*,#15802,.F.);
#22581=ORIENTED_EDGE('',*,*,#15834,.T.);
#22582=ORIENTED_EDGE('',*,*,#15829,.T.);
#22583=ORIENTED_EDGE('',*,*,#15803,.F.);
#22584=ORIENTED_EDGE('',*,*,#15831,.T.);
#22585=ORIENTED_EDGE('',*,*,#15826,.T.);
#22586=ORIENTED_EDGE('',*,*,#15804,.F.);
#22587=ORIENTED_EDGE('',*,*,#15828,.T.);
#22588=ORIENTED_EDGE('',*,*,#15822,.T.);
#22589=ORIENTED_EDGE('',*,*,#15805,.F.);
#22590=ORIENTED_EDGE('',*,*,#15840,.F.);
#22591=ORIENTED_EDGE('',*,*,#15841,.T.);
#22592=ORIENTED_EDGE('',*,*,#15842,.T.);
#22593=ORIENTED_EDGE('',*,*,#15841,.F.);
#22594=ORIENTED_EDGE('',*,*,#15843,.F.);
#22595=ORIENTED_EDGE('',*,*,#15844,.T.);
#22596=ORIENTED_EDGE('',*,*,#15845,.T.);
#22597=ORIENTED_EDGE('',*,*,#15844,.F.);
#22598=ORIENTED_EDGE('',*,*,#15840,.T.);
#22599=ORIENTED_EDGE('',*,*,#15845,.F.);
#22600=ORIENTED_EDGE('',*,*,#15842,.F.);
#22601=ORIENTED_EDGE('',*,*,#15843,.T.);
#22602=ORIENTED_EDGE('',*,*,#15846,.T.);
#22603=ORIENTED_EDGE('',*,*,#15847,.F.);
#22604=ORIENTED_EDGE('',*,*,#15848,.F.);
#22605=ORIENTED_EDGE('',*,*,#15849,.T.);
#22606=ORIENTED_EDGE('',*,*,#15850,.F.);
#22607=ORIENTED_EDGE('',*,*,#15851,.F.);
#22608=ORIENTED_EDGE('',*,*,#15852,.T.);
#22609=ORIENTED_EDGE('',*,*,#15853,.T.);
#22610=ORIENTED_EDGE('',*,*,#15848,.T.);
#22611=ORIENTED_EDGE('',*,*,#15854,.T.);
#22612=ORIENTED_EDGE('',*,*,#15852,.F.);
#22613=ORIENTED_EDGE('',*,*,#15855,.T.);
#22614=ORIENTED_EDGE('',*,*,#15850,.T.);
#22615=ORIENTED_EDGE('',*,*,#15856,.F.);
#22616=ORIENTED_EDGE('',*,*,#15846,.F.);
#22617=ORIENTED_EDGE('',*,*,#15857,.F.);
#22618=ORIENTED_EDGE('',*,*,#15857,.T.);
#22619=ORIENTED_EDGE('',*,*,#15849,.F.);
#22620=ORIENTED_EDGE('',*,*,#15855,.F.);
#22621=ORIENTED_EDGE('',*,*,#15851,.T.);
#22622=ORIENTED_EDGE('',*,*,#15856,.T.);
#22623=ORIENTED_EDGE('',*,*,#15853,.F.);
#22624=ORIENTED_EDGE('',*,*,#15854,.F.);
#22625=ORIENTED_EDGE('',*,*,#15847,.T.);
#22626=ORIENTED_EDGE('',*,*,#15858,.F.);
#22627=ORIENTED_EDGE('',*,*,#15859,.T.);
#22628=ORIENTED_EDGE('',*,*,#15860,.T.);
#22629=ORIENTED_EDGE('',*,*,#15859,.F.);
#22630=ORIENTED_EDGE('',*,*,#15860,.F.);
#22631=ORIENTED_EDGE('',*,*,#15861,.T.);
#22632=ORIENTED_EDGE('',*,*,#15862,.T.);
#22633=ORIENTED_EDGE('',*,*,#15861,.F.);
#22634=ORIENTED_EDGE('',*,*,#15863,.T.);
#22635=ORIENTED_EDGE('',*,*,#15864,.T.);
#22636=ORIENTED_EDGE('',*,*,#15865,.F.);
#22637=ORIENTED_EDGE('',*,*,#15864,.F.);
#22638=ORIENTED_EDGE('',*,*,#15866,.T.);
#22639=ORIENTED_EDGE('',*,*,#15863,.F.);
#22640=ORIENTED_EDGE('',*,*,#15867,.T.);
#22641=ORIENTED_EDGE('',*,*,#15868,.T.);
#22642=ORIENTED_EDGE('',*,*,#15867,.F.);
#22643=ORIENTED_EDGE('',*,*,#15866,.F.);
#22644=ORIENTED_EDGE('',*,*,#15865,.T.);
#22645=ORIENTED_EDGE('',*,*,#15862,.F.);
#22646=ORIENTED_EDGE('',*,*,#15869,.F.);
#22647=ORIENTED_EDGE('',*,*,#15870,.F.);
#22648=ORIENTED_EDGE('',*,*,#15871,.F.);
#22649=ORIENTED_EDGE('',*,*,#15872,.F.);
#22650=ORIENTED_EDGE('',*,*,#15873,.F.);
#22651=ORIENTED_EDGE('',*,*,#15874,.F.);
#22652=ORIENTED_EDGE('',*,*,#15858,.T.);
#22653=ORIENTED_EDGE('',*,*,#15868,.F.);
#22654=ORIENTED_EDGE('',*,*,#15869,.T.);
#22655=ORIENTED_EDGE('',*,*,#15875,.F.);
#22656=ORIENTED_EDGE('',*,*,#15876,.F.);
#22657=ORIENTED_EDGE('',*,*,#15877,.T.);
#22658=ORIENTED_EDGE('',*,*,#15870,.T.);
#22659=ORIENTED_EDGE('',*,*,#15877,.F.);
#22660=ORIENTED_EDGE('',*,*,#15878,.F.);
#22661=ORIENTED_EDGE('',*,*,#15879,.T.);
#22662=ORIENTED_EDGE('',*,*,#15871,.T.);
#22663=ORIENTED_EDGE('',*,*,#15879,.F.);
#22664=ORIENTED_EDGE('',*,*,#15880,.F.);
#22665=ORIENTED_EDGE('',*,*,#15881,.T.);
#22666=ORIENTED_EDGE('',*,*,#15872,.T.);
#22667=ORIENTED_EDGE('',*,*,#15881,.F.);
#22668=ORIENTED_EDGE('',*,*,#15882,.F.);
#22669=ORIENTED_EDGE('',*,*,#15883,.T.);
#22670=ORIENTED_EDGE('',*,*,#15873,.T.);
#22671=ORIENTED_EDGE('',*,*,#15883,.F.);
#22672=ORIENTED_EDGE('',*,*,#15884,.F.);
#22673=ORIENTED_EDGE('',*,*,#15885,.T.);
#22674=ORIENTED_EDGE('',*,*,#15874,.T.);
#22675=ORIENTED_EDGE('',*,*,#15885,.F.);
#22676=ORIENTED_EDGE('',*,*,#15886,.F.);
#22677=ORIENTED_EDGE('',*,*,#15875,.T.);
#22678=ORIENTED_EDGE('',*,*,#15876,.T.);
#22679=ORIENTED_EDGE('',*,*,#15886,.T.);
#22680=ORIENTED_EDGE('',*,*,#15884,.T.);
#22681=ORIENTED_EDGE('',*,*,#15882,.T.);
#22682=ORIENTED_EDGE('',*,*,#15880,.T.);
#22683=ORIENTED_EDGE('',*,*,#15878,.T.);
#22684=ORIENTED_EDGE('',*,*,#15887,.F.);
#22685=ORIENTED_EDGE('',*,*,#15888,.T.);
#22686=ORIENTED_EDGE('',*,*,#15889,.T.);
#22687=ORIENTED_EDGE('',*,*,#15888,.F.);
#22688=ORIENTED_EDGE('',*,*,#15889,.F.);
#22689=ORIENTED_EDGE('',*,*,#15890,.T.);
#22690=ORIENTED_EDGE('',*,*,#15891,.T.);
#22691=ORIENTED_EDGE('',*,*,#15890,.F.);
#22692=ORIENTED_EDGE('',*,*,#15892,.T.);
#22693=ORIENTED_EDGE('',*,*,#15893,.T.);
#22694=ORIENTED_EDGE('',*,*,#15894,.F.);
#22695=ORIENTED_EDGE('',*,*,#15893,.F.);
#22696=ORIENTED_EDGE('',*,*,#15895,.T.);
#22697=ORIENTED_EDGE('',*,*,#15892,.F.);
#22698=ORIENTED_EDGE('',*,*,#15896,.T.);
#22699=ORIENTED_EDGE('',*,*,#15897,.T.);
#22700=ORIENTED_EDGE('',*,*,#15896,.F.);
#22701=ORIENTED_EDGE('',*,*,#15895,.F.);
#22702=ORIENTED_EDGE('',*,*,#15894,.T.);
#22703=ORIENTED_EDGE('',*,*,#15891,.F.);
#22704=ORIENTED_EDGE('',*,*,#15898,.F.);
#22705=ORIENTED_EDGE('',*,*,#15899,.F.);
#22706=ORIENTED_EDGE('',*,*,#15900,.F.);
#22707=ORIENTED_EDGE('',*,*,#15901,.F.);
#22708=ORIENTED_EDGE('',*,*,#15902,.F.);
#22709=ORIENTED_EDGE('',*,*,#15903,.F.);
#22710=ORIENTED_EDGE('',*,*,#15887,.T.);
#22711=ORIENTED_EDGE('',*,*,#15897,.F.);
#22712=ORIENTED_EDGE('',*,*,#15898,.T.);
#22713=ORIENTED_EDGE('',*,*,#15904,.F.);
#22714=ORIENTED_EDGE('',*,*,#15905,.F.);
#22715=ORIENTED_EDGE('',*,*,#15906,.T.);
#22716=ORIENTED_EDGE('',*,*,#15899,.T.);
#22717=ORIENTED_EDGE('',*,*,#15906,.F.);
#22718=ORIENTED_EDGE('',*,*,#15907,.F.);
#22719=ORIENTED_EDGE('',*,*,#15908,.T.);
#22720=ORIENTED_EDGE('',*,*,#15900,.T.);
#22721=ORIENTED_EDGE('',*,*,#15908,.F.);
#22722=ORIENTED_EDGE('',*,*,#15909,.F.);
#22723=ORIENTED_EDGE('',*,*,#15910,.T.);
#22724=ORIENTED_EDGE('',*,*,#15901,.T.);
#22725=ORIENTED_EDGE('',*,*,#15910,.F.);
#22726=ORIENTED_EDGE('',*,*,#15911,.F.);
#22727=ORIENTED_EDGE('',*,*,#15912,.T.);
#22728=ORIENTED_EDGE('',*,*,#15902,.T.);
#22729=ORIENTED_EDGE('',*,*,#15912,.F.);
#22730=ORIENTED_EDGE('',*,*,#15913,.F.);
#22731=ORIENTED_EDGE('',*,*,#15914,.T.);
#22732=ORIENTED_EDGE('',*,*,#15903,.T.);
#22733=ORIENTED_EDGE('',*,*,#15914,.F.);
#22734=ORIENTED_EDGE('',*,*,#15915,.F.);
#22735=ORIENTED_EDGE('',*,*,#15904,.T.);
#22736=ORIENTED_EDGE('',*,*,#15905,.T.);
#22737=ORIENTED_EDGE('',*,*,#15915,.T.);
#22738=ORIENTED_EDGE('',*,*,#15913,.T.);
#22739=ORIENTED_EDGE('',*,*,#15911,.T.);
#22740=ORIENTED_EDGE('',*,*,#15909,.T.);
#22741=ORIENTED_EDGE('',*,*,#15907,.T.);
#22742=CYLINDRICAL_SURFACE('',#24885,3.);
#22743=CYLINDRICAL_SURFACE('',#24888,3.);
#22744=CYLINDRICAL_SURFACE('',#24891,3.);
#22745=CYLINDRICAL_SURFACE('',#24894,3.);
#22746=CYLINDRICAL_SURFACE('',#24897,3.4);
#22747=CYLINDRICAL_SURFACE('',#24900,3.4);
#22748=CYLINDRICAL_SURFACE('',#24903,3.4);
#22749=CYLINDRICAL_SURFACE('',#24906,3.4);
#22750=CYLINDRICAL_SURFACE('',#24909,3.);
#22751=CYLINDRICAL_SURFACE('',#24913,3.);
#22752=CYLINDRICAL_SURFACE('',#24917,2.49999999999999);
#22753=CYLINDRICAL_SURFACE('',#24921,2.49999999999999);
#22754=CYLINDRICAL_SURFACE('',#24938,5.00000000000009);
#22755=CYLINDRICAL_SURFACE('',#24948,6.00000000000005);
#22756=CYLINDRICAL_SURFACE('',#24956,7.50000000000004);
#22757=CYLINDRICAL_SURFACE('',#24965,5.);
#22758=CYLINDRICAL_SURFACE('',#24967,4.8);
#22759=CYLINDRICAL_SURFACE('',#24970,5.);
#22760=CYLINDRICAL_SURFACE('',#24989,1.5);
#22761=CYLINDRICAL_SURFACE('',#24991,2.45849999999999);
#22762=CYLINDRICAL_SURFACE('',#24992,2.74999999999999);
#22763=CYLINDRICAL_SURFACE('',#24995,2.74999999999999);
#22764=CYLINDRICAL_SURFACE('',#24998,2.74999999999999);
#22765=CYLINDRICAL_SURFACE('',#25001,2.74999999999999);
#22766=CYLINDRICAL_SURFACE('',#25004,2.74999999999999);
#22767=CYLINDRICAL_SURFACE('',#25007,2.74999999999999);
#22768=CYLINDRICAL_SURFACE('',#25010,14.);
#22769=CYLINDRICAL_SURFACE('',#25013,11.);
#22770=CYLINDRICAL_SURFACE('',#25016,10.75);
#22771=CYLINDRICAL_SURFACE('',#25019,7.5);
#22772=CYLINDRICAL_SURFACE('',#25022,10.75);
#22773=CYLINDRICAL_SURFACE('',#25025,11.);
#22774=CYLINDRICAL_SURFACE('',#25038,24.);
#22775=CYLINDRICAL_SURFACE('',#25040,24.);
#22776=CYLINDRICAL_SURFACE('',#25058,4.49999999999999);
#22777=CYLINDRICAL_SURFACE('',#25061,4.49999999999999);
#22778=CYLINDRICAL_SURFACE('',#25064,12.);
#22779=CYLINDRICAL_SURFACE('',#25067,7.75);
#22780=CYLINDRICAL_SURFACE('',#25070,6.00000000000001);
#22781=CYLINDRICAL_SURFACE('',#25073,7.74999999999999);
#22782=CYLINDRICAL_SURFACE('',#25076,12.);
#22783=CYLINDRICAL_SURFACE('',#25107,3.1);
#22784=CYLINDRICAL_SURFACE('',#25110,3.1);
#22785=CYLINDRICAL_SURFACE('',#25113,3.1);
#22786=CYLINDRICAL_SURFACE('',#25116,3.1);
#22787=CYLINDRICAL_SURFACE('',#25119,3.5);
#22788=CYLINDRICAL_SURFACE('',#25122,3.5);
#22789=CYLINDRICAL_SURFACE('',#25125,3.50000000000001);
#22790=CYLINDRICAL_SURFACE('',#25128,3.50000000000001);
#22791=CYLINDRICAL_SURFACE('',#25215,1.621);
#22792=CYLINDRICAL_SURFACE('',#25223,5.4585);
#22793=CYLINDRICAL_SURFACE('',#25224,11.);
#22794=CYLINDRICAL_SURFACE('',#25227,8.5);
#22795=CYLINDRICAL_SURFACE('',#25230,11.);
#22796=CYLINDRICAL_SURFACE('',#25233,11.);
#22797=CYLINDRICAL_SURFACE('',#25236,11.);
#22798=CYLINDRICAL_SURFACE('',#25253,2.);
#22799=CYLINDRICAL_SURFACE('',#25264,7.75);
#22800=CYLINDRICAL_SURFACE('',#25267,6.);
#22801=CYLINDRICAL_SURFACE('',#25278,4.49999999999999);
#22802=CYLINDRICAL_SURFACE('',#25281,4.49999999999999);
#22803=CYLINDRICAL_SURFACE('',#25284,13.);
#22804=CYLINDRICAL_SURFACE('',#25305,5.);
#22805=CYLINDRICAL_SURFACE('',#25310,6.7);
#22806=CYLINDRICAL_SURFACE('',#25313,9.8);
#22807=CYLINDRICAL_SURFACE('',#25320,13.);
#22808=CYLINDRICAL_SURFACE('',#25325,9.8);
#22809=CYLINDRICAL_SURFACE('',#25328,6.69999999999999);
#22810=CYLINDRICAL_SURFACE('',#25338,0.6);
#22811=CYLINDRICAL_SURFACE('',#25341,0.6);
#22812=CYLINDRICAL_SURFACE('',#25344,4.8);
#22813=CYLINDRICAL_SURFACE('',#25347,6.15);
#22814=CYLINDRICAL_SURFACE('',#25361,1.6);
#22815=CYLINDRICAL_SURFACE('',#25363,1.6);
#22816=CYLINDRICAL_SURFACE('',#25364,1.6);
#22817=CYLINDRICAL_SURFACE('',#25366,1.6);
#22818=CYLINDRICAL_SURFACE('',#25373,3.);
#22819=CYLINDRICAL_SURFACE('',#25376,3.);
#22820=CYLINDRICAL_SURFACE('',#25379,4.25000000000001);
#22821=CYLINDRICAL_SURFACE('',#25382,4.25000000000001);
#22822=CYLINDRICAL_SURFACE('',#25398,3.);
#22823=CYLINDRICAL_SURFACE('',#25401,3.);
#22824=CYLINDRICAL_SURFACE('',#25404,4.25000000000001);
#22825=CYLINDRICAL_SURFACE('',#25407,4.25000000000001);
#22826=CYLINDRICAL_SURFACE('',#25423,1.65);
#22827=CYLINDRICAL_SURFACE('',#25426,1.65);
#22828=CYLINDRICAL_SURFACE('',#25429,1.65);
#22829=CYLINDRICAL_SURFACE('',#25432,1.65);
#22830=CYLINDRICAL_SURFACE('',#25435,3.);
#22831=CYLINDRICAL_SURFACE('',#25438,3.);
#22832=CYLINDRICAL_SURFACE('',#25441,5.5);
#22833=CYLINDRICAL_SURFACE('',#25444,3.3);
#22834=CYLINDRICAL_SURFACE('',#25447,5.5);
#22835=CYLINDRICAL_SURFACE('',#25450,3.3);
#22836=CYLINDRICAL_SURFACE('',#25453,10.);
#22837=CYLINDRICAL_SURFACE('',#25456,25.);
#22838=CYLINDRICAL_SURFACE('',#25473,1.5);
#22839=CYLINDRICAL_SURFACE('',#25475,9.);
#22840=CYLINDRICAL_SURFACE('',#25480,1.5);
#22841=CYLINDRICAL_SURFACE('',#25626,1.5);
#22842=CYLINDRICAL_SURFACE('',#25630,1.5);
#22843=CYLINDRICAL_SURFACE('',#25637,1.5);
#22844=CYLINDRICAL_SURFACE('',#25641,1.5);
#22845=CYLINDRICAL_SURFACE('',#25649,2.5);
#22846=CYLINDRICAL_SURFACE('',#25668,20.);
#22847=CYLINDRICAL_SURFACE('',#25680,11.5);
#22848=CYLINDRICAL_SURFACE('',#25682,12.);
#22849=CYLINDRICAL_SURFACE('',#25684,12.);
#22850=CYLINDRICAL_SURFACE('',#25686,12.);
#22851=CYLINDRICAL_SURFACE('',#25688,11.5);
#22852=CYLINDRICAL_SURFACE('',#25690,11.5);
#22853=CYLINDRICAL_SURFACE('',#25701,11.5);
#22854=CYLINDRICAL_SURFACE('',#25702,11.5);
#22855=CYLINDRICAL_SURFACE('',#25703,11.5);
#22856=CYLINDRICAL_SURFACE('',#25704,7.);
#22857=CYLINDRICAL_SURFACE('',#25709,2.1);
#22858=CYLINDRICAL_SURFACE('',#25710,20.);
#22859=CYLINDRICAL_SURFACE('',#25734,19.5);
#22860=CYLINDRICAL_SURFACE('',#25765,19.5);
#22861=CYLINDRICAL_SURFACE('',#25766,19.5);
#22862=CYLINDRICAL_SURFACE('',#25787,19.5);
#22863=CYLINDRICAL_SURFACE('',#25793,1.4361111111);
#22864=CYLINDRICAL_SURFACE('',#25804,0.4033333333);
#22865=CYLINDRICAL_SURFACE('',#25806,19.5);
#22866=CYLINDRICAL_SURFACE('',#25812,2.5);
#22867=CYLINDRICAL_SURFACE('',#25831,20.);
#22868=CYLINDRICAL_SURFACE('',#25843,11.5);
#22869=CYLINDRICAL_SURFACE('',#25845,12.);
#22870=CYLINDRICAL_SURFACE('',#25847,12.);
#22871=CYLINDRICAL_SURFACE('',#25849,12.);
#22872=CYLINDRICAL_SURFACE('',#25851,11.5);
#22873=CYLINDRICAL_SURFACE('',#25853,11.5);
#22874=CYLINDRICAL_SURFACE('',#25864,11.5);
#22875=CYLINDRICAL_SURFACE('',#25865,11.5);
#22876=CYLINDRICAL_SURFACE('',#25866,11.5);
#22877=CYLINDRICAL_SURFACE('',#25867,5.);
#22878=CYLINDRICAL_SURFACE('',#25877,2.1);
#22879=CYLINDRICAL_SURFACE('',#25878,20.);
#22880=CYLINDRICAL_SURFACE('',#25902,19.5);
#22881=CYLINDRICAL_SURFACE('',#25933,19.5);
#22882=CYLINDRICAL_SURFACE('',#25934,19.5);
#22883=CYLINDRICAL_SURFACE('',#25955,19.5);
#22884=CYLINDRICAL_SURFACE('',#25961,1.4361111111);
#22885=CYLINDRICAL_SURFACE('',#25972,0.4033333333);
#22886=CYLINDRICAL_SURFACE('',#25974,19.5);
#22887=CYLINDRICAL_SURFACE('',#25983,2.1);
#22888=CYLINDRICAL_SURFACE('',#25986,2.1);
#22889=CYLINDRICAL_SURFACE('',#25989,2.1);
#22890=CYLINDRICAL_SURFACE('',#25992,2.1);
#22891=CYLINDRICAL_SURFACE('',#25995,2.1);
#22892=CYLINDRICAL_SURFACE('',#25998,2.1);
#22893=CYLINDRICAL_SURFACE('',#26001,14.);
#22894=CYLINDRICAL_SURFACE('',#26014,10.);
#22895=CYLINDRICAL_SURFACE('',#26015,10.);
#22896=CYLINDRICAL_SURFACE('',#26017,2.99999999999999);
#22897=CYLINDRICAL_SURFACE('',#26020,2.99999999999999);
#22898=CYLINDRICAL_SURFACE('',#26023,3.3);
#22899=CYLINDRICAL_SURFACE('',#26026,3.3);
#22900=CYLINDRICAL_SURFACE('',#26029,3.3);
#22901=CYLINDRICAL_SURFACE('',#26032,3.3);
#22902=CYLINDRICAL_SURFACE('',#26044,3.3);
#22903=CYLINDRICAL_SURFACE('',#26047,3.3);
#22904=CYLINDRICAL_SURFACE('',#26050,3.3);
#22905=CYLINDRICAL_SURFACE('',#26053,3.3);
#22906=CYLINDRICAL_SURFACE('',#26056,3.3);
#22907=CYLINDRICAL_SURFACE('',#26059,3.3);
#22908=CYLINDRICAL_SURFACE('',#26083,55.);
#22909=CYLINDRICAL_SURFACE('',#26086,3.39999999999999);
#22910=CYLINDRICAL_SURFACE('',#26089,3.4);
#22911=CYLINDRICAL_SURFACE('',#26092,3.4);
#22912=CYLINDRICAL_SURFACE('',#26095,3.39999999999999);
#22913=CYLINDRICAL_SURFACE('',#26098,4.24999999999998);
#22914=CYLINDRICAL_SURFACE('',#26101,4.24999999999998);
#22915=CYLINDRICAL_SURFACE('',#26104,4.24999999999998);
#22916=CYLINDRICAL_SURFACE('',#26107,4.24999999999998);
#22917=CYLINDRICAL_SURFACE('',#26110,45.);
#22918=CYLINDRICAL_SURFACE('',#26113,65.);
#22919=CYLINDRICAL_SURFACE('',#26116,2.99999999999999);
#22920=CYLINDRICAL_SURFACE('',#26119,2.99999999999999);
#22921=CYLINDRICAL_SURFACE('',#26122,2.5);
#22922=CYLINDRICAL_SURFACE('',#26125,2.5);
#22923=CYLINDRICAL_SURFACE('',#26128,2.5);
#22924=CYLINDRICAL_SURFACE('',#26131,2.5);
#22925=CYLINDRICAL_SURFACE('',#26134,5.50000000000001);
#22926=CYLINDRICAL_SURFACE('',#26137,3.30000000000004);
#22927=CYLINDRICAL_SURFACE('',#26140,5.50000000000001);
#22928=CYLINDRICAL_SURFACE('',#26143,3.30000000000004);
#22929=CYLINDRICAL_SURFACE('',#26146,5.50000000000001);
#22930=CYLINDRICAL_SURFACE('',#26149,3.30000000000004);
#22931=CYLINDRICAL_SURFACE('',#26152,5.50000000000001);
#22932=CYLINDRICAL_SURFACE('',#26155,3.30000000000004);
#22933=CYLINDRICAL_SURFACE('',#26158,5.50000000000001);
#22934=CYLINDRICAL_SURFACE('',#26161,3.30000000000004);
#22935=CYLINDRICAL_SURFACE('',#26164,5.50000000000001);
#22936=CYLINDRICAL_SURFACE('',#26167,3.30000000000004);
#22937=CYLINDRICAL_SURFACE('',#26170,5.49999999999999);
#22938=CYLINDRICAL_SURFACE('',#26173,3.30000000000004);
#22939=CYLINDRICAL_SURFACE('',#26176,5.50000000000001);
#22940=CYLINDRICAL_SURFACE('',#26179,3.30000000000004);
#22941=CYLINDRICAL_SURFACE('',#26182,5.50000000000001);
#22942=CYLINDRICAL_SURFACE('',#26185,3.30000000000004);
#22943=CYLINDRICAL_SURFACE('',#26188,5.50000000000001);
#22944=CYLINDRICAL_SURFACE('',#26191,3.30000000000004);
#22945=CYLINDRICAL_SURFACE('',#26194,5.50000000000001);
#22946=CYLINDRICAL_SURFACE('',#26197,3.30000000000004);
#22947=CYLINDRICAL_SURFACE('',#26200,5.50000000000001);
#22948=CYLINDRICAL_SURFACE('',#26203,3.30000000000004);
#22949=CYLINDRICAL_SURFACE('',#26206,5.50000000000001);
#22950=CYLINDRICAL_SURFACE('',#26209,3.30000000000004);
#22951=CYLINDRICAL_SURFACE('',#26212,5.50000000000001);
#22952=CYLINDRICAL_SURFACE('',#26215,3.30000000000004);
#22953=CYLINDRICAL_SURFACE('',#26218,5.49999999999999);
#22954=CYLINDRICAL_SURFACE('',#26221,3.30000000000004);
#22955=CYLINDRICAL_SURFACE('',#26224,5.50000000000001);
#22956=CYLINDRICAL_SURFACE('',#26227,3.30000000000004);
#22957=CYLINDRICAL_SURFACE('',#26264,55.);
#22958=CYLINDRICAL_SURFACE('',#26271,5.50000000000001);
#22959=CYLINDRICAL_SURFACE('',#26274,3.5);
#22960=CYLINDRICAL_SURFACE('',#26285,5.50000000000001);
#22961=CYLINDRICAL_SURFACE('',#26288,3.5);
#22962=CYLINDRICAL_SURFACE('',#26299,5.50000000000001);
#22963=CYLINDRICAL_SURFACE('',#26302,3.5);
#22964=CYLINDRICAL_SURFACE('',#26313,5.50000000000001);
#22965=CYLINDRICAL_SURFACE('',#26316,3.5);
#22966=CYLINDRICAL_SURFACE('',#26327,5.50000000000001);
#22967=CYLINDRICAL_SURFACE('',#26330,3.5);
#22968=CYLINDRICAL_SURFACE('',#26341,5.50000000000001);
#22969=CYLINDRICAL_SURFACE('',#26344,3.5);
#22970=CYLINDRICAL_SURFACE('',#26355,5.5);
#22971=CYLINDRICAL_SURFACE('',#26358,3.5);
#22972=CYLINDRICAL_SURFACE('',#26369,5.5);
#22973=CYLINDRICAL_SURFACE('',#26372,3.5);
#22974=CYLINDRICAL_SURFACE('',#26469,2.3);
#22975=CYLINDRICAL_SURFACE('',#26470,2.3);
#22976=CYLINDRICAL_SURFACE('',#26471,0.5);
#22977=CYLINDRICAL_SURFACE('',#26472,0.5);
#22978=CYLINDRICAL_SURFACE('',#26473,0.5);
#22979=CYLINDRICAL_SURFACE('',#26474,0.5);
#22980=CYLINDRICAL_SURFACE('',#26475,0.5);
#22981=CYLINDRICAL_SURFACE('',#26476,0.5);
#22982=CYLINDRICAL_SURFACE('',#26477,0.5);
#22983=CYLINDRICAL_SURFACE('',#26478,0.5);
#22984=CYLINDRICAL_SURFACE('',#26479,0.999999999999999);
#22985=CYLINDRICAL_SURFACE('',#26485,2.3);
#22986=CYLINDRICAL_SURFACE('',#26486,2.3);
#22987=CYLINDRICAL_SURFACE('',#26487,0.5);
#22988=CYLINDRICAL_SURFACE('',#26488,0.5);
#22989=CYLINDRICAL_SURFACE('',#26489,0.5);
#22990=CYLINDRICAL_SURFACE('',#26490,0.5);
#22991=CYLINDRICAL_SURFACE('',#26491,0.5);
#22992=CYLINDRICAL_SURFACE('',#26492,0.5);
#22993=CYLINDRICAL_SURFACE('',#26493,0.5);
#22994=CYLINDRICAL_SURFACE('',#26494,0.5);
#22995=CYLINDRICAL_SURFACE('',#26495,0.999999999999999);
#22996=CYLINDRICAL_SURFACE('',#26508,2.5);
#22997=CYLINDRICAL_SURFACE('',#26511,2.5);
#22998=CYLINDRICAL_SURFACE('',#26514,3.65);
#22999=CYLINDRICAL_SURFACE('',#26519,3.32349999999999);
#23000=CYLINDRICAL_SURFACE('',#26522,3.3235);
#23001=CYLINDRICAL_SURFACE('',#26525,3.32349999999999);
#23002=CYLINDRICAL_SURFACE('',#26528,3.3235);
#23003=CYLINDRICAL_SURFACE('',#26531,2.5);
#23004=CYLINDRICAL_SURFACE('',#26534,2.5);
#23005=CYLINDRICAL_SURFACE('',#26537,3.65);
#23006=CYLINDRICAL_SURFACE('',#26540,0.500000000000006);
#23007=CYLINDRICAL_SURFACE('',#26546,0.5);
#23008=CYLINDRICAL_SURFACE('',#26552,4.);
#23009=CYLINDRICAL_SURFACE('',#26554,4.99995);
#23010=CYLINDRICAL_SURFACE('',#26584,2.3);
#23011=CYLINDRICAL_SURFACE('',#26587,2.3);
#23012=CYLINDRICAL_SURFACE('',#26590,2.3);
#23013=CYLINDRICAL_SURFACE('',#26593,2.3);
#23014=CYLINDRICAL_SURFACE('',#26596,0.5);
#23015=CYLINDRICAL_SURFACE('',#26599,0.5);
#23016=CYLINDRICAL_SURFACE('',#26602,0.5);
#23017=CYLINDRICAL_SURFACE('',#26605,0.5);
#23018=CYLINDRICAL_SURFACE('',#26608,0.5);
#23019=CYLINDRICAL_SURFACE('',#26611,0.5);
#23020=CYLINDRICAL_SURFACE('',#26614,0.5);
#23021=CYLINDRICAL_SURFACE('',#26617,0.5);
#23022=CYLINDRICAL_SURFACE('',#26620,0.5);
#23023=CYLINDRICAL_SURFACE('',#26623,0.5);
#23024=CYLINDRICAL_SURFACE('',#26626,0.5);
#23025=CYLINDRICAL_SURFACE('',#26629,0.5);
#23026=CYLINDRICAL_SURFACE('',#26632,0.5);
#23027=CYLINDRICAL_SURFACE('',#26635,0.5);
#23028=CYLINDRICAL_SURFACE('',#26638,0.5);
#23029=CYLINDRICAL_SURFACE('',#26641,0.5);
#23030=CYLINDRICAL_SURFACE('',#26682,0.450000000000001);
#23031=CYLINDRICAL_SURFACE('',#26685,0.450000000000001);
#23032=CYLINDRICAL_SURFACE('',#26688,0.55);
#23033=CYLINDRICAL_SURFACE('',#26690,2.25);
#23034=CYLINDRICAL_SURFACE('',#26692,0.549999999999998);
#23035=CYLINDRICAL_SURFACE('',#26695,0.55);
#23036=CYLINDRICAL_SURFACE('',#26698,0.55);
#23037=CYLINDRICAL_SURFACE('',#26701,0.55);
#23038=CYLINDRICAL_SURFACE('',#26703,2.25);
#23039=CYLINDRICAL_SURFACE('',#26705,0.55);
#23040=CYLINDRICAL_SURFACE('',#26710,0.550000000000001);
#23041=CYLINDRICAL_SURFACE('',#26712,2.25);
#23042=CYLINDRICAL_SURFACE('',#26714,0.550000000000002);
#23043=CYLINDRICAL_SURFACE('',#26717,0.55);
#23044=CYLINDRICAL_SURFACE('',#26720,0.55);
#23045=CYLINDRICAL_SURFACE('',#26723,0.55);
#23046=CYLINDRICAL_SURFACE('',#26725,2.25);
#23047=CYLINDRICAL_SURFACE('',#26727,0.55);
#23048=CYLINDRICAL_SURFACE('',#26730,0.450000000000001);
#23049=CYLINDRICAL_SURFACE('',#26733,0.450000000000001);
#23050=CYLINDRICAL_SURFACE('',#26772,0.5);
#23051=CYLINDRICAL_SURFACE('',#26787,0.5);
#23052=CYLINDRICAL_SURFACE('',#26790,0.5);
#23053=CYLINDRICAL_SURFACE('',#26793,0.5);
#23054=CYLINDRICAL_SURFACE('',#26795,2.3);
#23055=CYLINDRICAL_SURFACE('',#26797,0.5);
#23056=CYLINDRICAL_SURFACE('',#26800,0.5);
#23057=CYLINDRICAL_SURFACE('',#26803,0.5);
#23058=CYLINDRICAL_SURFACE('',#26806,0.5);
#23059=CYLINDRICAL_SURFACE('',#26808,2.3);
#23060=CYLINDRICAL_SURFACE('',#26810,0.5);
#23061=CYLINDRICAL_SURFACE('',#26815,0.5);
#23062=CYLINDRICAL_SURFACE('',#26817,2.3);
#23063=CYLINDRICAL_SURFACE('',#26819,0.5);
#23064=CYLINDRICAL_SURFACE('',#26822,0.5);
#23065=CYLINDRICAL_SURFACE('',#26825,0.5);
#23066=CYLINDRICAL_SURFACE('',#26828,0.5);
#23067=CYLINDRICAL_SURFACE('',#26830,2.3);
#23068=CYLINDRICAL_SURFACE('',#26832,0.5);
#23069=CYLINDRICAL_SURFACE('',#26835,0.5);
#23070=CYLINDRICAL_SURFACE('',#26838,0.5);
#23071=CYLINDRICAL_SURFACE('',#26846,0.500000000000006);
#23072=CYLINDRICAL_SURFACE('',#26848,2.);
#23073=CYLINDRICAL_SURFACE('',#26856,2.);
#23074=CYLINDRICAL_SURFACE('',#26912,0.450000000000001);
#23075=CYLINDRICAL_SURFACE('',#26915,0.450000000000001);
#23076=CYLINDRICAL_SURFACE('',#26918,0.55);
#23077=CYLINDRICAL_SURFACE('',#26920,2.25);
#23078=CYLINDRICAL_SURFACE('',#26922,0.55);
#23079=CYLINDRICAL_SURFACE('',#26925,0.55);
#23080=CYLINDRICAL_SURFACE('',#26928,0.55);
#23081=CYLINDRICAL_SURFACE('',#26931,0.550000000000002);
#23082=CYLINDRICAL_SURFACE('',#26933,2.25);
#23083=CYLINDRICAL_SURFACE('',#26935,0.55);
#23084=CYLINDRICAL_SURFACE('',#26940,0.55);
#23085=CYLINDRICAL_SURFACE('',#26942,2.25);
#23086=CYLINDRICAL_SURFACE('',#26944,0.55);
#23087=CYLINDRICAL_SURFACE('',#26947,0.55);
#23088=CYLINDRICAL_SURFACE('',#26950,0.55);
#23089=CYLINDRICAL_SURFACE('',#26953,0.549999999999998);
#23090=CYLINDRICAL_SURFACE('',#26955,2.25);
#23091=CYLINDRICAL_SURFACE('',#26957,0.550000000000001);
#23092=CYLINDRICAL_SURFACE('',#26960,0.450000000000001);
#23093=CYLINDRICAL_SURFACE('',#26963,0.450000000000001);
#23094=CYLINDRICAL_SURFACE('',#27034,0.5);
#23095=CYLINDRICAL_SURFACE('',#27036,0.5);
#23096=CYLINDRICAL_SURFACE('',#27041,0.5);
#23097=CYLINDRICAL_SURFACE('',#27043,0.5);
#23098=CYLINDRICAL_SURFACE('',#27045,2.3);
#23099=CYLINDRICAL_SURFACE('',#27047,0.5);
#23100=CYLINDRICAL_SURFACE('',#27049,0.5);
#23101=CYLINDRICAL_SURFACE('',#27053,0.5);
#23102=CYLINDRICAL_SURFACE('',#27055,0.5);
#23103=CYLINDRICAL_SURFACE('',#27057,2.3);
#23104=CYLINDRICAL_SURFACE('',#27061,0.5);
#23105=CYLINDRICAL_SURFACE('',#27063,0.5);
#23106=CYLINDRICAL_SURFACE('',#27065,2.3);
#23107=CYLINDRICAL_SURFACE('',#27067,0.5);
#23108=CYLINDRICAL_SURFACE('',#27069,0.5);
#23109=CYLINDRICAL_SURFACE('',#27074,0.5);
#23110=CYLINDRICAL_SURFACE('',#27076,0.5);
#23111=CYLINDRICAL_SURFACE('',#27078,2.3);
#23112=CYLINDRICAL_SURFACE('',#27080,0.5);
#23113=CYLINDRICAL_SURFACE('',#27082,0.5);
#23114=CYLINDRICAL_SURFACE('',#27099,4.99995);
#23115=CYLINDRICAL_SURFACE('',#27103,5.5);
#23116=CYLINDRICAL_SURFACE('',#27104,5.50000000000001);
#23117=CYLINDRICAL_SURFACE('',#27105,5.5);
#23118=CYLINDRICAL_SURFACE('',#27106,5.49999999999999);
#23119=CYLINDRICAL_SURFACE('',#27122,3.);
#23120=CYLINDRICAL_SURFACE('',#27125,4.);
#23121=CYLINDRICAL_SURFACE('',#27190,2.5);
#23122=CYLINDRICAL_SURFACE('',#27194,2.5);
#23123=CYLINDRICAL_SURFACE('',#27198,2.5);
#23124=CYLINDRICAL_SURFACE('',#27202,2.5);
#23125=CYLINDRICAL_SURFACE('',#27206,2.5);
#23126=CYLINDRICAL_SURFACE('',#27210,2.5);
#23127=CYLINDRICAL_SURFACE('',#27214,2.5);
#23128=CYLINDRICAL_SURFACE('',#27218,2.5);
#23129=CYLINDRICAL_SURFACE('',#27236,0.200000000000001);
#23130=CYLINDRICAL_SURFACE('',#27237,0.200000000000001);
#23131=CYLINDRICAL_SURFACE('',#27251,4.25);
#23132=CYLINDRICAL_SURFACE('',#27253,2.065);
#23133=CYLINDRICAL_SURFACE('',#27256,2.5);
#23134=CYLINDRICAL_SURFACE('',#27275,5.);
#23135=CYLINDRICAL_SURFACE('',#27278,2.5);
#23136=CYLINDRICAL_SURFACE('',#27283,4.25);
#23137=CYLINDRICAL_SURFACE('',#27286,2.5);
#23138=CYLINDRICAL_SURFACE('',#27294,5.);
#23139=CYLINDRICAL_SURFACE('',#27303,3.);
#23140=CYLINDRICAL_SURFACE('',#27328,6.5);
#23141=CYLINDRICAL_SURFACE('',#27330,3.3225);
#23142=CYLINDRICAL_SURFACE('',#27333,4.);
#23143=CYLINDRICAL_SURFACE('',#27352,8.);
#23144=CYLINDRICAL_SURFACE('',#27355,4.);
#23145=CYLINDRICAL_SURFACE('',#27360,7.25);
#23146=CYLINDRICAL_SURFACE('',#27363,4.);
#23147=CYLINDRICAL_SURFACE('',#27371,5.);
#23148=CYLINDRICAL_SURFACE('',#27380,3.);
#23149=CYLINDRICAL_SURFACE('',#27393,3.5);
#23150=CYLINDRICAL_SURFACE('',#27402,2.);
#23151=ADVANCED_FACE('',(#2159),#22742,.F.);
#23152=ADVANCED_FACE('',(#2160),#22743,.F.);
#23153=ADVANCED_FACE('',(#2161),#22744,.F.);
#23154=ADVANCED_FACE('',(#2162),#22745,.F.);
#23155=ADVANCED_FACE('',(#2163),#22746,.F.);
#23156=ADVANCED_FACE('',(#2164),#22747,.F.);
#23157=ADVANCED_FACE('',(#2165),#22748,.F.);
#23158=ADVANCED_FACE('',(#2166),#22749,.F.);
#23159=ADVANCED_FACE('',(#2167),#22750,.F.);
#23160=ADVANCED_FACE('',(#2168),#2105,.F.);
#23161=ADVANCED_FACE('',(#2169),#22751,.F.);
#23162=ADVANCED_FACE('',(#2170),#2106,.F.);
#23163=ADVANCED_FACE('',(#2171),#22752,.F.);
#23164=ADVANCED_FACE('',(#2172),#2107,.F.);
#23165=ADVANCED_FACE('',(#2173),#22753,.F.);
#23166=ADVANCED_FACE('',(#2174),#2108,.F.);
#23167=ADVANCED_FACE('',(#2175),#1342,.F.);
#23168=ADVANCED_FACE('',(#2176),#1343,.F.);
#23169=ADVANCED_FACE('',(#2177,#1000,#1001,#1002,#1003),#1344,.F.);
#23170=ADVANCED_FACE('',(#2178),#1345,.F.);
#23171=ADVANCED_FACE('',(#2179),#1346,.F.);
#23172=ADVANCED_FACE('',(#2180,#1004,#1005,#1006,#1007,#1008,#1009,#1010,
#1011),#1347,.F.);
#23173=ADVANCED_FACE('',(#2181,#1012,#1013,#1014,#1015,#1016,#1017,#1018,
#1019),#1348,.T.);
#23174=ADVANCED_FACE('',(#2182),#1349,.F.);
#23175=ADVANCED_FACE('',(#2183),#1350,.F.);
#23176=ADVANCED_FACE('',(#2184),#1351,.F.);
#23177=ADVANCED_FACE('',(#2185),#22754,.T.);
#23178=ADVANCED_FACE('',(#2186),#636,.F.);
#23179=ADVANCED_FACE('',(#2187),#2109,.T.);
#23180=ADVANCED_FACE('',(#2188),#22755,.T.);
#23181=ADVANCED_FACE('',(#2189),#637,.F.);
#23182=ADVANCED_FACE('',(#2190),#2110,.T.);
#23183=ADVANCED_FACE('',(#2191),#22756,.T.);
#23184=ADVANCED_FACE('',(#2192),#2111,.T.);
#23185=ADVANCED_FACE('',(#2193),#638,.F.);
#23186=ADVANCED_FACE('',(#2194),#22757,.T.);
#23187=ADVANCED_FACE('',(#2195),#22758,.T.);
#23188=ADVANCED_FACE('',(#2196),#22759,.T.);
#23189=ADVANCED_FACE('',(#2197),#2112,.T.);
#23190=ADVANCED_FACE('',(#2198,#1020),#1352,.F.);
#23191=ADVANCED_FACE('',(#2199,#1021),#1353,.F.);
#23192=ADVANCED_FACE('',(#2200,#1022),#1354,.F.);
#23193=ADVANCED_FACE('',(#2201,#1023),#1355,.F.);
#23194=ADVANCED_FACE('',(#2202,#1024),#1356,.F.);
#23195=ADVANCED_FACE('',(#2203),#2113,.T.);
#23196=ADVANCED_FACE('',(#2204),#1357,.F.);
#23197=ADVANCED_FACE('',(#2205),#1358,.F.);
#23198=ADVANCED_FACE('',(#2206),#1359,.F.);
#23199=ADVANCED_FACE('',(#2207),#1360,.F.);
#23200=ADVANCED_FACE('',(#2208),#1361,.F.);
#23201=ADVANCED_FACE('',(#2209),#22760,.F.);
#23202=ADVANCED_FACE('',(#2210),#22761,.F.);
#23203=ADVANCED_FACE('',(#2211),#22762,.F.);
#23204=ADVANCED_FACE('',(#2212),#22763,.F.);
#23205=ADVANCED_FACE('',(#2213),#22764,.F.);
#23206=ADVANCED_FACE('',(#2214),#22765,.F.);
#23207=ADVANCED_FACE('',(#2215),#22766,.F.);
#23208=ADVANCED_FACE('',(#2216),#22767,.F.);
#23209=ADVANCED_FACE('',(#2217),#22768,.T.);
#23210=ADVANCED_FACE('',(#2218),#22769,.F.);
#23211=ADVANCED_FACE('',(#2219),#22770,.T.);
#23212=ADVANCED_FACE('',(#2220,#1025),#22771,.F.);
#23213=ADVANCED_FACE('',(#2221),#22772,.T.);
#23214=ADVANCED_FACE('',(#2222),#22773,.F.);
#23215=ADVANCED_FACE('',(#2223),#639,.T.);
#23216=ADVANCED_FACE('',(#2224,#1026,#1027,#1028,#1029,#1030,#1031,#1032),
#1362,.F.);
#23217=ADVANCED_FACE('',(#2225),#640,.T.);
#23218=ADVANCED_FACE('',(#2226),#641,.T.);
#23219=ADVANCED_FACE('',(#2227,#1033),#22774,.T.);
#23220=ADVANCED_FACE('',(#2228),#22775,.T.);
#23221=ADVANCED_FACE('',(#2229),#642,.T.);
#23222=ADVANCED_FACE('',(#2230),#643,.T.);
#23223=ADVANCED_FACE('',(#2231,#1034,#1035,#1036,#1037,#1038,#1039,#1040),
#1363,.F.);
#23224=ADVANCED_FACE('',(#2232,#1041),#1364,.F.);
#23225=ADVANCED_FACE('',(#2233,#1042),#1365,.F.);
#23226=ADVANCED_FACE('',(#2234,#1043),#1366,.F.);
#23227=ADVANCED_FACE('',(#2235,#1044),#1367,.F.);
#23228=ADVANCED_FACE('',(#2236,#1045),#1368,.F.);
#23229=ADVANCED_FACE('',(#2237),#1369,.T.);
#23230=ADVANCED_FACE('',(#2238),#1370,.T.);
#23231=ADVANCED_FACE('',(#2239),#22776,.F.);
#23232=ADVANCED_FACE('',(#2240),#22777,.F.);
#23233=ADVANCED_FACE('',(#2241),#22778,.F.);
#23234=ADVANCED_FACE('',(#2242),#22779,.F.);
#23235=ADVANCED_FACE('',(#2243),#22780,.F.);
#23236=ADVANCED_FACE('',(#2244),#22781,.F.);
#23237=ADVANCED_FACE('',(#2245),#22782,.F.);
#23238=ADVANCED_FACE('',(#2246),#2114,.F.);
#23239=ADVANCED_FACE('',(#2247),#2115,.F.);
#23240=ADVANCED_FACE('',(#2248),#2116,.F.);
#23241=ADVANCED_FACE('',(#2249),#2117,.F.);
#23242=ADVANCED_FACE('',(#2250),#22783,.T.);
#23243=ADVANCED_FACE('',(#2251),#22784,.T.);
#23244=ADVANCED_FACE('',(#2252),#22785,.T.);
#23245=ADVANCED_FACE('',(#2253),#22786,.T.);
#23246=ADVANCED_FACE('',(#2254),#22787,.F.);
#23247=ADVANCED_FACE('',(#2255),#22788,.F.);
#23248=ADVANCED_FACE('',(#2256),#22789,.F.);
#23249=ADVANCED_FACE('',(#2257),#22790,.F.);
#23250=ADVANCED_FACE('',(#2258,#1046),#1371,.T.);
#23251=ADVANCED_FACE('',(#2259,#1047),#1372,.T.);
#23252=ADVANCED_FACE('',(#2260,#1048),#1373,.T.);
#23253=ADVANCED_FACE('',(#2261,#1049),#1374,.T.);
#23254=ADVANCED_FACE('',(#2262,#1050),#1375,.T.);
#23255=ADVANCED_FACE('',(#2263,#1051),#1376,.F.);
#23256=ADVANCED_FACE('',(#2264),#1377,.F.);
#23257=ADVANCED_FACE('',(#2265),#1378,.F.);
#23258=ADVANCED_FACE('',(#2266,#1052,#1053),#1379,.F.);
#23259=ADVANCED_FACE('',(#2267),#1380,.F.);
#23260=ADVANCED_FACE('',(#2268),#1381,.F.);
#23261=ADVANCED_FACE('',(#2269,#1054),#1382,.F.);
#23262=ADVANCED_FACE('',(#2270),#1383,.F.);
#23263=ADVANCED_FACE('',(#2271),#1384,.F.);
#23264=ADVANCED_FACE('',(#2272),#1385,.F.);
#23265=ADVANCED_FACE('',(#2273),#1386,.F.);
#23266=ADVANCED_FACE('',(#2274),#1387,.F.);
#23267=ADVANCED_FACE('',(#2275,#1055),#1388,.F.);
#23268=ADVANCED_FACE('',(#2276,#1056,#1057,#1058,#1059,#1060),#1389,.F.);
#23269=ADVANCED_FACE('',(#2277),#1390,.F.);
#23270=ADVANCED_FACE('',(#2278),#1391,.F.);
#23271=ADVANCED_FACE('',(#2279),#1392,.F.);
#23272=ADVANCED_FACE('',(#2280),#1393,.F.);
#23273=ADVANCED_FACE('',(#2281),#1394,.F.);
#23274=ADVANCED_FACE('',(#2282),#1395,.F.);
#23275=ADVANCED_FACE('',(#2283),#1396,.F.);
#23276=ADVANCED_FACE('',(#2284),#1397,.F.);
#23277=ADVANCED_FACE('',(#2285,#1061),#1398,.T.);
#23278=ADVANCED_FACE('',(#2286,#1062),#1399,.T.);
#23279=ADVANCED_FACE('',(#2287,#1063),#1400,.T.);
#23280=ADVANCED_FACE('',(#2288,#1064),#1401,.T.);
#23281=ADVANCED_FACE('',(#2289),#1402,.F.);
#23282=ADVANCED_FACE('',(#2290),#1403,.F.);
#23283=ADVANCED_FACE('',(#2291),#1404,.F.);
#23284=ADVANCED_FACE('',(#2292),#1405,.F.);
#23285=ADVANCED_FACE('',(#2293),#1406,.F.);
#23286=ADVANCED_FACE('',(#2294),#1407,.F.);
#23287=ADVANCED_FACE('',(#2295),#1408,.T.);
#23288=ADVANCED_FACE('',(#2296),#1409,.T.);
#23289=ADVANCED_FACE('',(#2297),#1410,.T.);
#23290=ADVANCED_FACE('',(#2298),#1411,.T.);
#23291=ADVANCED_FACE('',(#2299),#1412,.T.);
#23292=ADVANCED_FACE('',(#2300),#1413,.T.);
#23293=ADVANCED_FACE('',(#2301),#1414,.F.);
#23294=ADVANCED_FACE('',(#2302),#1415,.F.);
#23295=ADVANCED_FACE('',(#2303),#1416,.F.);
#23296=ADVANCED_FACE('',(#2304),#1417,.F.);
#23297=ADVANCED_FACE('',(#2305),#1418,.F.);
#23298=ADVANCED_FACE('',(#2306),#1419,.F.);
#23299=ADVANCED_FACE('',(#2307),#1420,.T.);
#23300=ADVANCED_FACE('',(#2308),#1421,.T.);
#23301=ADVANCED_FACE('',(#2309),#1422,.T.);
#23302=ADVANCED_FACE('',(#2310),#1423,.T.);
#23303=ADVANCED_FACE('',(#2311),#1424,.T.);
#23304=ADVANCED_FACE('',(#2312),#1425,.T.);
#23305=ADVANCED_FACE('',(#2313),#1426,.F.);
#23306=ADVANCED_FACE('',(#2314),#1427,.F.);
#23307=ADVANCED_FACE('',(#2315),#1428,.F.);
#23308=ADVANCED_FACE('',(#2316),#1429,.F.);
#23309=ADVANCED_FACE('',(#2317),#1430,.F.);
#23310=ADVANCED_FACE('',(#2318),#1431,.F.);
#23311=ADVANCED_FACE('',(#2319),#1432,.T.);
#23312=ADVANCED_FACE('',(#2320),#1433,.T.);
#23313=ADVANCED_FACE('',(#2321),#1434,.T.);
#23314=ADVANCED_FACE('',(#2322),#1435,.T.);
#23315=ADVANCED_FACE('',(#2323),#1436,.T.);
#23316=ADVANCED_FACE('',(#2324),#1437,.T.);
#23317=ADVANCED_FACE('',(#2325),#1438,.F.);
#23318=ADVANCED_FACE('',(#2326),#1439,.F.);
#23319=ADVANCED_FACE('',(#2327),#1440,.F.);
#23320=ADVANCED_FACE('',(#2328),#1441,.F.);
#23321=ADVANCED_FACE('',(#2329),#1442,.F.);
#23322=ADVANCED_FACE('',(#2330),#1443,.F.);
#23323=ADVANCED_FACE('',(#2331),#1444,.T.);
#23324=ADVANCED_FACE('',(#2332),#1445,.T.);
#23325=ADVANCED_FACE('',(#2333),#1446,.T.);
#23326=ADVANCED_FACE('',(#2334),#1447,.T.);
#23327=ADVANCED_FACE('',(#2335),#1448,.T.);
#23328=ADVANCED_FACE('',(#2336),#1449,.T.);
#23329=ADVANCED_FACE('',(#2337,#1065),#1450,.F.);
#23330=ADVANCED_FACE('',(#2338,#1066),#1451,.F.);
#23331=ADVANCED_FACE('',(#2339,#1067),#1452,.F.);
#23332=ADVANCED_FACE('',(#2340,#1068),#1453,.F.);
#23333=ADVANCED_FACE('',(#2341),#22791,.F.);
#23334=ADVANCED_FACE('',(#2342),#2118,.F.);
#23335=ADVANCED_FACE('',(#2343),#2119,.F.);
#23336=ADVANCED_FACE('',(#2344,#1069),#22792,.F.);
#23337=ADVANCED_FACE('',(#2345),#22793,.T.);
#23338=ADVANCED_FACE('',(#2346),#22794,.T.);
#23339=ADVANCED_FACE('',(#2347),#22795,.T.);
#23340=ADVANCED_FACE('',(#2348),#22796,.T.);
#23341=ADVANCED_FACE('',(#2349,#1070),#22797,.T.);
#23342=ADVANCED_FACE('',(#2350,#1071),#1454,.F.);
#23343=ADVANCED_FACE('',(#2351,#1072),#1455,.F.);
#23344=ADVANCED_FACE('',(#2352,#1073),#1456,.F.);
#23345=ADVANCED_FACE('',(#2353),#1457,.F.);
#23346=ADVANCED_FACE('',(#2354),#1458,.F.);
#23347=ADVANCED_FACE('',(#2355),#1459,.F.);
#23348=ADVANCED_FACE('',(#2356),#1460,.F.);
#23349=ADVANCED_FACE('',(#2357),#2120,.T.);
#23350=ADVANCED_FACE('',(#2358),#2121,.T.);
#23351=ADVANCED_FACE('',(#2359),#22798,.T.);
#23352=ADVANCED_FACE('',(#2360),#1461,.T.);
#23353=ADVANCED_FACE('',(#2361,#1074),#1462,.T.);
#23354=ADVANCED_FACE('',(#2362),#1463,.F.);
#23355=ADVANCED_FACE('',(#2363),#1464,.F.);
#23356=ADVANCED_FACE('',(#2364),#1465,.F.);
#23357=ADVANCED_FACE('',(#2365),#1466,.F.);
#23358=ADVANCED_FACE('',(#2366),#1467,.F.);
#23359=ADVANCED_FACE('',(#2367),#1468,.F.);
#23360=ADVANCED_FACE('',(#2368),#1469,.T.);
#23361=ADVANCED_FACE('',(#2369),#22799,.T.);
#23362=ADVANCED_FACE('',(#2370),#22800,.F.);
#23363=ADVANCED_FACE('',(#2371,#1075),#1470,.F.);
#23364=ADVANCED_FACE('',(#2372,#1076),#1471,.F.);
#23365=ADVANCED_FACE('',(#2373),#22801,.F.);
#23366=ADVANCED_FACE('',(#2374),#22802,.F.);
#23367=ADVANCED_FACE('',(#2375),#22803,.F.);
#23368=ADVANCED_FACE('',(#2376,#1077),#1472,.T.);
#23369=ADVANCED_FACE('',(#2377,#1078),#1473,.F.);
#23370=ADVANCED_FACE('',(#2378,#1079),#1474,.F.);
#23371=ADVANCED_FACE('',(#2379),#1475,.F.);
#23372=ADVANCED_FACE('',(#2380),#1476,.F.);
#23373=ADVANCED_FACE('',(#2381,#1080,#1081),#1477,.F.);
#23374=ADVANCED_FACE('',(#2382),#1478,.F.);
#23375=ADVANCED_FACE('',(#2383),#1479,.F.);
#23376=ADVANCED_FACE('',(#2384,#1082),#1480,.F.);
#23377=ADVANCED_FACE('',(#2385),#1481,.F.);
#23378=ADVANCED_FACE('',(#2386),#1482,.F.);
#23379=ADVANCED_FACE('',(#2387),#1483,.F.);
#23380=ADVANCED_FACE('',(#2388),#1484,.F.);
#23381=ADVANCED_FACE('',(#2389),#1485,.F.);
#23382=ADVANCED_FACE('',(#2390),#644,.T.);
#23383=ADVANCED_FACE('',(#2391),#22804,.F.);
#23384=ADVANCED_FACE('',(#2392),#645,.T.);
#23385=ADVANCED_FACE('',(#2393),#22805,.T.);
#23386=ADVANCED_FACE('',(#2394),#22806,.F.);
#23387=ADVANCED_FACE('',(#2395),#646,.T.);
#23388=ADVANCED_FACE('',(#2396),#22807,.T.);
#23389=ADVANCED_FACE('',(#2397),#647,.T.);
#23390=ADVANCED_FACE('',(#2398),#22808,.F.);
#23391=ADVANCED_FACE('',(#2399),#22809,.T.);
#23392=ADVANCED_FACE('',(#2400,#1083),#1486,.F.);
#23393=ADVANCED_FACE('',(#2401,#1084),#1487,.F.);
#23394=ADVANCED_FACE('',(#2402,#1085),#1488,.F.);
#23395=ADVANCED_FACE('',(#2403,#1086),#1489,.F.);
#23396=ADVANCED_FACE('',(#2404,#1087),#1490,.F.);
#23397=ADVANCED_FACE('',(#2405,#1088),#1491,.F.);
#23398=ADVANCED_FACE('',(#2406),#22810,.F.);
#23399=ADVANCED_FACE('',(#2407),#22811,.F.);
#23400=ADVANCED_FACE('',(#2408),#22812,.F.);
#23401=ADVANCED_FACE('',(#2409),#22813,.T.);
#23402=ADVANCED_FACE('',(#2410,#1089,#1090),#1492,.T.);
#23403=ADVANCED_FACE('',(#2411,#1091,#1092),#1493,.F.);
#23404=ADVANCED_FACE('',(#2412),#1494,.F.);
#23405=ADVANCED_FACE('',(#2413),#22814,.T.);
#23406=ADVANCED_FACE('',(#2414),#1495,.F.);
#23407=ADVANCED_FACE('',(#2415),#22815,.F.);
#23408=ADVANCED_FACE('',(#2416),#22816,.F.);
#23409=ADVANCED_FACE('',(#2417),#1496,.F.);
#23410=ADVANCED_FACE('',(#2418),#22817,.T.);
#23411=ADVANCED_FACE('',(#2419),#1497,.F.);
#23412=ADVANCED_FACE('',(#2420),#1498,.F.);
#23413=ADVANCED_FACE('',(#2421),#1499,.F.);
#23414=ADVANCED_FACE('',(#2422),#22818,.F.);
#23415=ADVANCED_FACE('',(#2423),#22819,.F.);
#23416=ADVANCED_FACE('',(#2424),#22820,.F.);
#23417=ADVANCED_FACE('',(#2425),#22821,.F.);
#23418=ADVANCED_FACE('',(#2426),#1500,.T.);
#23419=ADVANCED_FACE('',(#2427),#1501,.F.);
#23420=ADVANCED_FACE('',(#2428),#1502,.F.);
#23421=ADVANCED_FACE('',(#2429),#1503,.F.);
#23422=ADVANCED_FACE('',(#2430),#1504,.F.);
#23423=ADVANCED_FACE('',(#2431),#1505,.T.);
#23424=ADVANCED_FACE('',(#2432,#1093,#1094,#1095,#1096),#1506,.F.);
#23425=ADVANCED_FACE('',(#2433),#1507,.F.);
#23426=ADVANCED_FACE('',(#2434),#1508,.F.);
#23427=ADVANCED_FACE('',(#2435),#1509,.F.);
#23428=ADVANCED_FACE('',(#2436),#1510,.F.);
#23429=ADVANCED_FACE('',(#2437,#1097,#1098,#1099,#1100),#1511,.T.);
#23430=ADVANCED_FACE('',(#2438),#22822,.F.);
#23431=ADVANCED_FACE('',(#2439),#22823,.F.);
#23432=ADVANCED_FACE('',(#2440),#22824,.F.);
#23433=ADVANCED_FACE('',(#2441),#22825,.F.);
#23434=ADVANCED_FACE('',(#2442),#1512,.T.);
#23435=ADVANCED_FACE('',(#2443),#1513,.F.);
#23436=ADVANCED_FACE('',(#2444),#1514,.F.);
#23437=ADVANCED_FACE('',(#2445),#1515,.F.);
#23438=ADVANCED_FACE('',(#2446),#1516,.F.);
#23439=ADVANCED_FACE('',(#2447),#1517,.T.);
#23440=ADVANCED_FACE('',(#2448,#1101,#1102,#1103,#1104),#1518,.F.);
#23441=ADVANCED_FACE('',(#2449),#1519,.F.);
#23442=ADVANCED_FACE('',(#2450),#1520,.F.);
#23443=ADVANCED_FACE('',(#2451),#1521,.F.);
#23444=ADVANCED_FACE('',(#2452),#1522,.F.);
#23445=ADVANCED_FACE('',(#2453,#1105,#1106,#1107,#1108),#1523,.T.);
#23446=ADVANCED_FACE('',(#2454),#22826,.F.);
#23447=ADVANCED_FACE('',(#2455),#22827,.F.);
#23448=ADVANCED_FACE('',(#2456),#22828,.F.);
#23449=ADVANCED_FACE('',(#2457),#22829,.F.);
#23450=ADVANCED_FACE('',(#2458),#22830,.F.);
#23451=ADVANCED_FACE('',(#2459),#22831,.F.);
#23452=ADVANCED_FACE('',(#2460),#22832,.F.);
#23453=ADVANCED_FACE('',(#2461),#22833,.F.);
#23454=ADVANCED_FACE('',(#2462),#22834,.F.);
#23455=ADVANCED_FACE('',(#2463),#22835,.F.);
#23456=ADVANCED_FACE('',(#2464),#22836,.F.);
#23457=ADVANCED_FACE('',(#2465),#22837,.F.);
#23458=ADVANCED_FACE('',(#2466,#1109,#1110,#1111,#1112,#1113,#1114,#1115,
#1116,#1117),#1524,.F.);
#23459=ADVANCED_FACE('',(#2467),#1525,.F.);
#23460=ADVANCED_FACE('',(#2468),#1526,.F.);
#23461=ADVANCED_FACE('',(#2469),#1527,.F.);
#23462=ADVANCED_FACE('',(#2470),#1528,.F.);
#23463=ADVANCED_FACE('',(#2471,#1118,#1119,#1120,#1121,#1122,#1123,#1124,
#1125,#1126),#1529,.T.);
#23464=ADVANCED_FACE('',(#2472,#1127),#1530,.T.);
#23465=ADVANCED_FACE('',(#2473,#1128),#1531,.F.);
#23466=ADVANCED_FACE('',(#2474,#1129),#1532,.F.);
#23467=ADVANCED_FACE('',(#2475),#1533,.F.);
#23468=ADVANCED_FACE('',(#2476),#22838,.T.);
#23469=ADVANCED_FACE('',(#2477),#22839,.F.);
#23470=ADVANCED_FACE('',(#2478),#1534,.T.);
#23471=ADVANCED_FACE('',(#2479),#22840,.T.);
#23472=ADVANCED_FACE('',(#2480),#254,.T.);
#23473=ADVANCED_FACE('',(#2481),#162,.T.);
#23474=ADVANCED_FACE('',(#2482),#163,.F.);
#23475=ADVANCED_FACE('',(#2483),#164,.F.);
#23476=ADVANCED_FACE('',(#2484),#165,.T.);
#23477=ADVANCED_FACE('',(#2485),#166,.T.);
#23478=ADVANCED_FACE('',(#2486),#255,.T.);
#23479=ADVANCED_FACE('',(#2487),#167,.T.);
#23480=ADVANCED_FACE('',(#2488),#36,.T.);
#23481=ADVANCED_FACE('',(#2489),#168,.F.);
#23482=ADVANCED_FACE('',(#2490),#169,.F.);
#23483=ADVANCED_FACE('',(#2491),#170,.T.);
#23484=ADVANCED_FACE('',(#2492),#256,.T.);
#23485=ADVANCED_FACE('',(#2493),#171,.F.);
#23486=ADVANCED_FACE('',(#2494),#172,.T.);
#23487=ADVANCED_FACE('',(#2495),#257,.T.);
#23488=ADVANCED_FACE('',(#2496),#173,.T.);
#23489=ADVANCED_FACE('',(#2497),#37,.T.);
#23490=ADVANCED_FACE('',(#2498),#174,.T.);
#23491=ADVANCED_FACE('',(#2499),#258,.T.);
#23492=ADVANCED_FACE('',(#2500),#175,.F.);
#23493=ADVANCED_FACE('',(#2501),#176,.T.);
#23494=ADVANCED_FACE('',(#2502),#38,.T.);
#23495=ADVANCED_FACE('',(#2503),#177,.F.);
#23496=ADVANCED_FACE('',(#2504),#178,.F.);
#23497=ADVANCED_FACE('',(#2505),#179,.T.);
#23498=ADVANCED_FACE('',(#2506),#180,.T.);
#23499=ADVANCED_FACE('',(#2507),#259,.T.);
#23500=ADVANCED_FACE('',(#2508),#181,.T.);
#23501=ADVANCED_FACE('',(#2509),#39,.T.);
#23502=ADVANCED_FACE('',(#2510),#182,.F.);
#23503=ADVANCED_FACE('',(#2511),#183,.F.);
#23504=ADVANCED_FACE('',(#2512),#184,.T.);
#23505=ADVANCED_FACE('',(#2513),#260,.T.);
#23506=ADVANCED_FACE('',(#2514),#185,.F.);
#23507=ADVANCED_FACE('',(#2515),#186,.T.);
#23508=ADVANCED_FACE('',(#2516),#261,.T.);
#23509=ADVANCED_FACE('',(#2517),#187,.T.);
#23510=ADVANCED_FACE('',(#2518),#40,.T.);
#23511=ADVANCED_FACE('',(#2519),#188,.T.);
#23512=ADVANCED_FACE('',(#2520),#262,.T.);
#23513=ADVANCED_FACE('',(#2521),#189,.F.);
#23514=ADVANCED_FACE('',(#2522),#190,.T.);
#23515=ADVANCED_FACE('',(#2523),#41,.T.);
#23516=ADVANCED_FACE('',(#2524),#191,.F.);
#23517=ADVANCED_FACE('',(#2525),#192,.F.);
#23518=ADVANCED_FACE('',(#2526),#193,.T.);
#23519=ADVANCED_FACE('',(#2527),#194,.T.);
#23520=ADVANCED_FACE('',(#2528),#263,.T.);
#23521=ADVANCED_FACE('',(#2529),#195,.T.);
#23522=ADVANCED_FACE('',(#2530),#42,.T.);
#23523=ADVANCED_FACE('',(#2531),#196,.F.);
#23524=ADVANCED_FACE('',(#2532),#197,.F.);
#23525=ADVANCED_FACE('',(#2533),#198,.T.);
#23526=ADVANCED_FACE('',(#2534),#264,.T.);
#23527=ADVANCED_FACE('',(#2535),#199,.F.);
#23528=ADVANCED_FACE('',(#2536),#200,.T.);
#23529=ADVANCED_FACE('',(#2537),#265,.T.);
#23530=ADVANCED_FACE('',(#2538),#201,.T.);
#23531=ADVANCED_FACE('',(#2539),#43,.T.);
#23532=ADVANCED_FACE('',(#2540),#202,.T.);
#23533=ADVANCED_FACE('',(#2541),#266,.T.);
#23534=ADVANCED_FACE('',(#2542),#203,.F.);
#23535=ADVANCED_FACE('',(#2543),#204,.T.);
#23536=ADVANCED_FACE('',(#2544),#44,.T.);
#23537=ADVANCED_FACE('',(#2545),#205,.F.);
#23538=ADVANCED_FACE('',(#2546),#206,.F.);
#23539=ADVANCED_FACE('',(#2547),#207,.T.);
#23540=ADVANCED_FACE('',(#2548),#208,.T.);
#23541=ADVANCED_FACE('',(#2549),#267,.T.);
#23542=ADVANCED_FACE('',(#2550),#209,.T.);
#23543=ADVANCED_FACE('',(#2551),#45,.T.);
#23544=ADVANCED_FACE('',(#2552),#210,.F.);
#23545=ADVANCED_FACE('',(#2553),#211,.F.);
#23546=ADVANCED_FACE('',(#2554),#212,.T.);
#23547=ADVANCED_FACE('',(#2555),#268,.T.);
#23548=ADVANCED_FACE('',(#2556),#213,.F.);
#23549=ADVANCED_FACE('',(#2557),#214,.T.);
#23550=ADVANCED_FACE('',(#2558),#269,.T.);
#23551=ADVANCED_FACE('',(#2559),#215,.T.);
#23552=ADVANCED_FACE('',(#2560),#46,.T.);
#23553=ADVANCED_FACE('',(#2561),#216,.T.);
#23554=ADVANCED_FACE('',(#2562),#270,.T.);
#23555=ADVANCED_FACE('',(#2563),#217,.F.);
#23556=ADVANCED_FACE('',(#2564),#218,.T.);
#23557=ADVANCED_FACE('',(#2565),#47,.T.);
#23558=ADVANCED_FACE('',(#2566),#219,.F.);
#23559=ADVANCED_FACE('',(#2567),#271,.T.);
#23560=ADVANCED_FACE('',(#2568),#220,.T.);
#23561=ADVANCED_FACE('',(#2569),#272,.T.);
#23562=ADVANCED_FACE('',(#2570),#221,.T.);
#23563=ADVANCED_FACE('',(#2571),#222,.F.);
#23564=ADVANCED_FACE('',(#2572),#223,.F.);
#23565=ADVANCED_FACE('',(#2573),#48,.T.);
#23566=ADVANCED_FACE('',(#2574),#224,.T.);
#23567=ADVANCED_FACE('',(#2575),#273,.T.);
#23568=ADVANCED_FACE('',(#2576),#225,.T.);
#23569=ADVANCED_FACE('',(#2577),#226,.F.);
#23570=ADVANCED_FACE('',(#2578),#227,.F.);
#23571=ADVANCED_FACE('',(#2579),#228,.T.);
#23572=ADVANCED_FACE('',(#2580),#229,.T.);
#23573=ADVANCED_FACE('',(#2581),#274,.T.);
#23574=ADVANCED_FACE('',(#2582),#230,.T.);
#23575=ADVANCED_FACE('',(#2583),#49,.T.);
#23576=ADVANCED_FACE('',(#2584),#231,.F.);
#23577=ADVANCED_FACE('',(#2585),#232,.F.);
#23578=ADVANCED_FACE('',(#2586),#233,.T.);
#23579=ADVANCED_FACE('',(#2587),#275,.T.);
#23580=ADVANCED_FACE('',(#2588),#234,.F.);
#23581=ADVANCED_FACE('',(#2589),#235,.T.);
#23582=ADVANCED_FACE('',(#2590),#276,.T.);
#23583=ADVANCED_FACE('',(#2591),#236,.T.);
#23584=ADVANCED_FACE('',(#2592),#50,.T.);
#23585=ADVANCED_FACE('',(#2593),#237,.T.);
#23586=ADVANCED_FACE('',(#2594),#277,.T.);
#23587=ADVANCED_FACE('',(#2595),#238,.F.);
#23588=ADVANCED_FACE('',(#2596),#239,.T.);
#23589=ADVANCED_FACE('',(#2597),#51,.T.);
#23590=ADVANCED_FACE('',(#2598),#240,.F.);
#23591=ADVANCED_FACE('',(#2599),#241,.F.);
#23592=ADVANCED_FACE('',(#2600),#242,.F.);
#23593=ADVANCED_FACE('',(#2601),#243,.F.);
#23594=ADVANCED_FACE('',(#2602),#244,.F.);
#23595=ADVANCED_FACE('',(#2603),#245,.F.);
#23596=ADVANCED_FACE('',(#2604),#246,.F.);
#23597=ADVANCED_FACE('',(#2605),#1535,.T.);
#23598=ADVANCED_FACE('',(#2606),#22841,.T.);
#23599=ADVANCED_FACE('',(#2607),#1536,.T.);
#23600=ADVANCED_FACE('',(#2608),#22842,.T.);
#23601=ADVANCED_FACE('',(#2609,#1130,#1131,#1132,#1133),#1537,.F.);
#23602=ADVANCED_FACE('',(#2610),#247,.T.);
#23603=ADVANCED_FACE('',(#2611),#52,.T.);
#23604=ADVANCED_FACE('',(#2612),#248,.T.);
#23605=ADVANCED_FACE('',(#2613),#53,.T.);
#23606=ADVANCED_FACE('',(#2614),#249,.F.);
#23607=ADVANCED_FACE('',(#2615),#250,.F.);
#23608=ADVANCED_FACE('',(#2616),#251,.T.);
#23609=ADVANCED_FACE('',(#2617),#1538,.F.);
#23610=ADVANCED_FACE('',(#2618),#22843,.T.);
#23611=ADVANCED_FACE('',(#2619),#1539,.F.);
#23612=ADVANCED_FACE('',(#2620),#22844,.T.);
#23613=ADVANCED_FACE('',(#2621,#1134,#1135,#1136,#1137),#1540,.T.);
#23614=ADVANCED_FACE('',(#2622,#1138),#1541,.T.);
#23615=ADVANCED_FACE('',(#2623),#1542,.T.);
#23616=ADVANCED_FACE('',(#2624),#22845,.T.);
#23617=ADVANCED_FACE('',(#2625),#1543,.F.);
#23618=ADVANCED_FACE('',(#2626),#1544,.F.);
#23619=ADVANCED_FACE('',(#2627),#1545,.F.);
#23620=ADVANCED_FACE('',(#2628),#1546,.F.);
#23621=ADVANCED_FACE('',(#2629),#1547,.F.);
#23622=ADVANCED_FACE('',(#2630),#1548,.F.);
#23623=ADVANCED_FACE('',(#2631),#1549,.F.);
#23624=ADVANCED_FACE('',(#2632),#1550,.T.);
#23625=ADVANCED_FACE('',(#2633,#1139),#1551,.T.);
#23626=ADVANCED_FACE('',(#2634),#2122,.T.);
#23627=ADVANCED_FACE('',(#2635),#22846,.T.);
#23628=ADVANCED_FACE('',(#2636),#1552,.T.);
#23629=ADVANCED_FACE('',(#2637),#1553,.T.);
#23630=ADVANCED_FACE('',(#2638),#22847,.F.);
#23631=ADVANCED_FACE('',(#2639),#22848,.F.);
#23632=ADVANCED_FACE('',(#2640),#22849,.F.);
#23633=ADVANCED_FACE('',(#2641),#22850,.F.);
#23634=ADVANCED_FACE('',(#2642),#22851,.F.);
#23635=ADVANCED_FACE('',(#2643),#22852,.F.);
#23636=ADVANCED_FACE('',(#2644,#1140),#1554,.F.);
#23637=ADVANCED_FACE('',(#2645),#22853,.F.);
#23638=ADVANCED_FACE('',(#2646),#22854,.F.);
#23639=ADVANCED_FACE('',(#2647),#22855,.F.);
#23640=ADVANCED_FACE('',(#2648),#22856,.F.);
#23641=ADVANCED_FACE('',(#2649,#1141),#1555,.F.);
#23642=ADVANCED_FACE('',(#2650),#1556,.T.);
#23643=ADVANCED_FACE('',(#2651),#1557,.T.);
#23644=ADVANCED_FACE('',(#2652),#22857,.F.);
#23645=ADVANCED_FACE('',(#2653,#1142,#1143,#1144,#1145,#1146),#22858,.T.);
#23646=ADVANCED_FACE('',(#2654),#22859,.T.);
#23647=ADVANCED_FACE('',(#2655),#1558,.F.);
#23648=ADVANCED_FACE('',(#2656),#1559,.F.);
#23649=ADVANCED_FACE('',(#2657),#1560,.F.);
#23650=ADVANCED_FACE('',(#2658),#1561,.F.);
#23651=ADVANCED_FACE('',(#2659),#1562,.F.);
#23652=ADVANCED_FACE('',(#2660),#1563,.F.);
#23653=ADVANCED_FACE('',(#2661),#1564,.F.);
#23654=ADVANCED_FACE('',(#2662),#1565,.F.);
#23655=ADVANCED_FACE('',(#2663),#1566,.F.);
#23656=ADVANCED_FACE('',(#2664),#1567,.F.);
#23657=ADVANCED_FACE('',(#2665),#1568,.F.);
#23658=ADVANCED_FACE('',(#2666),#1569,.F.);
#23659=ADVANCED_FACE('',(#2667),#1570,.F.);
#23660=ADVANCED_FACE('',(#2668),#1571,.F.);
#23661=ADVANCED_FACE('',(#2669),#1572,.F.);
#23662=ADVANCED_FACE('',(#2670),#1573,.F.);
#23663=ADVANCED_FACE('',(#2671),#1574,.F.);
#23664=ADVANCED_FACE('',(#2672),#1575,.F.);
#23665=ADVANCED_FACE('',(#2673),#1576,.F.);
#23666=ADVANCED_FACE('',(#2674),#22860,.T.);
#23667=ADVANCED_FACE('',(#2675),#22861,.T.);
#23668=ADVANCED_FACE('',(#2676),#1577,.F.);
#23669=ADVANCED_FACE('',(#2677),#1578,.F.);
#23670=ADVANCED_FACE('',(#2678),#1579,.F.);
#23671=ADVANCED_FACE('',(#2679),#1580,.F.);
#23672=ADVANCED_FACE('',(#2680),#1581,.F.);
#23673=ADVANCED_FACE('',(#2681),#1582,.F.);
#23674=ADVANCED_FACE('',(#2682),#1583,.F.);
#23675=ADVANCED_FACE('',(#2683),#1584,.F.);
#23676=ADVANCED_FACE('',(#2684),#1585,.F.);
#23677=ADVANCED_FACE('',(#2685),#1586,.F.);
#23678=ADVANCED_FACE('',(#2686),#1587,.F.);
#23679=ADVANCED_FACE('',(#2687),#1588,.F.);
#23680=ADVANCED_FACE('',(#2688),#22862,.T.);
#23681=ADVANCED_FACE('',(#2689),#1589,.F.);
#23682=ADVANCED_FACE('',(#2690),#1590,.F.);
#23683=ADVANCED_FACE('',(#2691),#1591,.F.);
#23684=ADVANCED_FACE('',(#2692),#22863,.F.);
#23685=ADVANCED_FACE('',(#2693),#1592,.F.);
#23686=ADVANCED_FACE('',(#2694),#1593,.T.);
#23687=ADVANCED_FACE('',(#2695),#1594,.T.);
#23688=ADVANCED_FACE('',(#2696),#1595,.F.);
#23689=ADVANCED_FACE('',(#2697),#1596,.F.);
#23690=ADVANCED_FACE('',(#2698),#1597,.F.);
#23691=ADVANCED_FACE('',(#2699),#1598,.F.);
#23692=ADVANCED_FACE('',(#2700),#22864,.T.);
#23693=ADVANCED_FACE('',(#2701),#1599,.T.);
#23694=ADVANCED_FACE('',(#2702,#1147),#22865,.T.);
#23695=ADVANCED_FACE('',(#2703,#1148),#1600,.T.);
#23696=ADVANCED_FACE('',(#2704),#1601,.T.);
#23697=ADVANCED_FACE('',(#2705),#22866,.T.);
#23698=ADVANCED_FACE('',(#2706),#1602,.F.);
#23699=ADVANCED_FACE('',(#2707),#1603,.F.);
#23700=ADVANCED_FACE('',(#2708),#1604,.F.);
#23701=ADVANCED_FACE('',(#2709),#1605,.F.);
#23702=ADVANCED_FACE('',(#2710),#1606,.F.);
#23703=ADVANCED_FACE('',(#2711),#1607,.F.);
#23704=ADVANCED_FACE('',(#2712),#1608,.F.);
#23705=ADVANCED_FACE('',(#2713),#1609,.T.);
#23706=ADVANCED_FACE('',(#2714,#1149),#1610,.T.);
#23707=ADVANCED_FACE('',(#2715),#2123,.T.);
#23708=ADVANCED_FACE('',(#2716),#22867,.T.);
#23709=ADVANCED_FACE('',(#2717),#1611,.T.);
#23710=ADVANCED_FACE('',(#2718),#1612,.T.);
#23711=ADVANCED_FACE('',(#2719),#22868,.F.);
#23712=ADVANCED_FACE('',(#2720),#22869,.F.);
#23713=ADVANCED_FACE('',(#2721),#22870,.F.);
#23714=ADVANCED_FACE('',(#2722),#22871,.F.);
#23715=ADVANCED_FACE('',(#2723),#22872,.F.);
#23716=ADVANCED_FACE('',(#2724),#22873,.F.);
#23717=ADVANCED_FACE('',(#2725,#1150),#1613,.F.);
#23718=ADVANCED_FACE('',(#2726),#22874,.F.);
#23719=ADVANCED_FACE('',(#2727),#22875,.F.);
#23720=ADVANCED_FACE('',(#2728),#22876,.F.);
#23721=ADVANCED_FACE('',(#2729),#22877,.F.);
#23722=ADVANCED_FACE('',(#2730),#1614,.T.);
#23723=ADVANCED_FACE('',(#2731),#1615,.T.);
#23724=ADVANCED_FACE('',(#2732),#1616,.F.);
#23725=ADVANCED_FACE('',(#2733),#1617,.F.);
#23726=ADVANCED_FACE('',(#2734),#1618,.T.);
#23727=ADVANCED_FACE('',(#2735),#1619,.T.);
#23728=ADVANCED_FACE('',(#2736),#22878,.F.);
#23729=ADVANCED_FACE('',(#2737,#1151,#1152,#1153,#1154,#1155),#22879,.T.);
#23730=ADVANCED_FACE('',(#2738),#22880,.T.);
#23731=ADVANCED_FACE('',(#2739),#1620,.F.);
#23732=ADVANCED_FACE('',(#2740),#1621,.F.);
#23733=ADVANCED_FACE('',(#2741),#1622,.F.);
#23734=ADVANCED_FACE('',(#2742),#1623,.F.);
#23735=ADVANCED_FACE('',(#2743),#1624,.F.);
#23736=ADVANCED_FACE('',(#2744),#1625,.F.);
#23737=ADVANCED_FACE('',(#2745),#1626,.F.);
#23738=ADVANCED_FACE('',(#2746),#1627,.F.);
#23739=ADVANCED_FACE('',(#2747),#1628,.F.);
#23740=ADVANCED_FACE('',(#2748),#1629,.F.);
#23741=ADVANCED_FACE('',(#2749),#1630,.F.);
#23742=ADVANCED_FACE('',(#2750),#1631,.F.);
#23743=ADVANCED_FACE('',(#2751),#1632,.F.);
#23744=ADVANCED_FACE('',(#2752),#1633,.F.);
#23745=ADVANCED_FACE('',(#2753),#1634,.F.);
#23746=ADVANCED_FACE('',(#2754),#1635,.F.);
#23747=ADVANCED_FACE('',(#2755),#1636,.F.);
#23748=ADVANCED_FACE('',(#2756),#1637,.F.);
#23749=ADVANCED_FACE('',(#2757),#1638,.F.);
#23750=ADVANCED_FACE('',(#2758),#22881,.T.);
#23751=ADVANCED_FACE('',(#2759),#22882,.T.);
#23752=ADVANCED_FACE('',(#2760),#1639,.F.);
#23753=ADVANCED_FACE('',(#2761),#1640,.F.);
#23754=ADVANCED_FACE('',(#2762),#1641,.F.);
#23755=ADVANCED_FACE('',(#2763),#1642,.F.);
#23756=ADVANCED_FACE('',(#2764),#1643,.F.);
#23757=ADVANCED_FACE('',(#2765),#1644,.F.);
#23758=ADVANCED_FACE('',(#2766),#1645,.F.);
#23759=ADVANCED_FACE('',(#2767),#1646,.F.);
#23760=ADVANCED_FACE('',(#2768),#1647,.F.);
#23761=ADVANCED_FACE('',(#2769),#1648,.F.);
#23762=ADVANCED_FACE('',(#2770),#1649,.F.);
#23763=ADVANCED_FACE('',(#2771),#1650,.F.);
#23764=ADVANCED_FACE('',(#2772),#22883,.T.);
#23765=ADVANCED_FACE('',(#2773),#1651,.F.);
#23766=ADVANCED_FACE('',(#2774),#1652,.F.);
#23767=ADVANCED_FACE('',(#2775),#1653,.F.);
#23768=ADVANCED_FACE('',(#2776),#22884,.F.);
#23769=ADVANCED_FACE('',(#2777),#1654,.F.);
#23770=ADVANCED_FACE('',(#2778),#1655,.T.);
#23771=ADVANCED_FACE('',(#2779),#1656,.T.);
#23772=ADVANCED_FACE('',(#2780),#1657,.F.);
#23773=ADVANCED_FACE('',(#2781),#1658,.F.);
#23774=ADVANCED_FACE('',(#2782),#1659,.F.);
#23775=ADVANCED_FACE('',(#2783),#1660,.F.);
#23776=ADVANCED_FACE('',(#2784),#22885,.T.);
#23777=ADVANCED_FACE('',(#2785),#1661,.T.);
#23778=ADVANCED_FACE('',(#2786,#1156),#22886,.T.);
#23779=ADVANCED_FACE('',(#2787),#22887,.F.);
#23780=ADVANCED_FACE('',(#2788),#22888,.F.);
#23781=ADVANCED_FACE('',(#2789),#22889,.F.);
#23782=ADVANCED_FACE('',(#2790),#22890,.F.);
#23783=ADVANCED_FACE('',(#2791),#22891,.F.);
#23784=ADVANCED_FACE('',(#2792),#22892,.F.);
#23785=ADVANCED_FACE('',(#2793),#22893,.F.);
#23786=ADVANCED_FACE('',(#2794,#1157,#1158,#1159,#1160,#1161,#1162,#1163),
#1662,.F.);
#23787=ADVANCED_FACE('',(#2795),#1663,.F.);
#23788=ADVANCED_FACE('',(#2796,#1164,#1165,#1166,#1167,#1168,#1169,#1170),
#1664,.F.);
#23789=ADVANCED_FACE('',(#2797),#1665,.F.);
#23790=ADVANCED_FACE('',(#2798),#1666,.F.);
#23791=ADVANCED_FACE('',(#2799),#1667,.T.);
#23792=ADVANCED_FACE('',(#2800),#22894,.T.);
#23793=ADVANCED_FACE('',(#2801),#22895,.T.);
#23794=ADVANCED_FACE('',(#2802),#22896,.F.);
#23795=ADVANCED_FACE('',(#2803),#22897,.F.);
#23796=ADVANCED_FACE('',(#2804),#22898,.F.);
#23797=ADVANCED_FACE('',(#2805),#22899,.F.);
#23798=ADVANCED_FACE('',(#2806),#22900,.F.);
#23799=ADVANCED_FACE('',(#2807),#22901,.F.);
#23800=ADVANCED_FACE('',(#2808),#1668,.F.);
#23801=ADVANCED_FACE('',(#2809),#1669,.F.);
#23802=ADVANCED_FACE('',(#2810),#1670,.F.);
#23803=ADVANCED_FACE('',(#2811),#1671,.F.);
#23804=ADVANCED_FACE('',(#2812,#1171,#1172,#1173,#1174,#1175,#1176),#1672,
 .T.);
#23805=ADVANCED_FACE('',(#2813,#1177,#1178,#1179,#1180,#1181,#1182),#1673,
 .F.);
#23806=ADVANCED_FACE('',(#2814),#22902,.F.);
#23807=ADVANCED_FACE('',(#2815),#22903,.F.);
#23808=ADVANCED_FACE('',(#2816),#22904,.F.);
#23809=ADVANCED_FACE('',(#2817),#22905,.F.);
#23810=ADVANCED_FACE('',(#2818),#22906,.F.);
#23811=ADVANCED_FACE('',(#2819),#22907,.F.);
#23812=ADVANCED_FACE('',(#2820),#1674,.F.);
#23813=ADVANCED_FACE('',(#2821),#1675,.F.);
#23814=ADVANCED_FACE('',(#2822),#1676,.F.);
#23815=ADVANCED_FACE('',(#2823),#1677,.F.);
#23816=ADVANCED_FACE('',(#2824,#1183,#1184,#1185,#1186,#1187,#1188),#1678,
 .T.);
#23817=ADVANCED_FACE('',(#2825,#1189,#1190,#1191,#1192,#1193,#1194),#1679,
 .F.);
#23818=ADVANCED_FACE('',(#2826),#1680,.T.);
#23819=ADVANCED_FACE('',(#2827),#1681,.T.);
#23820=ADVANCED_FACE('',(#2828),#1682,.T.);
#23821=ADVANCED_FACE('',(#2829),#1683,.F.);
#23822=ADVANCED_FACE('',(#2830),#1684,.F.);
#23823=ADVANCED_FACE('',(#2831),#1685,.T.);
#23824=ADVANCED_FACE('',(#2832),#1686,.F.);
#23825=ADVANCED_FACE('',(#2833),#1687,.T.);
#23826=ADVANCED_FACE('',(#2834),#1688,.T.);
#23827=ADVANCED_FACE('',(#2835),#1689,.T.);
#23828=ADVANCED_FACE('',(#2836),#1690,.F.);
#23829=ADVANCED_FACE('',(#2837),#1691,.F.);
#23830=ADVANCED_FACE('',(#2838),#1692,.T.);
#23831=ADVANCED_FACE('',(#2839),#1693,.F.);
#23832=ADVANCED_FACE('',(#2840),#22908,.F.);
#23833=ADVANCED_FACE('',(#2841),#22909,.F.);
#23834=ADVANCED_FACE('',(#2842),#22910,.F.);
#23835=ADVANCED_FACE('',(#2843),#22911,.F.);
#23836=ADVANCED_FACE('',(#2844),#22912,.F.);
#23837=ADVANCED_FACE('',(#2845),#22913,.F.);
#23838=ADVANCED_FACE('',(#2846),#22914,.F.);
#23839=ADVANCED_FACE('',(#2847),#22915,.F.);
#23840=ADVANCED_FACE('',(#2848),#22916,.F.);
#23841=ADVANCED_FACE('',(#2849),#22917,.F.);
#23842=ADVANCED_FACE('',(#2850),#22918,.F.);
#23843=ADVANCED_FACE('',(#2851),#22919,.F.);
#23844=ADVANCED_FACE('',(#2852),#22920,.F.);
#23845=ADVANCED_FACE('',(#2853),#22921,.F.);
#23846=ADVANCED_FACE('',(#2854),#22922,.F.);
#23847=ADVANCED_FACE('',(#2855),#22923,.F.);
#23848=ADVANCED_FACE('',(#2856),#22924,.F.);
#23849=ADVANCED_FACE('',(#2857),#22925,.F.);
#23850=ADVANCED_FACE('',(#2858),#22926,.F.);
#23851=ADVANCED_FACE('',(#2859),#22927,.F.);
#23852=ADVANCED_FACE('',(#2860),#22928,.F.);
#23853=ADVANCED_FACE('',(#2861),#22929,.F.);
#23854=ADVANCED_FACE('',(#2862),#22930,.F.);
#23855=ADVANCED_FACE('',(#2863),#22931,.F.);
#23856=ADVANCED_FACE('',(#2864),#22932,.F.);
#23857=ADVANCED_FACE('',(#2865),#22933,.F.);
#23858=ADVANCED_FACE('',(#2866),#22934,.F.);
#23859=ADVANCED_FACE('',(#2867),#22935,.F.);
#23860=ADVANCED_FACE('',(#2868),#22936,.F.);
#23861=ADVANCED_FACE('',(#2869),#22937,.F.);
#23862=ADVANCED_FACE('',(#2870),#22938,.F.);
#23863=ADVANCED_FACE('',(#2871),#22939,.F.);
#23864=ADVANCED_FACE('',(#2872),#22940,.F.);
#23865=ADVANCED_FACE('',(#2873),#22941,.F.);
#23866=ADVANCED_FACE('',(#2874),#22942,.F.);
#23867=ADVANCED_FACE('',(#2875),#22943,.F.);
#23868=ADVANCED_FACE('',(#2876),#22944,.F.);
#23869=ADVANCED_FACE('',(#2877),#22945,.F.);
#23870=ADVANCED_FACE('',(#2878),#22946,.F.);
#23871=ADVANCED_FACE('',(#2879),#22947,.F.);
#23872=ADVANCED_FACE('',(#2880),#22948,.F.);
#23873=ADVANCED_FACE('',(#2881),#22949,.F.);
#23874=ADVANCED_FACE('',(#2882),#22950,.F.);
#23875=ADVANCED_FACE('',(#2883),#22951,.F.);
#23876=ADVANCED_FACE('',(#2884),#22952,.F.);
#23877=ADVANCED_FACE('',(#2885),#22953,.F.);
#23878=ADVANCED_FACE('',(#2886),#22954,.F.);
#23879=ADVANCED_FACE('',(#2887),#22955,.F.);
#23880=ADVANCED_FACE('',(#2888),#22956,.F.);
#23881=ADVANCED_FACE('',(#2889,#1195,#1196,#1197,#1198,#1199,#1200,#1201,
#1202,#1203,#1204,#1205,#1206,#1207,#1208,#1209,#1210,#1211,#1212,#1213,
#1214,#1215,#1216),#1694,.T.);
#23882=ADVANCED_FACE('',(#2890),#1695,.F.);
#23883=ADVANCED_FACE('',(#2891),#1696,.F.);
#23884=ADVANCED_FACE('',(#2892),#1697,.T.);
#23885=ADVANCED_FACE('',(#2893,#1217,#1218,#1219,#1220,#1221,#1222,#1223,
#1224,#1225,#1226),#1698,.F.);
#23886=ADVANCED_FACE('',(#2894,#1227,#1228,#1229,#1230,#1231,#1232,#1233,
#1234,#1235,#1236),#1699,.T.);
#23887=ADVANCED_FACE('',(#2895,#1237,#1238,#1239,#1240,#1241,#1242,#1243,
#1244,#1245,#1246,#1247,#1248,#1249,#1250,#1251,#1252,#1253,#1254,#1255,
#1256,#1257,#1258,#1259),#1700,.T.);
#23888=ADVANCED_FACE('',(#2896),#1701,.F.);
#23889=ADVANCED_FACE('',(#2897),#1702,.F.);
#23890=ADVANCED_FACE('',(#2898),#1703,.F.);
#23891=ADVANCED_FACE('',(#2899),#1704,.F.);
#23892=ADVANCED_FACE('',(#2900,#1260),#1705,.F.);
#23893=ADVANCED_FACE('',(#2901,#1261),#1706,.F.);
#23894=ADVANCED_FACE('',(#2902,#1262),#1707,.F.);
#23895=ADVANCED_FACE('',(#2903,#1263),#1708,.F.);
#23896=ADVANCED_FACE('',(#2904,#1264),#1709,.F.);
#23897=ADVANCED_FACE('',(#2905,#1265),#1710,.F.);
#23898=ADVANCED_FACE('',(#2906,#1266),#1711,.F.);
#23899=ADVANCED_FACE('',(#2907,#1267),#1712,.F.);
#23900=ADVANCED_FACE('',(#2908,#1268),#1713,.F.);
#23901=ADVANCED_FACE('',(#2909,#1269),#1714,.F.);
#23902=ADVANCED_FACE('',(#2910,#1270),#1715,.F.);
#23903=ADVANCED_FACE('',(#2911,#1271),#1716,.F.);
#23904=ADVANCED_FACE('',(#2912,#1272),#1717,.F.);
#23905=ADVANCED_FACE('',(#2913,#1273),#1718,.F.);
#23906=ADVANCED_FACE('',(#2914,#1274),#1719,.F.);
#23907=ADVANCED_FACE('',(#2915,#1275),#1720,.F.);
#23908=ADVANCED_FACE('',(#2916,#1276),#1721,.T.);
#23909=ADVANCED_FACE('',(#2917),#1722,.F.);
#23910=ADVANCED_FACE('',(#2918),#1723,.T.);
#23911=ADVANCED_FACE('',(#2919),#1724,.F.);
#23912=ADVANCED_FACE('',(#2920),#1725,.F.);
#23913=ADVANCED_FACE('',(#2921),#22957,.F.);
#23914=ADVANCED_FACE('',(#2922),#1726,.F.);
#23915=ADVANCED_FACE('',(#2923),#1727,.F.);
#23916=ADVANCED_FACE('',(#2924),#1728,.F.);
#23917=ADVANCED_FACE('',(#2925),#1729,.F.);
#23918=ADVANCED_FACE('',(#2926),#22958,.F.);
#23919=ADVANCED_FACE('',(#2927),#22959,.F.);
#23920=ADVANCED_FACE('',(#2928),#22960,.F.);
#23921=ADVANCED_FACE('',(#2929),#22961,.F.);
#23922=ADVANCED_FACE('',(#2930),#22962,.F.);
#23923=ADVANCED_FACE('',(#2931),#22963,.F.);
#23924=ADVANCED_FACE('',(#2932),#22964,.F.);
#23925=ADVANCED_FACE('',(#2933),#22965,.F.);
#23926=ADVANCED_FACE('',(#2934),#22966,.F.);
#23927=ADVANCED_FACE('',(#2935),#22967,.F.);
#23928=ADVANCED_FACE('',(#2936),#22968,.F.);
#23929=ADVANCED_FACE('',(#2937),#22969,.F.);
#23930=ADVANCED_FACE('',(#2938),#22970,.F.);
#23931=ADVANCED_FACE('',(#2939),#22971,.F.);
#23932=ADVANCED_FACE('',(#2940),#22972,.F.);
#23933=ADVANCED_FACE('',(#2941),#22973,.F.);
#23934=ADVANCED_FACE('',(#2942),#1730,.F.);
#23935=ADVANCED_FACE('',(#2943),#1731,.F.);
#23936=ADVANCED_FACE('',(#2944),#1732,.F.);
#23937=ADVANCED_FACE('',(#2945),#1733,.T.);
#23938=ADVANCED_FACE('',(#2946),#1734,.T.);
#23939=ADVANCED_FACE('',(#2947),#1735,.F.);
#23940=ADVANCED_FACE('',(#2948),#1736,.F.);
#23941=ADVANCED_FACE('',(#2949),#1737,.F.);
#23942=ADVANCED_FACE('',(#2950),#1738,.F.);
#23943=ADVANCED_FACE('',(#2951),#1739,.F.);
#23944=ADVANCED_FACE('',(#2952),#1740,.F.);
#23945=ADVANCED_FACE('',(#2953),#1741,.F.);
#23946=ADVANCED_FACE('',(#2954),#1742,.F.);
#23947=ADVANCED_FACE('',(#2955),#1743,.F.);
#23948=ADVANCED_FACE('',(#2956),#1744,.F.);
#23949=ADVANCED_FACE('',(#2957),#1745,.F.);
#23950=ADVANCED_FACE('',(#2958),#1746,.F.);
#23951=ADVANCED_FACE('',(#2959),#1747,.F.);
#23952=ADVANCED_FACE('',(#2960),#1748,.F.);
#23953=ADVANCED_FACE('',(#2961),#1749,.F.);
#23954=ADVANCED_FACE('',(#2962),#1750,.F.);
#23955=ADVANCED_FACE('',(#2963),#1751,.F.);
#23956=ADVANCED_FACE('',(#2964),#1752,.F.);
#23957=ADVANCED_FACE('',(#2965),#1753,.F.);
#23958=ADVANCED_FACE('',(#2966),#1754,.F.);
#23959=ADVANCED_FACE('',(#2967),#1755,.F.);
#23960=ADVANCED_FACE('',(#2968),#1756,.T.);
#23961=ADVANCED_FACE('',(#2969),#1757,.F.);
#23962=ADVANCED_FACE('',(#2970),#1758,.F.);
#23963=ADVANCED_FACE('',(#2971),#1759,.F.);
#23964=ADVANCED_FACE('',(#2972),#1760,.F.);
#23965=ADVANCED_FACE('',(#2973),#1761,.F.);
#23966=ADVANCED_FACE('',(#2974),#1762,.T.);
#23967=ADVANCED_FACE('',(#2975),#1763,.T.);
#23968=ADVANCED_FACE('',(#2976,#1277,#1278,#1279,#1280,#1281,#1282,#1283,
#1284),#1764,.T.);
#23969=ADVANCED_FACE('',(#2977),#1765,.T.);
#23970=ADVANCED_FACE('',(#2978),#1766,.T.);
#23971=ADVANCED_FACE('',(#2979),#1767,.T.);
#23972=ADVANCED_FACE('',(#2980),#1768,.T.);
#23973=ADVANCED_FACE('',(#2981),#1769,.T.);
#23974=ADVANCED_FACE('',(#2982),#1770,.T.);
#23975=ADVANCED_FACE('',(#2983),#1771,.T.);
#23976=ADVANCED_FACE('',(#2984),#22974,.F.);
#23977=ADVANCED_FACE('',(#2985),#22975,.F.);
#23978=ADVANCED_FACE('',(#2986),#22976,.T.);
#23979=ADVANCED_FACE('',(#2987),#22977,.T.);
#23980=ADVANCED_FACE('',(#2988),#22978,.T.);
#23981=ADVANCED_FACE('',(#2989),#22979,.T.);
#23982=ADVANCED_FACE('',(#2990),#22980,.F.);
#23983=ADVANCED_FACE('',(#2991),#22981,.F.);
#23984=ADVANCED_FACE('',(#2992),#22982,.T.);
#23985=ADVANCED_FACE('',(#2993),#22983,.T.);
#23986=ADVANCED_FACE('',(#2994),#22984,.T.);
#23987=ADVANCED_FACE('',(#2995),#1772,.F.);
#23988=ADVANCED_FACE('',(#2996),#1773,.F.);
#23989=ADVANCED_FACE('',(#2997),#1774,.F.);
#23990=ADVANCED_FACE('',(#2998),#1775,.F.);
#23991=ADVANCED_FACE('',(#2999),#1776,.F.);
#23992=ADVANCED_FACE('',(#3000),#22985,.F.);
#23993=ADVANCED_FACE('',(#3001),#22986,.F.);
#23994=ADVANCED_FACE('',(#3002),#22987,.T.);
#23995=ADVANCED_FACE('',(#3003),#22988,.T.);
#23996=ADVANCED_FACE('',(#3004),#22989,.T.);
#23997=ADVANCED_FACE('',(#3005),#22990,.T.);
#23998=ADVANCED_FACE('',(#3006),#22991,.F.);
#23999=ADVANCED_FACE('',(#3007),#22992,.F.);
#24000=ADVANCED_FACE('',(#3008),#22993,.T.);
#24001=ADVANCED_FACE('',(#3009),#22994,.T.);
#24002=ADVANCED_FACE('',(#3010),#22995,.T.);
#24003=ADVANCED_FACE('',(#3011),#1777,.F.);
#24004=ADVANCED_FACE('',(#3012),#1778,.F.);
#24005=ADVANCED_FACE('',(#3013),#1779,.F.);
#24006=ADVANCED_FACE('',(#3014,#1285),#1780,.F.);
#24007=ADVANCED_FACE('',(#3015,#1286),#1781,.F.);
#24008=ADVANCED_FACE('',(#3016,#1287),#1782,.F.);
#24009=ADVANCED_FACE('',(#3017,#1288),#1783,.F.);
#24010=ADVANCED_FACE('',(#3018,#1289),#1784,.F.);
#24011=ADVANCED_FACE('',(#3019,#1290),#1785,.F.);
#24012=ADVANCED_FACE('',(#3020,#1291),#1786,.F.);
#24013=ADVANCED_FACE('',(#3021,#1292),#1787,.F.);
#24014=ADVANCED_FACE('',(#3022),#22996,.F.);
#24015=ADVANCED_FACE('',(#3023),#22997,.F.);
#24016=ADVANCED_FACE('',(#3024),#22998,.F.);
#24017=ADVANCED_FACE('',(#3025),#2124,.F.);
#24018=ADVANCED_FACE('',(#3026),#2125,.F.);
#24019=ADVANCED_FACE('',(#3027),#22999,.F.);
#24020=ADVANCED_FACE('',(#3028),#23000,.F.);
#24021=ADVANCED_FACE('',(#3029),#23001,.F.);
#24022=ADVANCED_FACE('',(#3030),#23002,.F.);
#24023=ADVANCED_FACE('',(#3031),#23003,.F.);
#24024=ADVANCED_FACE('',(#3032),#23004,.F.);
#24025=ADVANCED_FACE('',(#3033),#23005,.F.);
#24026=ADVANCED_FACE('',(#3034),#23006,.F.);
#24027=ADVANCED_FACE('',(#3035),#2126,.F.);
#24028=ADVANCED_FACE('',(#3036),#2127,.F.);
#24029=ADVANCED_FACE('',(#3037),#23007,.F.);
#24030=ADVANCED_FACE('',(#3038),#252,.F.);
#24031=ADVANCED_FACE('',(#3039),#23008,.T.);
#24032=ADVANCED_FACE('',(#3040),#23009,.F.);
#24033=ADVANCED_FACE('',(#3041),#1788,.T.);
#24034=ADVANCED_FACE('',(#3042),#1789,.T.);
#24035=ADVANCED_FACE('',(#3043),#1790,.T.);
#24036=ADVANCED_FACE('',(#3044),#1791,.T.);
#24037=ADVANCED_FACE('',(#3045),#1792,.T.);
#24038=ADVANCED_FACE('',(#3046),#1793,.T.);
#24039=ADVANCED_FACE('',(#3047),#1794,.T.);
#24040=ADVANCED_FACE('',(#3048),#1795,.T.);
#24041=ADVANCED_FACE('',(#3049),#1796,.T.);
#24042=ADVANCED_FACE('',(#3050),#1797,.T.);
#24043=ADVANCED_FACE('',(#3051),#1798,.T.);
#24044=ADVANCED_FACE('',(#3052),#1799,.T.);
#24045=ADVANCED_FACE('',(#3053),#1800,.T.);
#24046=ADVANCED_FACE('',(#3054),#1801,.T.);
#24047=ADVANCED_FACE('',(#3055),#1802,.T.);
#24048=ADVANCED_FACE('',(#3056),#1803,.T.);
#24049=ADVANCED_FACE('',(#3057),#1804,.T.);
#24050=ADVANCED_FACE('',(#3058),#1805,.T.);
#24051=ADVANCED_FACE('',(#3059),#1806,.T.);
#24052=ADVANCED_FACE('',(#3060),#1807,.T.);
#24053=ADVANCED_FACE('',(#3061),#1808,.T.);
#24054=ADVANCED_FACE('',(#3062),#23010,.T.);
#24055=ADVANCED_FACE('',(#3063),#23011,.T.);
#24056=ADVANCED_FACE('',(#3064),#23012,.T.);
#24057=ADVANCED_FACE('',(#3065),#23013,.T.);
#24058=ADVANCED_FACE('',(#3066),#23014,.T.);
#24059=ADVANCED_FACE('',(#3067),#23015,.T.);
#24060=ADVANCED_FACE('',(#3068),#23016,.F.);
#24061=ADVANCED_FACE('',(#3069),#23017,.F.);
#24062=ADVANCED_FACE('',(#3070),#23018,.F.);
#24063=ADVANCED_FACE('',(#3071),#23019,.F.);
#24064=ADVANCED_FACE('',(#3072),#23020,.F.);
#24065=ADVANCED_FACE('',(#3073),#23021,.F.);
#24066=ADVANCED_FACE('',(#3074),#23022,.T.);
#24067=ADVANCED_FACE('',(#3075),#23023,.T.);
#24068=ADVANCED_FACE('',(#3076),#23024,.F.);
#24069=ADVANCED_FACE('',(#3077),#23025,.F.);
#24070=ADVANCED_FACE('',(#3078),#23026,.F.);
#24071=ADVANCED_FACE('',(#3079),#23027,.F.);
#24072=ADVANCED_FACE('',(#3080),#23028,.F.);
#24073=ADVANCED_FACE('',(#3081),#23029,.F.);
#24074=ADVANCED_FACE('',(#3082,#1293),#1809,.T.);
#24075=ADVANCED_FACE('',(#3083),#1810,.F.);
#24076=ADVANCED_FACE('',(#3084,#1294),#1811,.T.);
#24077=ADVANCED_FACE('',(#3085),#1812,.F.);
#24078=ADVANCED_FACE('',(#3086),#1813,.F.);
#24079=ADVANCED_FACE('',(#3087),#1814,.F.);
#24080=ADVANCED_FACE('',(#3088),#1815,.F.);
#24081=ADVANCED_FACE('',(#3089),#1816,.F.);
#24082=ADVANCED_FACE('',(#3090),#1817,.F.);
#24083=ADVANCED_FACE('',(#3091),#1818,.F.);
#24084=ADVANCED_FACE('',(#3092),#1819,.F.);
#24085=ADVANCED_FACE('',(#3093),#1820,.F.);
#24086=ADVANCED_FACE('',(#3094),#1821,.F.);
#24087=ADVANCED_FACE('',(#3095),#1822,.F.);
#24088=ADVANCED_FACE('',(#3096),#1823,.F.);
#24089=ADVANCED_FACE('',(#3097),#1824,.T.);
#24090=ADVANCED_FACE('',(#3098,#1295),#1825,.F.);
#24091=ADVANCED_FACE('',(#3099),#1826,.T.);
#24092=ADVANCED_FACE('',(#3100),#23030,.T.);
#24093=ADVANCED_FACE('',(#3101),#1827,.T.);
#24094=ADVANCED_FACE('',(#3102),#23031,.T.);
#24095=ADVANCED_FACE('',(#3103),#1828,.T.);
#24096=ADVANCED_FACE('',(#3104),#23032,.F.);
#24097=ADVANCED_FACE('',(#3105),#23033,.T.);
#24098=ADVANCED_FACE('',(#3106),#23034,.F.);
#24099=ADVANCED_FACE('',(#3107),#1829,.T.);
#24100=ADVANCED_FACE('',(#3108),#23035,.F.);
#24101=ADVANCED_FACE('',(#3109),#1830,.T.);
#24102=ADVANCED_FACE('',(#3110),#23036,.F.);
#24103=ADVANCED_FACE('',(#3111),#1831,.T.);
#24104=ADVANCED_FACE('',(#3112),#23037,.F.);
#24105=ADVANCED_FACE('',(#3113),#23038,.T.);
#24106=ADVANCED_FACE('',(#3114),#23039,.F.);
#24107=ADVANCED_FACE('',(#3115),#1832,.T.);
#24108=ADVANCED_FACE('',(#3116),#1833,.T.);
#24109=ADVANCED_FACE('',(#3117),#1834,.T.);
#24110=ADVANCED_FACE('',(#3118),#23040,.F.);
#24111=ADVANCED_FACE('',(#3119),#23041,.T.);
#24112=ADVANCED_FACE('',(#3120),#23042,.F.);
#24113=ADVANCED_FACE('',(#3121),#1835,.T.);
#24114=ADVANCED_FACE('',(#3122),#23043,.F.);
#24115=ADVANCED_FACE('',(#3123),#1836,.T.);
#24116=ADVANCED_FACE('',(#3124),#23044,.F.);
#24117=ADVANCED_FACE('',(#3125),#1837,.T.);
#24118=ADVANCED_FACE('',(#3126),#23045,.F.);
#24119=ADVANCED_FACE('',(#3127),#23046,.T.);
#24120=ADVANCED_FACE('',(#3128),#23047,.F.);
#24121=ADVANCED_FACE('',(#3129),#1838,.T.);
#24122=ADVANCED_FACE('',(#3130),#23048,.T.);
#24123=ADVANCED_FACE('',(#3131),#1839,.T.);
#24124=ADVANCED_FACE('',(#3132),#23049,.T.);
#24125=ADVANCED_FACE('',(#3133),#1840,.T.);
#24126=ADVANCED_FACE('',(#3134),#1841,.T.);
#24127=ADVANCED_FACE('',(#3135),#1842,.T.);
#24128=ADVANCED_FACE('',(#3136),#1843,.T.);
#24129=ADVANCED_FACE('',(#3137),#1844,.T.);
#24130=ADVANCED_FACE('',(#3138),#1845,.T.);
#24131=ADVANCED_FACE('',(#3139),#1846,.T.);
#24132=ADVANCED_FACE('',(#3140),#1847,.T.);
#24133=ADVANCED_FACE('',(#3141),#1848,.T.);
#24134=ADVANCED_FACE('',(#3142),#1849,.T.);
#24135=ADVANCED_FACE('',(#3143),#1850,.T.);
#24136=ADVANCED_FACE('',(#3144),#1851,.T.);
#24137=ADVANCED_FACE('',(#3145),#1852,.F.);
#24138=ADVANCED_FACE('',(#3146),#1853,.F.);
#24139=ADVANCED_FACE('',(#3147),#1854,.F.);
#24140=ADVANCED_FACE('',(#3148),#23050,.F.);
#24141=ADVANCED_FACE('',(#3149),#1855,.T.);
#24142=ADVANCED_FACE('',(#3150),#1856,.T.);
#24143=ADVANCED_FACE('',(#3151),#1857,.T.);
#24144=ADVANCED_FACE('',(#3152),#1858,.F.);
#24145=ADVANCED_FACE('',(#3153),#1859,.F.);
#24146=ADVANCED_FACE('',(#3154),#1860,.F.);
#24147=ADVANCED_FACE('',(#3155),#1861,.F.);
#24148=ADVANCED_FACE('',(#3156),#1862,.F.);
#24149=ADVANCED_FACE('',(#3157),#1863,.F.);
#24150=ADVANCED_FACE('',(#3158),#1864,.F.);
#24151=ADVANCED_FACE('',(#3159),#1865,.T.);
#24152=ADVANCED_FACE('',(#3160),#1866,.T.);
#24153=ADVANCED_FACE('',(#3161),#23051,.T.);
#24154=ADVANCED_FACE('',(#3162),#1867,.T.);
#24155=ADVANCED_FACE('',(#3163),#23052,.T.);
#24156=ADVANCED_FACE('',(#3164),#1868,.T.);
#24157=ADVANCED_FACE('',(#3165),#23053,.F.);
#24158=ADVANCED_FACE('',(#3166),#23054,.T.);
#24159=ADVANCED_FACE('',(#3167),#23055,.F.);
#24160=ADVANCED_FACE('',(#3168),#1869,.T.);
#24161=ADVANCED_FACE('',(#3169),#23056,.F.);
#24162=ADVANCED_FACE('',(#3170),#1870,.T.);
#24163=ADVANCED_FACE('',(#3171),#23057,.F.);
#24164=ADVANCED_FACE('',(#3172),#1871,.T.);
#24165=ADVANCED_FACE('',(#3173),#23058,.F.);
#24166=ADVANCED_FACE('',(#3174),#23059,.T.);
#24167=ADVANCED_FACE('',(#3175),#23060,.F.);
#24168=ADVANCED_FACE('',(#3176),#1872,.T.);
#24169=ADVANCED_FACE('',(#3177),#1873,.T.);
#24170=ADVANCED_FACE('',(#3178),#1874,.T.);
#24171=ADVANCED_FACE('',(#3179),#23061,.F.);
#24172=ADVANCED_FACE('',(#3180),#23062,.T.);
#24173=ADVANCED_FACE('',(#3181),#23063,.F.);
#24174=ADVANCED_FACE('',(#3182),#1875,.T.);
#24175=ADVANCED_FACE('',(#3183),#23064,.F.);
#24176=ADVANCED_FACE('',(#3184),#1876,.T.);
#24177=ADVANCED_FACE('',(#3185),#23065,.F.);
#24178=ADVANCED_FACE('',(#3186),#1877,.T.);
#24179=ADVANCED_FACE('',(#3187),#23066,.F.);
#24180=ADVANCED_FACE('',(#3188),#23067,.T.);
#24181=ADVANCED_FACE('',(#3189),#23068,.F.);
#24182=ADVANCED_FACE('',(#3190),#1878,.T.);
#24183=ADVANCED_FACE('',(#3191),#23069,.T.);
#24184=ADVANCED_FACE('',(#3192),#1879,.T.);
#24185=ADVANCED_FACE('',(#3193),#23070,.T.);
#24186=ADVANCED_FACE('',(#3194),#1880,.T.);
#24187=ADVANCED_FACE('',(#3195,#1296),#1881,.T.);
#24188=ADVANCED_FACE('',(#3196),#1882,.T.);
#24189=ADVANCED_FACE('',(#3197),#1883,.T.);
#24190=ADVANCED_FACE('',(#3198),#1884,.F.);
#24191=ADVANCED_FACE('',(#3199),#1885,.F.);
#24192=ADVANCED_FACE('',(#3200),#23071,.F.);
#24193=ADVANCED_FACE('',(#3201),#23072,.F.);
#24194=ADVANCED_FACE('',(#3202),#1886,.T.);
#24195=ADVANCED_FACE('',(#3203),#1887,.F.);
#24196=ADVANCED_FACE('',(#3204),#1888,.F.);
#24197=ADVANCED_FACE('',(#3205),#1889,.T.);
#24198=ADVANCED_FACE('',(#3206),#23073,.F.);
#24199=ADVANCED_FACE('',(#3207,#1297),#1890,.F.);
#24200=ADVANCED_FACE('',(#3208),#1891,.F.);
#24201=ADVANCED_FACE('',(#3209),#1892,.F.);
#24202=ADVANCED_FACE('',(#3210),#1893,.T.);
#24203=ADVANCED_FACE('',(#3211),#1894,.F.);
#24204=ADVANCED_FACE('',(#3212),#1895,.F.);
#24205=ADVANCED_FACE('',(#3213),#1896,.F.);
#24206=ADVANCED_FACE('',(#3214,#1298),#1897,.T.);
#24207=ADVANCED_FACE('',(#3215),#1898,.T.);
#24208=ADVANCED_FACE('',(#3216,#1299),#1899,.F.);
#24209=ADVANCED_FACE('',(#3217),#1900,.F.);
#24210=ADVANCED_FACE('',(#3218),#1901,.T.);
#24211=ADVANCED_FACE('',(#3219),#1902,.F.);
#24212=ADVANCED_FACE('',(#3220,#1300),#1903,.F.);
#24213=ADVANCED_FACE('',(#3221),#1904,.T.);
#24214=ADVANCED_FACE('',(#3222),#1905,.T.);
#24215=ADVANCED_FACE('',(#3223),#1906,.F.);
#24216=ADVANCED_FACE('',(#3224),#1907,.F.);
#24217=ADVANCED_FACE('',(#3225),#1908,.F.);
#24218=ADVANCED_FACE('',(#3226),#1909,.F.);
#24219=ADVANCED_FACE('',(#3227),#1910,.F.);
#24220=ADVANCED_FACE('',(#3228),#1911,.F.);
#24221=ADVANCED_FACE('',(#3229),#1912,.F.);
#24222=ADVANCED_FACE('',(#3230),#1913,.F.);
#24223=ADVANCED_FACE('',(#3231),#1914,.F.);
#24224=ADVANCED_FACE('',(#3232),#1915,.F.);
#24225=ADVANCED_FACE('',(#3233),#23074,.T.);
#24226=ADVANCED_FACE('',(#3234),#1916,.F.);
#24227=ADVANCED_FACE('',(#3235),#23075,.T.);
#24228=ADVANCED_FACE('',(#3236),#1917,.F.);
#24229=ADVANCED_FACE('',(#3237),#23076,.F.);
#24230=ADVANCED_FACE('',(#3238),#23077,.T.);
#24231=ADVANCED_FACE('',(#3239),#23078,.F.);
#24232=ADVANCED_FACE('',(#3240),#1918,.F.);
#24233=ADVANCED_FACE('',(#3241),#23079,.F.);
#24234=ADVANCED_FACE('',(#3242),#1919,.F.);
#24235=ADVANCED_FACE('',(#3243),#23080,.F.);
#24236=ADVANCED_FACE('',(#3244),#1920,.F.);
#24237=ADVANCED_FACE('',(#3245),#23081,.F.);
#24238=ADVANCED_FACE('',(#3246),#23082,.T.);
#24239=ADVANCED_FACE('',(#3247),#23083,.F.);
#24240=ADVANCED_FACE('',(#3248),#1921,.F.);
#24241=ADVANCED_FACE('',(#3249),#1922,.F.);
#24242=ADVANCED_FACE('',(#3250),#1923,.F.);
#24243=ADVANCED_FACE('',(#3251),#23084,.F.);
#24244=ADVANCED_FACE('',(#3252),#23085,.T.);
#24245=ADVANCED_FACE('',(#3253),#23086,.F.);
#24246=ADVANCED_FACE('',(#3254),#1924,.F.);
#24247=ADVANCED_FACE('',(#3255),#23087,.F.);
#24248=ADVANCED_FACE('',(#3256),#1925,.F.);
#24249=ADVANCED_FACE('',(#3257),#23088,.F.);
#24250=ADVANCED_FACE('',(#3258),#1926,.F.);
#24251=ADVANCED_FACE('',(#3259),#23089,.F.);
#24252=ADVANCED_FACE('',(#3260),#23090,.T.);
#24253=ADVANCED_FACE('',(#3261),#23091,.F.);
#24254=ADVANCED_FACE('',(#3262),#1927,.F.);
#24255=ADVANCED_FACE('',(#3263),#23092,.T.);
#24256=ADVANCED_FACE('',(#3264),#1928,.F.);
#24257=ADVANCED_FACE('',(#3265),#23093,.T.);
#24258=ADVANCED_FACE('',(#3266),#1929,.F.);
#24259=ADVANCED_FACE('',(#3267,#1301),#1930,.T.);
#24260=ADVANCED_FACE('',(#3268),#1931,.T.);
#24261=ADVANCED_FACE('',(#3269),#1932,.F.);
#24262=ADVANCED_FACE('',(#3270),#1933,.F.);
#24263=ADVANCED_FACE('',(#3271,#1302),#1934,.F.);
#24264=ADVANCED_FACE('',(#3272,#1303),#1935,.F.);
#24265=ADVANCED_FACE('',(#3273),#1936,.F.);
#24266=ADVANCED_FACE('',(#3274),#1937,.F.);
#24267=ADVANCED_FACE('',(#3275),#1938,.T.);
#24268=ADVANCED_FACE('',(#3276),#1939,.T.);
#24269=ADVANCED_FACE('',(#3277),#1940,.T.);
#24270=ADVANCED_FACE('',(#3278,#1304,#1305),#1941,.T.);
#24271=ADVANCED_FACE('',(#3279),#1942,.F.);
#24272=ADVANCED_FACE('',(#3280),#1943,.F.);
#24273=ADVANCED_FACE('',(#3281),#1944,.F.);
#24274=ADVANCED_FACE('',(#3282),#1945,.T.);
#24275=ADVANCED_FACE('',(#3283),#1946,.F.);
#24276=ADVANCED_FACE('',(#3284),#1947,.F.);
#24277=ADVANCED_FACE('',(#3285),#1948,.F.);
#24278=ADVANCED_FACE('',(#3286,#1306,#1307),#1949,.T.);
#24279=ADVANCED_FACE('',(#3287),#1950,.T.);
#24280=ADVANCED_FACE('',(#3288),#1951,.T.);
#24281=ADVANCED_FACE('',(#3289),#1952,.T.);
#24282=ADVANCED_FACE('',(#3290),#1953,.T.);
#24283=ADVANCED_FACE('',(#3291,#1308),#1954,.F.);
#24284=ADVANCED_FACE('',(#3292),#1955,.F.);
#24285=ADVANCED_FACE('',(#3293),#1956,.T.);
#24286=ADVANCED_FACE('',(#3294),#1957,.T.);
#24287=ADVANCED_FACE('',(#3295),#1958,.F.);
#24288=ADVANCED_FACE('',(#3296,#1309),#1959,.F.);
#24289=ADVANCED_FACE('',(#3297),#1960,.T.);
#24290=ADVANCED_FACE('',(#3298),#1961,.F.);
#24291=ADVANCED_FACE('',(#3299),#1962,.F.);
#24292=ADVANCED_FACE('',(#3300),#1963,.T.);
#24293=ADVANCED_FACE('',(#3301),#1964,.T.);
#24294=ADVANCED_FACE('',(#3302,#1310),#1965,.F.);
#24295=ADVANCED_FACE('',(#3303),#1966,.T.);
#24296=ADVANCED_FACE('',(#3304),#1967,.T.);
#24297=ADVANCED_FACE('',(#3305),#1968,.F.);
#24298=ADVANCED_FACE('',(#3306,#1311),#1969,.F.);
#24299=ADVANCED_FACE('',(#3307),#1970,.F.);
#24300=ADVANCED_FACE('',(#3308),#1971,.F.);
#24301=ADVANCED_FACE('',(#3309),#23094,.T.);
#24302=ADVANCED_FACE('',(#3310),#23095,.T.);
#24303=ADVANCED_FACE('',(#3311),#1972,.T.);
#24304=ADVANCED_FACE('',(#3312),#1973,.T.);
#24305=ADVANCED_FACE('',(#3313),#1974,.T.);
#24306=ADVANCED_FACE('',(#3314),#23096,.F.);
#24307=ADVANCED_FACE('',(#3315),#23097,.F.);
#24308=ADVANCED_FACE('',(#3316),#23098,.T.);
#24309=ADVANCED_FACE('',(#3317),#23099,.F.);
#24310=ADVANCED_FACE('',(#3318),#23100,.F.);
#24311=ADVANCED_FACE('',(#3319),#1975,.T.);
#24312=ADVANCED_FACE('',(#3320),#1976,.T.);
#24313=ADVANCED_FACE('',(#3321),#23101,.F.);
#24314=ADVANCED_FACE('',(#3322),#23102,.F.);
#24315=ADVANCED_FACE('',(#3323),#23103,.T.);
#24316=ADVANCED_FACE('',(#3324),#1977,.T.);
#24317=ADVANCED_FACE('',(#3325),#1978,.T.);
#24318=ADVANCED_FACE('',(#3326),#23104,.F.);
#24319=ADVANCED_FACE('',(#3327),#23105,.F.);
#24320=ADVANCED_FACE('',(#3328),#23106,.T.);
#24321=ADVANCED_FACE('',(#3329),#23107,.F.);
#24322=ADVANCED_FACE('',(#3330),#23108,.F.);
#24323=ADVANCED_FACE('',(#3331),#1979,.T.);
#24324=ADVANCED_FACE('',(#3332),#1980,.T.);
#24325=ADVANCED_FACE('',(#3333),#1981,.T.);
#24326=ADVANCED_FACE('',(#3334),#23109,.F.);
#24327=ADVANCED_FACE('',(#3335),#23110,.F.);
#24328=ADVANCED_FACE('',(#3336),#23111,.T.);
#24329=ADVANCED_FACE('',(#3337),#23112,.T.);
#24330=ADVANCED_FACE('',(#3338),#23113,.T.);
#24331=ADVANCED_FACE('',(#3339),#1982,.F.);
#24332=ADVANCED_FACE('',(#3340,#1312),#1983,.F.);
#24333=ADVANCED_FACE('',(#3341),#1984,.F.);
#24334=ADVANCED_FACE('',(#3342),#1985,.F.);
#24335=ADVANCED_FACE('',(#3343),#1986,.T.);
#24336=ADVANCED_FACE('',(#3344),#1987,.T.);
#24337=ADVANCED_FACE('',(#3345),#1988,.T.);
#24338=ADVANCED_FACE('',(#3346),#1989,.T.);
#24339=ADVANCED_FACE('',(#3347),#1990,.T.);
#24340=ADVANCED_FACE('',(#3348),#1991,.T.);
#24341=ADVANCED_FACE('',(#3349),#1992,.T.);
#24342=ADVANCED_FACE('',(#3350),#1993,.T.);
#24343=ADVANCED_FACE('',(#3351,#1313),#1994,.T.);
#24344=ADVANCED_FACE('',(#3352,#1314),#1995,.F.);
#24345=ADVANCED_FACE('',(#3353),#1996,.F.);
#24346=ADVANCED_FACE('',(#3354),#23114,.F.);
#24347=ADVANCED_FACE('',(#3355),#1997,.F.);
#24348=ADVANCED_FACE('',(#3356),#1998,.T.);
#24349=ADVANCED_FACE('',(#3357),#23115,.F.);
#24350=ADVANCED_FACE('',(#3358),#23116,.F.);
#24351=ADVANCED_FACE('',(#3359),#23117,.F.);
#24352=ADVANCED_FACE('',(#3360),#23118,.F.);
#24353=ADVANCED_FACE('',(#3361),#648,.F.);
#24354=ADVANCED_FACE('',(#3362),#253,.F.);
#24355=ADVANCED_FACE('',(#3363),#2128,.T.);
#24356=ADVANCED_FACE('',(#3364),#278,.T.);
#24357=ADVANCED_FACE('',(#3365),#2129,.T.);
#24358=ADVANCED_FACE('',(#3366),#2130,.T.);
#24359=ADVANCED_FACE('',(#3367),#23119,.T.);
#24360=ADVANCED_FACE('',(#3368),#23120,.T.);
#24361=ADVANCED_FACE('',(#3369),#279,.T.);
#24362=ADVANCED_FACE('',(#3370,#1315),#1999,.F.);
#24363=ADVANCED_FACE('',(#3371,#1316),#2000,.F.);
#24364=ADVANCED_FACE('',(#3372),#2001,.F.);
#24365=ADVANCED_FACE('',(#3373),#2002,.F.);
#24366=ADVANCED_FACE('',(#3374),#2003,.F.);
#24367=ADVANCED_FACE('',(#3375),#2004,.F.);
#24368=ADVANCED_FACE('',(#3376),#2005,.F.);
#24369=ADVANCED_FACE('',(#3377),#2006,.F.);
#24370=ADVANCED_FACE('',(#3378),#2007,.T.);
#24371=ADVANCED_FACE('',(#3379),#2008,.T.);
#24372=ADVANCED_FACE('',(#3380),#2009,.T.);
#24373=ADVANCED_FACE('',(#3381),#2010,.T.);
#24374=ADVANCED_FACE('',(#3382),#2011,.T.);
#24375=ADVANCED_FACE('',(#3383),#2012,.T.);
#24376=ADVANCED_FACE('',(#3384),#2013,.T.);
#24377=ADVANCED_FACE('',(#3385),#2131,.T.);
#24378=ADVANCED_FACE('',(#3386),#2132,.T.);
#24379=ADVANCED_FACE('',(#3387),#2133,.T.);
#24380=ADVANCED_FACE('',(#3388),#2134,.T.);
#24381=ADVANCED_FACE('',(#3389),#2135,.T.);
#24382=ADVANCED_FACE('',(#3390),#2136,.T.);
#24383=ADVANCED_FACE('',(#3391),#2137,.T.);
#24384=ADVANCED_FACE('',(#3392),#2138,.T.);
#24385=ADVANCED_FACE('',(#3393),#2139,.T.);
#24386=ADVANCED_FACE('',(#3394),#2140,.T.);
#24387=ADVANCED_FACE('',(#3395),#2014,.T.);
#24388=ADVANCED_FACE('',(#3396),#2015,.T.);
#24389=ADVANCED_FACE('',(#3397),#2016,.T.);
#24390=ADVANCED_FACE('',(#3398),#2017,.T.);
#24391=ADVANCED_FACE('',(#3399),#2018,.T.);
#24392=ADVANCED_FACE('',(#3400),#2019,.T.);
#24393=ADVANCED_FACE('',(#3401,#1317),#2020,.F.);
#24394=ADVANCED_FACE('',(#3402),#23121,.F.);
#24395=ADVANCED_FACE('',(#3403),#2141,.F.);
#24396=ADVANCED_FACE('',(#3404),#23122,.F.);
#24397=ADVANCED_FACE('',(#3405),#2142,.F.);
#24398=ADVANCED_FACE('',(#3406),#23123,.F.);
#24399=ADVANCED_FACE('',(#3407),#2143,.F.);
#24400=ADVANCED_FACE('',(#3408),#23124,.F.);
#24401=ADVANCED_FACE('',(#3409),#2144,.F.);
#24402=ADVANCED_FACE('',(#3410),#23125,.F.);
#24403=ADVANCED_FACE('',(#3411),#2145,.F.);
#24404=ADVANCED_FACE('',(#3412),#23126,.F.);
#24405=ADVANCED_FACE('',(#3413),#2146,.F.);
#24406=ADVANCED_FACE('',(#3414),#23127,.F.);
#24407=ADVANCED_FACE('',(#3415),#2147,.F.);
#24408=ADVANCED_FACE('',(#3416),#23128,.F.);
#24409=ADVANCED_FACE('',(#3417),#2148,.F.);
#24410=ADVANCED_FACE('',(#3418),#2021,.F.);
#24411=ADVANCED_FACE('',(#3419),#2022,.F.);
#24412=ADVANCED_FACE('',(#3420),#2023,.F.);
#24413=ADVANCED_FACE('',(#3421),#2024,.F.);
#24414=ADVANCED_FACE('',(#3422),#2025,.F.);
#24415=ADVANCED_FACE('',(#3423),#2026,.T.);
#24416=ADVANCED_FACE('',(#3424),#2027,.F.);
#24417=ADVANCED_FACE('',(#3425),#2028,.F.);
#24418=ADVANCED_FACE('',(#3426,#1318,#1319,#1320,#1321,#1322,#1323,#1324,
#1325),#2029,.F.);
#24419=ADVANCED_FACE('',(#3427),#2030,.F.);
#24420=ADVANCED_FACE('',(#3428),#23129,.F.);
#24421=ADVANCED_FACE('',(#3429),#23130,.F.);
#24422=ADVANCED_FACE('',(#3430),#2149,.T.);
#24423=ADVANCED_FACE('',(#3431),#2150,.F.);
#24424=ADVANCED_FACE('',(#3432),#23131,.T.);
#24425=ADVANCED_FACE('',(#3433),#23132,.T.);
#24426=ADVANCED_FACE('',(#3434),#23133,.T.);
#24427=ADVANCED_FACE('',(#3435,#1326),#2031,.F.);
#24428=ADVANCED_FACE('',(#3436),#2032,.F.);
#24429=ADVANCED_FACE('',(#3437,#1327),#2033,.F.);
#24430=ADVANCED_FACE('',(#3438,#1328),#2034,.F.);
#24431=ADVANCED_FACE('',(#3439),#2035,.F.);
#24432=ADVANCED_FACE('',(#3440),#2036,.F.);
#24433=ADVANCED_FACE('',(#3441),#2037,.F.);
#24434=ADVANCED_FACE('',(#3442),#2038,.F.);
#24435=ADVANCED_FACE('',(#3443),#2039,.F.);
#24436=ADVANCED_FACE('',(#3444),#2040,.F.);
#24437=ADVANCED_FACE('',(#3445),#2041,.T.);
#24438=ADVANCED_FACE('',(#3446),#2042,.T.);
#24439=ADVANCED_FACE('',(#3447),#2043,.T.);
#24440=ADVANCED_FACE('',(#3448),#2044,.T.);
#24441=ADVANCED_FACE('',(#3449),#2045,.T.);
#24442=ADVANCED_FACE('',(#3450),#2046,.T.);
#24443=ADVANCED_FACE('',(#3451),#23134,.T.);
#24444=ADVANCED_FACE('',(#3452),#23135,.F.);
#24445=ADVANCED_FACE('',(#3453,#1329),#2047,.F.);
#24446=ADVANCED_FACE('',(#3454,#1330),#2048,.F.);
#24447=ADVANCED_FACE('',(#3455),#23136,.T.);
#24448=ADVANCED_FACE('',(#3456),#23137,.F.);
#24449=ADVANCED_FACE('',(#3457),#2049,.F.);
#24450=ADVANCED_FACE('',(#3458),#2050,.F.);
#24451=ADVANCED_FACE('',(#3459),#2051,.F.);
#24452=ADVANCED_FACE('',(#3460),#2052,.F.);
#24453=ADVANCED_FACE('',(#3461),#23138,.T.);
#24454=ADVANCED_FACE('',(#3462),#2151,.T.);
#24455=ADVANCED_FACE('',(#3463),#2152,.T.);
#24456=ADVANCED_FACE('',(#3464),#23139,.T.);
#24457=ADVANCED_FACE('',(#3465),#2053,.T.);
#24458=ADVANCED_FACE('',(#3466,#1331),#2054,.T.);
#24459=ADVANCED_FACE('',(#3467,#1332),#2055,.T.);
#24460=ADVANCED_FACE('',(#3468),#2056,.F.);
#24461=ADVANCED_FACE('',(#3469),#2057,.F.);
#24462=ADVANCED_FACE('',(#3470),#2058,.F.);
#24463=ADVANCED_FACE('',(#3471),#2059,.F.);
#24464=ADVANCED_FACE('',(#3472),#2060,.F.);
#24465=ADVANCED_FACE('',(#3473),#2061,.F.);
#24466=ADVANCED_FACE('',(#3474),#2062,.T.);
#24467=ADVANCED_FACE('',(#3475),#2153,.T.);
#24468=ADVANCED_FACE('',(#3476),#2154,.F.);
#24469=ADVANCED_FACE('',(#3477),#23140,.T.);
#24470=ADVANCED_FACE('',(#3478),#23141,.T.);
#24471=ADVANCED_FACE('',(#3479),#23142,.T.);
#24472=ADVANCED_FACE('',(#3480,#1333),#2063,.F.);
#24473=ADVANCED_FACE('',(#3481),#2064,.F.);
#24474=ADVANCED_FACE('',(#3482,#1334),#2065,.F.);
#24475=ADVANCED_FACE('',(#3483,#1335),#2066,.F.);
#24476=ADVANCED_FACE('',(#3484),#2067,.F.);
#24477=ADVANCED_FACE('',(#3485),#2068,.F.);
#24478=ADVANCED_FACE('',(#3486),#2069,.F.);
#24479=ADVANCED_FACE('',(#3487),#2070,.F.);
#24480=ADVANCED_FACE('',(#3488),#2071,.F.);
#24481=ADVANCED_FACE('',(#3489),#2072,.F.);
#24482=ADVANCED_FACE('',(#3490),#2073,.T.);
#24483=ADVANCED_FACE('',(#3491),#2074,.T.);
#24484=ADVANCED_FACE('',(#3492),#2075,.T.);
#24485=ADVANCED_FACE('',(#3493),#2076,.T.);
#24486=ADVANCED_FACE('',(#3494),#2077,.T.);
#24487=ADVANCED_FACE('',(#3495),#2078,.T.);
#24488=ADVANCED_FACE('',(#3496),#23143,.T.);
#24489=ADVANCED_FACE('',(#3497),#23144,.F.);
#24490=ADVANCED_FACE('',(#3498,#1336),#2079,.F.);
#24491=ADVANCED_FACE('',(#3499,#1337),#2080,.F.);
#24492=ADVANCED_FACE('',(#3500),#23145,.T.);
#24493=ADVANCED_FACE('',(#3501),#23146,.F.);
#24494=ADVANCED_FACE('',(#3502),#2081,.F.);
#24495=ADVANCED_FACE('',(#3503),#2082,.F.);
#24496=ADVANCED_FACE('',(#3504),#2083,.F.);
#24497=ADVANCED_FACE('',(#3505),#2084,.F.);
#24498=ADVANCED_FACE('',(#3506),#23147,.T.);
#24499=ADVANCED_FACE('',(#3507),#2155,.T.);
#24500=ADVANCED_FACE('',(#3508),#2156,.T.);
#24501=ADVANCED_FACE('',(#3509),#23148,.T.);
#24502=ADVANCED_FACE('',(#3510),#2085,.T.);
#24503=ADVANCED_FACE('',(#3511,#1338),#2086,.T.);
#24504=ADVANCED_FACE('',(#3512,#1339),#2087,.T.);
#24505=ADVANCED_FACE('',(#3513),#2088,.F.);
#24506=ADVANCED_FACE('',(#3514),#2089,.F.);
#24507=ADVANCED_FACE('',(#3515),#2090,.F.);
#24508=ADVANCED_FACE('',(#3516),#2091,.F.);
#24509=ADVANCED_FACE('',(#3517),#2092,.F.);
#24510=ADVANCED_FACE('',(#3518),#2093,.F.);
#24511=ADVANCED_FACE('',(#3519),#2094,.T.);
#24512=ADVANCED_FACE('',(#3520),#23149,.T.);
#24513=ADVANCED_FACE('',(#3521),#2157,.T.);
#24514=ADVANCED_FACE('',(#3522),#2158,.T.);
#24515=ADVANCED_FACE('',(#3523),#23150,.T.);
#24516=ADVANCED_FACE('',(#3524),#2095,.T.);
#24517=ADVANCED_FACE('',(#3525,#1340),#2096,.T.);
#24518=ADVANCED_FACE('',(#3526,#1341),#2097,.T.);
#24519=ADVANCED_FACE('',(#3527),#2098,.F.);
#24520=ADVANCED_FACE('',(#3528),#2099,.F.);
#24521=ADVANCED_FACE('',(#3529),#2100,.F.);
#24522=ADVANCED_FACE('',(#3530),#2101,.F.);
#24523=ADVANCED_FACE('',(#3531),#2102,.F.);
#24524=ADVANCED_FACE('',(#3532),#2103,.F.);
#24525=ADVANCED_FACE('',(#3533),#2104,.T.);
#24526=CLOSED_SHELL('',(#23151,#23152,#23153,#23154,#23155,#23156,#23157,
#23158,#23159,#23160,#23161,#23162,#23163,#23164,#23165,#23166,#23167,#23168,
#23169,#23170,#23171,#23172,#23173,#23174,#23175,#23176));
#24527=CLOSED_SHELL('',(#23177,#23178,#23179,#23180,#23181,#23182,#23183,
#23184,#23185,#23186,#23187,#23188,#23189,#23190,#23191,#23192,#23193,#23194,
#23195,#23196,#23197,#23198,#23199,#23200,#23201));
#24528=CLOSED_SHELL('',(#23202,#23203,#23204,#23205,#23206,#23207,#23208,
#23209,#23210,#23211,#23212,#23213,#23214,#23215,#23216,#23217,#23218,#23219,
#23220,#23221,#23222,#23223,#23224,#23225,#23226,#23227,#23228,#23229,#23230));
#24529=CLOSED_SHELL('',(#23231,#23232,#23233,#23234,#23235,#23236,#23237,
#23238,#23239,#23240,#23241,#23242,#23243,#23244,#23245,#23246,#23247,#23248,
#23249,#23250,#23251,#23252,#23253,#23254,#23255,#23256,#23257,#23258,#23259,
#23260,#23261,#23262,#23263,#23264,#23265,#23266,#23267,#23268,#23269,#23270,
#23271,#23272,#23273,#23274,#23275,#23276,#23277,#23278,#23279,#23280,#23281,
#23282,#23283,#23284,#23285,#23286,#23287,#23288,#23289,#23290,#23291,#23292,
#23293,#23294,#23295,#23296,#23297,#23298,#23299,#23300,#23301,#23302,#23303,
#23304,#23305,#23306,#23307,#23308,#23309,#23310,#23311,#23312,#23313,#23314,
#23315,#23316,#23317,#23318,#23319,#23320,#23321,#23322,#23323,#23324,#23325,
#23326,#23327,#23328,#23329,#23330,#23331,#23332));
#24530=CLOSED_SHELL('',(#23333,#23334,#23335,#23336,#23337,#23338,#23339,
#23340,#23341,#23342,#23343,#23344,#23345,#23346,#23347,#23348));
#24531=CLOSED_SHELL('',(#23349,#23350,#23351,#23352,#23353,#23354,#23355,
#23356,#23357,#23358,#23359,#23360));
#24532=CLOSED_SHELL('',(#23361,#23362,#23363,#23364));
#24533=CLOSED_SHELL('',(#23365,#23366,#23367,#23368,#23369,#23370,#23371,
#23372,#23373,#23374,#23375,#23376,#23377,#23378,#23379,#23380,#23381));
#24534=CLOSED_SHELL('',(#23382,#23383,#23384,#23385,#23386,#23387,#23388,
#23389,#23390,#23391,#23392,#23393,#23394,#23395,#23396,#23397));
#24535=CLOSED_SHELL('',(#23398,#23399,#23400,#23401,#23402,#23403,#23404,
#23405,#23406,#23407,#23408,#23409,#23410,#23411,#23412,#23413));
#24536=CLOSED_SHELL('',(#23414,#23415,#23416,#23417,#23418,#23419,#23420,
#23421,#23422,#23423,#23424,#23425,#23426,#23427,#23428,#23429));
#24537=CLOSED_SHELL('',(#23430,#23431,#23432,#23433,#23434,#23435,#23436,
#23437,#23438,#23439,#23440,#23441,#23442,#23443,#23444,#23445));
#24538=CLOSED_SHELL('',(#23446,#23447,#23448,#23449,#23450,#23451,#23452,
#23453,#23454,#23455,#23456,#23457,#23458,#23459,#23460,#23461,#23462,#23463,
#23464,#23465,#23466));
#24539=CLOSED_SHELL('',(#23467,#23468,#23469,#23470,#23471,#23472,#23473,
#23474,#23475,#23476,#23477,#23478,#23479,#23480,#23481,#23482,#23483,#23484,
#23485,#23486,#23487,#23488,#23489,#23490,#23491,#23492,#23493,#23494,#23495,
#23496,#23497,#23498,#23499,#23500,#23501,#23502,#23503,#23504,#23505,#23506,
#23507,#23508,#23509,#23510,#23511,#23512,#23513,#23514,#23515,#23516,#23517,
#23518,#23519,#23520,#23521,#23522,#23523,#23524,#23525,#23526,#23527,#23528,
#23529,#23530,#23531,#23532,#23533,#23534,#23535,#23536,#23537,#23538,#23539,
#23540,#23541,#23542,#23543,#23544,#23545,#23546,#23547,#23548,#23549,#23550,
#23551,#23552,#23553,#23554,#23555,#23556,#23557,#23558,#23559,#23560,#23561,
#23562,#23563,#23564,#23565,#23566,#23567,#23568,#23569,#23570,#23571,#23572,
#23573,#23574,#23575,#23576,#23577,#23578,#23579,#23580,#23581,#23582,#23583,
#23584,#23585,#23586,#23587,#23588,#23589,#23590,#23591,#23592,#23593,#23594,
#23595,#23596,#23597,#23598,#23599,#23600,#23601,#23602,#23603,#23604,#23605,
#23606,#23607,#23608,#23609,#23610,#23611,#23612,#23613));
#24540=CLOSED_SHELL('',(#23614,#23615,#23616,#23617,#23618,#23619,#23620,
#23621,#23622,#23623));
#24541=CLOSED_SHELL('',(#23624,#23625,#23626,#23627,#23628,#23629,#23630,
#23631,#23632,#23633,#23634,#23635,#23636,#23637,#23638,#23639,#23640,#23641,
#23642,#23643,#23644,#23645,#23646,#23647,#23648,#23649,#23650,#23651,#23652,
#23653,#23654,#23655,#23656,#23657,#23658,#23659,#23660,#23661,#23662,#23663,
#23664,#23665,#23666,#23667,#23668,#23669,#23670,#23671,#23672,#23673,#23674,
#23675,#23676,#23677,#23678,#23679,#23680,#23681,#23682,#23683,#23684,#23685,
#23686,#23687,#23688,#23689,#23690,#23691,#23692,#23693,#23694));
#24542=CLOSED_SHELL('',(#23695,#23696,#23697,#23698,#23699,#23700,#23701,
#23702,#23703,#23704));
#24543=CLOSED_SHELL('',(#23705,#23706,#23707,#23708,#23709,#23710,#23711,
#23712,#23713,#23714,#23715,#23716,#23717,#23718,#23719,#23720,#23721,#23722,
#23723,#23724,#23725,#23726,#23727,#23728,#23729,#23730,#23731,#23732,#23733,
#23734,#23735,#23736,#23737,#23738,#23739,#23740,#23741,#23742,#23743,#23744,
#23745,#23746,#23747,#23748,#23749,#23750,#23751,#23752,#23753,#23754,#23755,
#23756,#23757,#23758,#23759,#23760,#23761,#23762,#23763,#23764,#23765,#23766,
#23767,#23768,#23769,#23770,#23771,#23772,#23773,#23774,#23775,#23776,#23777,
#23778));
#24544=CLOSED_SHELL('',(#23779,#23780,#23781,#23782,#23783,#23784,#23785,
#23786,#23787,#23788,#23789,#23790,#23791,#23792,#23793));
#24545=CLOSED_SHELL('',(#23794,#23795,#23796,#23797,#23798,#23799,#23800,
#23801,#23802,#23803,#23804,#23805));
#24546=CLOSED_SHELL('',(#23806,#23807,#23808,#23809,#23810,#23811,#23812,
#23813,#23814,#23815,#23816,#23817));
#24547=CLOSED_SHELL('',(#23818,#23819,#23820,#23821,#23822,#23823,#23824));
#24548=CLOSED_SHELL('',(#23825,#23826,#23827,#23828,#23829,#23830,#23831));
#24549=CLOSED_SHELL('',(#23832,#23833,#23834,#23835,#23836,#23837,#23838,
#23839,#23840,#23841,#23842,#23843,#23844,#23845,#23846,#23847,#23848,#23849,
#23850,#23851,#23852,#23853,#23854,#23855,#23856,#23857,#23858,#23859,#23860,
#23861,#23862,#23863,#23864,#23865,#23866,#23867,#23868,#23869,#23870,#23871,
#23872,#23873,#23874,#23875,#23876,#23877,#23878,#23879,#23880,#23881,#23882,
#23883,#23884,#23885,#23886,#23887,#23888,#23889,#23890,#23891,#23892,#23893,
#23894,#23895,#23896,#23897,#23898,#23899,#23900,#23901,#23902,#23903,#23904,
#23905,#23906,#23907,#23908,#23909,#23910,#23911,#23912,#23913,#23914,#23915,
#23916,#23917));
#24550=CLOSED_SHELL('',(#23918,#23919,#23920,#23921,#23922,#23923,#23924,
#23925,#23926,#23927,#23928,#23929,#23930,#23931,#23932,#23933,#23934,#23935,
#23936,#23937,#23938,#23939,#23940,#23941,#23942,#23943,#23944,#23945,#23946,
#23947,#23948,#23949,#23950,#23951,#23952,#23953,#23954,#23955,#23956,#23957,
#23958,#23959,#23960,#23961,#23962,#23963,#23964,#23965,#23966,#23967,#23968,
#23969,#23970,#23971,#23972,#23973,#23974,#23975,#23976,#23977,#23978,#23979,
#23980,#23981,#23982,#23983,#23984,#23985,#23986,#23987,#23988,#23989,#23990,
#23991,#23992,#23993,#23994,#23995,#23996,#23997,#23998,#23999,#24000,#24001,
#24002,#24003,#24004,#24005,#24006,#24007,#24008,#24009,#24010,#24011,#24012,
#24013));
#24551=CLOSED_SHELL('',(#24014,#24015,#24016,#24017,#24018,#24019,#24020,
#24021,#24022,#24023,#24024,#24025,#24026,#24027,#24028,#24029,#24030,#24031,
#24032,#24033,#24034,#24035,#24036,#24037,#24038,#24039,#24040,#24041,#24042,
#24043,#24044,#24045,#24046,#24047,#24048,#24049,#24050,#24051,#24052,#24053,
#24054,#24055,#24056,#24057,#24058,#24059,#24060,#24061,#24062,#24063,#24064,
#24065,#24066,#24067,#24068,#24069,#24070,#24071,#24072,#24073,#24074,#24075,
#24076,#24077,#24078,#24079,#24080,#24081,#24082,#24083,#24084,#24085,#24086,
#24087,#24088,#24089,#24090,#24091,#24092,#24093,#24094,#24095,#24096,#24097,
#24098,#24099,#24100,#24101,#24102,#24103,#24104,#24105,#24106,#24107,#24108,
#24109,#24110,#24111,#24112,#24113,#24114,#24115,#24116,#24117,#24118,#24119,
#24120,#24121,#24122,#24123,#24124,#24125,#24126,#24127,#24128,#24129,#24130,
#24131,#24132,#24133,#24134,#24135,#24136,#24137,#24138,#24139,#24140,#24141,
#24142,#24143,#24144,#24145,#24146,#24147,#24148,#24149,#24150,#24151,#24152,
#24153,#24154,#24155,#24156,#24157,#24158,#24159,#24160,#24161,#24162,#24163,
#24164,#24165,#24166,#24167,#24168,#24169,#24170,#24171,#24172,#24173,#24174,
#24175,#24176,#24177,#24178,#24179,#24180,#24181,#24182,#24183,#24184,#24185,
#24186,#24187,#24188,#24189,#24190,#24191,#24192,#24193,#24194,#24195,#24196,
#24197,#24198,#24199,#24200,#24201,#24202,#24203,#24204,#24205,#24206,#24207,
#24208,#24209,#24210,#24211,#24212,#24213,#24214,#24215,#24216,#24217,#24218,
#24219,#24220,#24221,#24222,#24223,#24224,#24225,#24226,#24227,#24228,#24229,
#24230,#24231,#24232,#24233,#24234,#24235,#24236,#24237,#24238,#24239,#24240,
#24241,#24242,#24243,#24244,#24245,#24246,#24247,#24248,#24249,#24250,#24251,
#24252,#24253,#24254,#24255,#24256,#24257,#24258,#24259,#24260,#24261,#24262,
#24263,#24264,#24265,#24266,#24267,#24268,#24269,#24270,#24271,#24272,#24273,
#24274,#24275,#24276,#24277,#24278,#24279,#24280,#24281,#24282,#24283,#24284,
#24285,#24286,#24287,#24288,#24289,#24290,#24291,#24292,#24293,#24294,#24295,
#24296,#24297,#24298,#24299,#24300,#24301,#24302,#24303,#24304,#24305,#24306,
#24307,#24308,#24309,#24310,#24311,#24312,#24313,#24314,#24315,#24316,#24317,
#24318,#24319,#24320,#24321,#24322,#24323,#24324,#24325,#24326,#24327,#24328,
#24329,#24330,#24331,#24332,#24333,#24334,#24335,#24336,#24337,#24338,#24339,
#24340,#24341,#24342,#24343,#24344,#24345,#24346,#24347,#24348,#24349,#24350,
#24351,#24352));
#24552=CLOSED_SHELL('',(#24353,#24354,#24355,#24356,#24357,#24358,#24359,
#24360,#24361,#24362,#24363,#24364,#24365,#24366,#24367,#24368,#24369,#24370,
#24371,#24372,#24373,#24374,#24375,#24376,#24377,#24378,#24379,#24380,#24381,
#24382,#24383,#24384,#24385,#24386,#24387,#24388,#24389,#24390,#24391,#24392,
#24393));
#24553=CLOSED_SHELL('',(#24394,#24395,#24396,#24397,#24398,#24399,#24400,
#24401,#24402,#24403,#24404,#24405,#24406,#24407,#24408,#24409,#24410,#24411,
#24412,#24413,#24414,#24415,#24416,#24417,#24418,#24419,#24420,#24421));
#24554=CLOSED_SHELL('',(#24422,#24423,#24424,#24425,#24426,#24427,#24428,
#24429,#24430,#24431,#24432,#24433,#24434,#24435,#24436,#24437,#24438,#24439,
#24440,#24441,#24442));
#24555=CLOSED_SHELL('',(#24443,#24444,#24445,#24446));
#24556=CLOSED_SHELL('',(#24447,#24448,#24449,#24450,#24451,#24452));
#24557=CLOSED_SHELL('',(#24453,#24454,#24455,#24456,#24457,#24458,#24459,
#24460,#24461,#24462,#24463,#24464,#24465,#24466));
#24558=CLOSED_SHELL('',(#24467,#24468,#24469,#24470,#24471,#24472,#24473,
#24474,#24475,#24476,#24477,#24478,#24479,#24480,#24481,#24482,#24483,#24484,
#24485,#24486,#24487));
#24559=CLOSED_SHELL('',(#24488,#24489,#24490,#24491));
#24560=CLOSED_SHELL('',(#24492,#24493,#24494,#24495,#24496,#24497));
#24561=CLOSED_SHELL('',(#24498,#24499,#24500,#24501,#24502,#24503,#24504,
#24505,#24506,#24507,#24508,#24509,#24510,#24511));
#24562=CLOSED_SHELL('',(#24512,#24513,#24514,#24515,#24516,#24517,#24518,
#24519,#24520,#24521,#24522,#24523,#24524,#24525));
#24563=DERIVED_UNIT_ELEMENT(#24621,1.);
#24564=DERIVED_UNIT_ELEMENT(#57081,-3.);
#24565=DERIVED_UNIT_ELEMENT(#24621,1.);
#24566=DERIVED_UNIT_ELEMENT(#57081,-3.);
#24567=DERIVED_UNIT_ELEMENT(#24621,1.);
#24568=DERIVED_UNIT_ELEMENT(#57081,-3.);
#24569=DERIVED_UNIT_ELEMENT(#24621,1.);
#24570=DERIVED_UNIT_ELEMENT(#57081,-3.);
#24571=DERIVED_UNIT_ELEMENT(#24621,1.);
#24572=DERIVED_UNIT_ELEMENT(#57081,-3.);
#24573=DERIVED_UNIT_ELEMENT(#24621,1.);
#24574=DERIVED_UNIT_ELEMENT(#57081,-3.);
#24575=DERIVED_UNIT_ELEMENT(#24621,1.);
#24576=DERIVED_UNIT_ELEMENT(#57081,-3.);
#24577=DERIVED_UNIT_ELEMENT(#24621,1.);
#24578=DERIVED_UNIT_ELEMENT(#57081,-3.);
#24579=DERIVED_UNIT_ELEMENT(#24621,1.);
#24580=DERIVED_UNIT_ELEMENT(#57081,-3.);
#24581=DERIVED_UNIT_ELEMENT(#24621,1.);
#24582=DERIVED_UNIT_ELEMENT(#57081,-3.);
#24583=DERIVED_UNIT_ELEMENT(#24621,1.);
#24584=DERIVED_UNIT_ELEMENT(#57081,-3.);
#24585=DERIVED_UNIT_ELEMENT(#24621,1.);
#24586=DERIVED_UNIT_ELEMENT(#57081,-3.);
#24587=DERIVED_UNIT_ELEMENT(#24621,1.);
#24588=DERIVED_UNIT_ELEMENT(#57081,-3.);
#24589=DERIVED_UNIT_ELEMENT(#24621,1.);
#24590=DERIVED_UNIT_ELEMENT(#57081,-3.);
#24591=DERIVED_UNIT_ELEMENT(#24621,1.);
#24592=DERIVED_UNIT_ELEMENT(#57081,-3.);
#24593=DERIVED_UNIT_ELEMENT(#24621,1.);
#24594=DERIVED_UNIT_ELEMENT(#57081,-3.);
#24595=DERIVED_UNIT_ELEMENT(#24621,1.);
#24596=DERIVED_UNIT_ELEMENT(#57081,-3.);
#24597=DERIVED_UNIT_ELEMENT(#24621,1.);
#24598=DERIVED_UNIT_ELEMENT(#57081,-3.);
#24599=DERIVED_UNIT_ELEMENT(#24621,1.);
#24600=DERIVED_UNIT_ELEMENT(#57081,-3.);
#24601=DERIVED_UNIT_ELEMENT(#24621,1.);
#24602=DERIVED_UNIT_ELEMENT(#57081,-3.);
#24603=DERIVED_UNIT_ELEMENT(#24621,1.);
#24604=DERIVED_UNIT_ELEMENT(#57081,-3.);
#24605=DERIVED_UNIT_ELEMENT(#24621,1.);
#24606=DERIVED_UNIT_ELEMENT(#57081,-3.);
#24607=DERIVED_UNIT_ELEMENT(#24621,1.);
#24608=DERIVED_UNIT_ELEMENT(#57081,-3.);
#24609=DERIVED_UNIT_ELEMENT(#24621,1.);
#24610=DERIVED_UNIT_ELEMENT(#57081,-3.);
#24611=DERIVED_UNIT_ELEMENT(#24621,1.);
#24612=DERIVED_UNIT_ELEMENT(#57081,-3.);
#24613=DERIVED_UNIT_ELEMENT(#24621,1.);
#24614=DERIVED_UNIT_ELEMENT(#57081,-3.);
#24615=DERIVED_UNIT_ELEMENT(#24621,1.);
#24616=DERIVED_UNIT_ELEMENT(#57081,-3.);
#24617=DERIVED_UNIT_ELEMENT(#24621,1.);
#24618=DERIVED_UNIT_ELEMENT(#57081,-3.);
#24619=DERIVED_UNIT_ELEMENT(#24621,1.);
#24620=DERIVED_UNIT_ELEMENT(#57081,-3.);
#24621=(
MASS_UNIT()
NAMED_UNIT(*)
SI_UNIT(.KILO.,.GRAM.)
);
#24622=DERIVED_UNIT((#24563,#24564));
#24623=DERIVED_UNIT((#24565,#24566));
#24624=DERIVED_UNIT((#24567,#24568));
#24625=DERIVED_UNIT((#24569,#24570));
#24626=DERIVED_UNIT((#24571,#24572));
#24627=DERIVED_UNIT((#24573,#24574));
#24628=DERIVED_UNIT((#24575,#24576));
#24629=DERIVED_UNIT((#24577,#24578));
#24630=DERIVED_UNIT((#24579,#24580));
#24631=DERIVED_UNIT((#24581,#24582));
#24632=DERIVED_UNIT((#24583,#24584));
#24633=DERIVED_UNIT((#24585,#24586));
#24634=DERIVED_UNIT((#24587,#24588));
#24635=DERIVED_UNIT((#24589,#24590));
#24636=DERIVED_UNIT((#24591,#24592));
#24637=DERIVED_UNIT((#24593,#24594));
#24638=DERIVED_UNIT((#24595,#24596));
#24639=DERIVED_UNIT((#24597,#24598));
#24640=DERIVED_UNIT((#24599,#24600));
#24641=DERIVED_UNIT((#24601,#24602));
#24642=DERIVED_UNIT((#24603,#24604));
#24643=DERIVED_UNIT((#24605,#24606));
#24644=DERIVED_UNIT((#24607,#24608));
#24645=DERIVED_UNIT((#24609,#24610));
#24646=DERIVED_UNIT((#24611,#24612));
#24647=DERIVED_UNIT((#24613,#24614));
#24648=DERIVED_UNIT((#24615,#24616));
#24649=DERIVED_UNIT((#24617,#24618));
#24650=DERIVED_UNIT((#24619,#24620));
#24651=MEASURE_REPRESENTATION_ITEM('density measure',
POSITIVE_RATIO_MEASURE(7850.),#24622);
#24652=MEASURE_REPRESENTATION_ITEM('density measure',
POSITIVE_RATIO_MEASURE(7850.),#24623);
#24653=MEASURE_REPRESENTATION_ITEM('density measure',
POSITIVE_RATIO_MEASURE(7850.),#24624);
#24654=MEASURE_REPRESENTATION_ITEM('density measure',
POSITIVE_RATIO_MEASURE(7850.),#24625);
#24655=MEASURE_REPRESENTATION_ITEM('density measure',
POSITIVE_RATIO_MEASURE(7850.),#24626);
#24656=MEASURE_REPRESENTATION_ITEM('density measure',
POSITIVE_RATIO_MEASURE(7850.),#24627);
#24657=MEASURE_REPRESENTATION_ITEM('density measure',
POSITIVE_RATIO_MEASURE(7850.),#24628);
#24658=MEASURE_REPRESENTATION_ITEM('density measure',
POSITIVE_RATIO_MEASURE(7850.),#24629);
#24659=MEASURE_REPRESENTATION_ITEM('density measure',
POSITIVE_RATIO_MEASURE(7850.),#24630);
#24660=MEASURE_REPRESENTATION_ITEM('density measure',
POSITIVE_RATIO_MEASURE(7850.),#24631);
#24661=MEASURE_REPRESENTATION_ITEM('density measure',
POSITIVE_RATIO_MEASURE(7850.),#24632);
#24662=MEASURE_REPRESENTATION_ITEM('density measure',
POSITIVE_RATIO_MEASURE(7850.),#24633);
#24663=MEASURE_REPRESENTATION_ITEM('density measure',
POSITIVE_RATIO_MEASURE(7850.),#24634);
#24664=MEASURE_REPRESENTATION_ITEM('density measure',
POSITIVE_RATIO_MEASURE(7850.),#24635);
#24665=MEASURE_REPRESENTATION_ITEM('density measure',
POSITIVE_RATIO_MEASURE(7850.),#24636);
#24666=MEASURE_REPRESENTATION_ITEM('density measure',
POSITIVE_RATIO_MEASURE(7850.),#24637);
#24667=MEASURE_REPRESENTATION_ITEM('density measure',
POSITIVE_RATIO_MEASURE(7850.),#24638);
#24668=MEASURE_REPRESENTATION_ITEM('density measure',
POSITIVE_RATIO_MEASURE(7850.),#24639);
#24669=MEASURE_REPRESENTATION_ITEM('density measure',
POSITIVE_RATIO_MEASURE(7850.),#24640);
#24670=MEASURE_REPRESENTATION_ITEM('density measure',
POSITIVE_RATIO_MEASURE(7850.),#24641);
#24671=MEASURE_REPRESENTATION_ITEM('density measure',
POSITIVE_RATIO_MEASURE(7850.),#24642);
#24672=MEASURE_REPRESENTATION_ITEM('density measure',
POSITIVE_RATIO_MEASURE(7850.),#24643);
#24673=MEASURE_REPRESENTATION_ITEM('density measure',
POSITIVE_RATIO_MEASURE(7850.),#24644);
#24674=MEASURE_REPRESENTATION_ITEM('density measure',
POSITIVE_RATIO_MEASURE(7850.),#24645);
#24675=MEASURE_REPRESENTATION_ITEM('density measure',
POSITIVE_RATIO_MEASURE(7850.),#24646);
#24676=MEASURE_REPRESENTATION_ITEM('density measure',
POSITIVE_RATIO_MEASURE(7850.),#24647);
#24677=MEASURE_REPRESENTATION_ITEM('density measure',
POSITIVE_RATIO_MEASURE(7850.),#24648);
#24678=MEASURE_REPRESENTATION_ITEM('density measure',
POSITIVE_RATIO_MEASURE(7850.),#24649);
#24679=MEASURE_REPRESENTATION_ITEM('density measure',
POSITIVE_RATIO_MEASURE(7850.),#24650);
#24680=PROPERTY_DEFINITION_REPRESENTATION(#24825,#24738);
#24681=PROPERTY_DEFINITION_REPRESENTATION(#24826,#24739);
#24682=PROPERTY_DEFINITION_REPRESENTATION(#24827,#24740);
#24683=PROPERTY_DEFINITION_REPRESENTATION(#24828,#24741);
#24684=PROPERTY_DEFINITION_REPRESENTATION(#24829,#24742);
#24685=PROPERTY_DEFINITION_REPRESENTATION(#24830,#24743);
#24686=PROPERTY_DEFINITION_REPRESENTATION(#24831,#24744);
#24687=PROPERTY_DEFINITION_REPRESENTATION(#24832,#24745);
#24688=PROPERTY_DEFINITION_REPRESENTATION(#24833,#24746);
#24689=PROPERTY_DEFINITION_REPRESENTATION(#24834,#24747);
#24690=PROPERTY_DEFINITION_REPRESENTATION(#24835,#24748);
#24691=PROPERTY_DEFINITION_REPRESENTATION(#24836,#24749);
#24692=PROPERTY_DEFINITION_REPRESENTATION(#24837,#24750);
#24693=PROPERTY_DEFINITION_REPRESENTATION(#24838,#24751);
#24694=PROPERTY_DEFINITION_REPRESENTATION(#24839,#24752);
#24695=PROPERTY_DEFINITION_REPRESENTATION(#24840,#24753);
#24696=PROPERTY_DEFINITION_REPRESENTATION(#24841,#24754);
#24697=PROPERTY_DEFINITION_REPRESENTATION(#24842,#24755);
#24698=PROPERTY_DEFINITION_REPRESENTATION(#24843,#24756);
#24699=PROPERTY_DEFINITION_REPRESENTATION(#24844,#24757);
#24700=PROPERTY_DEFINITION_REPRESENTATION(#24845,#24758);
#24701=PROPERTY_DEFINITION_REPRESENTATION(#24846,#24759);
#24702=PROPERTY_DEFINITION_REPRESENTATION(#24847,#24760);
#24703=PROPERTY_DEFINITION_REPRESENTATION(#24848,#24761);
#24704=PROPERTY_DEFINITION_REPRESENTATION(#24849,#24762);
#24705=PROPERTY_DEFINITION_REPRESENTATION(#24850,#24763);
#24706=PROPERTY_DEFINITION_REPRESENTATION(#24851,#24764);
#24707=PROPERTY_DEFINITION_REPRESENTATION(#24852,#24765);
#24708=PROPERTY_DEFINITION_REPRESENTATION(#24853,#24766);
#24709=PROPERTY_DEFINITION_REPRESENTATION(#24854,#24767);
#24710=PROPERTY_DEFINITION_REPRESENTATION(#24855,#24768);
#24711=PROPERTY_DEFINITION_REPRESENTATION(#24856,#24769);
#24712=PROPERTY_DEFINITION_REPRESENTATION(#24857,#24770);
#24713=PROPERTY_DEFINITION_REPRESENTATION(#24858,#24771);
#24714=PROPERTY_DEFINITION_REPRESENTATION(#24859,#24772);
#24715=PROPERTY_DEFINITION_REPRESENTATION(#24860,#24773);
#24716=PROPERTY_DEFINITION_REPRESENTATION(#24861,#24774);
#24717=PROPERTY_DEFINITION_REPRESENTATION(#24862,#24775);
#24718=PROPERTY_DEFINITION_REPRESENTATION(#24863,#24776);
#24719=PROPERTY_DEFINITION_REPRESENTATION(#24864,#24777);
#24720=PROPERTY_DEFINITION_REPRESENTATION(#24865,#24778);
#24721=PROPERTY_DEFINITION_REPRESENTATION(#24866,#24779);
#24722=PROPERTY_DEFINITION_REPRESENTATION(#24867,#24780);
#24723=PROPERTY_DEFINITION_REPRESENTATION(#24868,#24781);
#24724=PROPERTY_DEFINITION_REPRESENTATION(#24869,#24782);
#24725=PROPERTY_DEFINITION_REPRESENTATION(#24870,#24783);
#24726=PROPERTY_DEFINITION_REPRESENTATION(#24871,#24784);
#24727=PROPERTY_DEFINITION_REPRESENTATION(#24872,#24785);
#24728=PROPERTY_DEFINITION_REPRESENTATION(#24873,#24786);
#24729=PROPERTY_DEFINITION_REPRESENTATION(#24874,#24787);
#24730=PROPERTY_DEFINITION_REPRESENTATION(#24875,#24788);
#24731=PROPERTY_DEFINITION_REPRESENTATION(#24876,#24789);
#24732=PROPERTY_DEFINITION_REPRESENTATION(#24877,#24790);
#24733=PROPERTY_DEFINITION_REPRESENTATION(#24878,#24791);
#24734=PROPERTY_DEFINITION_REPRESENTATION(#24879,#24792);
#24735=PROPERTY_DEFINITION_REPRESENTATION(#24880,#24793);
#24736=PROPERTY_DEFINITION_REPRESENTATION(#24881,#24794);
#24737=PROPERTY_DEFINITION_REPRESENTATION(#24882,#24795);
#24738=REPRESENTATION('material name',(#24796),#57042);
#24739=REPRESENTATION('density',(#24651),#57042);
#24740=REPRESENTATION('material name',(#24797),#57045);
#24741=REPRESENTATION('density',(#24652),#57045);
#24742=REPRESENTATION('material name',(#24798),#57046);
#24743=REPRESENTATION('density',(#24653),#57046);
#24744=REPRESENTATION('material name',(#24799),#57048);
#24745=REPRESENTATION('density',(#24654),#57048);
#24746=REPRESENTATION('material name',(#24800),#57049);
#24747=REPRESENTATION('density',(#24655),#57049);
#24748=REPRESENTATION('material name',(#24801),#57050);
#24749=REPRESENTATION('density',(#24656),#57050);
#24750=REPRESENTATION('material name',(#24802),#57052);
#24751=REPRESENTATION('density',(#24657),#57052);
#24752=REPRESENTATION('material name',(#24803),#57053);
#24753=REPRESENTATION('density',(#24658),#57053);
#24754=REPRESENTATION('material name',(#24804),#57054);
#24755=REPRESENTATION('density',(#24659),#57054);
#24756=REPRESENTATION('material name',(#24805),#57055);
#24757=REPRESENTATION('density',(#24660),#57055);
#24758=REPRESENTATION('material name',(#24806),#57056);
#24759=REPRESENTATION('density',(#24661),#57056);
#24760=REPRESENTATION('material name',(#24807),#57059);
#24761=REPRESENTATION('density',(#24662),#57059);
#24762=REPRESENTATION('material name',(#24808),#57060);
#24763=REPRESENTATION('density',(#24663),#57060);
#24764=REPRESENTATION('material name',(#24809),#57061);
#24765=REPRESENTATION('density',(#24664),#57061);
#24766=REPRESENTATION('material name',(#24810),#57062);
#24767=REPRESENTATION('density',(#24665),#57062);
#24768=REPRESENTATION('material name',(#24811),#57063);
#24769=REPRESENTATION('density',(#24666),#57063);
#24770=REPRESENTATION('material name',(#24812),#57065);
#24771=REPRESENTATION('density',(#24667),#57065);
#24772=REPRESENTATION('material name',(#24813),#57066);
#24773=REPRESENTATION('density',(#24668),#57066);
#24774=REPRESENTATION('material name',(#24814),#57067);
#24775=REPRESENTATION('density',(#24669),#57067);
#24776=REPRESENTATION('material name',(#24815),#57068);
#24777=REPRESENTATION('density',(#24670),#57068);
#24778=REPRESENTATION('material name',(#24816),#57070);
#24779=REPRESENTATION('density',(#24671),#57070);
#24780=REPRESENTATION('material name',(#24817),#57071);
#24781=REPRESENTATION('density',(#24672),#57071);
#24782=REPRESENTATION('material name',(#24818),#57072);
#24783=REPRESENTATION('density',(#24673),#57072);
#24784=REPRESENTATION('material name',(#24819),#57073);
#24785=REPRESENTATION('density',(#24674),#57073);
#24786=REPRESENTATION('material name',(#24820),#57074);
#24787=REPRESENTATION('density',(#24675),#57074);
#24788=REPRESENTATION('material name',(#24821),#57075);
#24789=REPRESENTATION('density',(#24676),#57075);
#24790=REPRESENTATION('material name',(#24822),#57076);
#24791=REPRESENTATION('density',(#24677),#57076);
#24792=REPRESENTATION('material name',(#24823),#57077);
#24793=REPRESENTATION('density',(#24678),#57077);
#24794=REPRESENTATION('material name',(#24824),#57078);
#24795=REPRESENTATION('density',(#24679),#57078);
#24796=DESCRIPTIVE_REPRESENTATION_ITEM('Steel','Steel');
#24797=DESCRIPTIVE_REPRESENTATION_ITEM('Steel','Steel');
#24798=DESCRIPTIVE_REPRESENTATION_ITEM('Steel','Steel');
#24799=DESCRIPTIVE_REPRESENTATION_ITEM('Steel','Steel');
#24800=DESCRIPTIVE_REPRESENTATION_ITEM('Steel','Steel');
#24801=DESCRIPTIVE_REPRESENTATION_ITEM('Steel','Steel');
#24802=DESCRIPTIVE_REPRESENTATION_ITEM('Steel','Steel');
#24803=DESCRIPTIVE_REPRESENTATION_ITEM('Steel','Steel');
#24804=DESCRIPTIVE_REPRESENTATION_ITEM('Steel','Steel');
#24805=DESCRIPTIVE_REPRESENTATION_ITEM('Steel','Steel');
#24806=DESCRIPTIVE_REPRESENTATION_ITEM('Steel','Steel');
#24807=DESCRIPTIVE_REPRESENTATION_ITEM('Steel','Steel');
#24808=DESCRIPTIVE_REPRESENTATION_ITEM('Steel','Steel');
#24809=DESCRIPTIVE_REPRESENTATION_ITEM('Steel','Steel');
#24810=DESCRIPTIVE_REPRESENTATION_ITEM('Steel','Steel');
#24811=DESCRIPTIVE_REPRESENTATION_ITEM('Steel','Steel');
#24812=DESCRIPTIVE_REPRESENTATION_ITEM('Steel','Steel');
#24813=DESCRIPTIVE_REPRESENTATION_ITEM('Steel','Steel');
#24814=DESCRIPTIVE_REPRESENTATION_ITEM('Steel','Steel');
#24815=DESCRIPTIVE_REPRESENTATION_ITEM('Steel','Steel');
#24816=DESCRIPTIVE_REPRESENTATION_ITEM('Steel','Steel');
#24817=DESCRIPTIVE_REPRESENTATION_ITEM('Steel','Steel');
#24818=DESCRIPTIVE_REPRESENTATION_ITEM('Steel','Steel');
#24819=DESCRIPTIVE_REPRESENTATION_ITEM('Steel','Steel');
#24820=DESCRIPTIVE_REPRESENTATION_ITEM('Steel','Steel');
#24821=DESCRIPTIVE_REPRESENTATION_ITEM('Steel','Steel');
#24822=DESCRIPTIVE_REPRESENTATION_ITEM('Steel','Steel');
#24823=DESCRIPTIVE_REPRESENTATION_ITEM('Steel','Steel');
#24824=DESCRIPTIVE_REPRESENTATION_ITEM('Steel','Steel');
#24825=PROPERTY_DEFINITION('material property','material name',#57289);
#24826=PROPERTY_DEFINITION('material property','density of part',#57289);
#24827=PROPERTY_DEFINITION('material property','material name',#57292);
#24828=PROPERTY_DEFINITION('material property','density of part',#57292);
#24829=PROPERTY_DEFINITION('material property','material name',#57293);
#24830=PROPERTY_DEFINITION('material property','density of part',#57293);
#24831=PROPERTY_DEFINITION('material property','material name',#57295);
#24832=PROPERTY_DEFINITION('material property','density of part',#57295);
#24833=PROPERTY_DEFINITION('material property','material name',#57296);
#24834=PROPERTY_DEFINITION('material property','density of part',#57296);
#24835=PROPERTY_DEFINITION('material property','material name',#57297);
#24836=PROPERTY_DEFINITION('material property','density of part',#57297);
#24837=PROPERTY_DEFINITION('material property','material name',#57299);
#24838=PROPERTY_DEFINITION('material property','density of part',#57299);
#24839=PROPERTY_DEFINITION('material property','material name',#57300);
#24840=PROPERTY_DEFINITION('material property','density of part',#57300);
#24841=PROPERTY_DEFINITION('material property','material name',#57301);
#24842=PROPERTY_DEFINITION('material property','density of part',#57301);
#24843=PROPERTY_DEFINITION('material property','material name',#57302);
#24844=PROPERTY_DEFINITION('material property','density of part',#57302);
#24845=PROPERTY_DEFINITION('material property','material name',#57303);
#24846=PROPERTY_DEFINITION('material property','density of part',#57303);
#24847=PROPERTY_DEFINITION('material property','material name',#57306);
#24848=PROPERTY_DEFINITION('material property','density of part',#57306);
#24849=PROPERTY_DEFINITION('material property','material name',#57307);
#24850=PROPERTY_DEFINITION('material property','density of part',#57307);
#24851=PROPERTY_DEFINITION('material property','material name',#57308);
#24852=PROPERTY_DEFINITION('material property','density of part',#57308);
#24853=PROPERTY_DEFINITION('material property','material name',#57309);
#24854=PROPERTY_DEFINITION('material property','density of part',#57309);
#24855=PROPERTY_DEFINITION('material property','material name',#57310);
#24856=PROPERTY_DEFINITION('material property','density of part',#57310);
#24857=PROPERTY_DEFINITION('material property','material name',#57312);
#24858=PROPERTY_DEFINITION('material property','density of part',#57312);
#24859=PROPERTY_DEFINITION('material property','material name',#57313);
#24860=PROPERTY_DEFINITION('material property','density of part',#57313);
#24861=PROPERTY_DEFINITION('material property','material name',#57314);
#24862=PROPERTY_DEFINITION('material property','density of part',#57314);
#24863=PROPERTY_DEFINITION('material property','material name',#57315);
#24864=PROPERTY_DEFINITION('material property','density of part',#57315);
#24865=PROPERTY_DEFINITION('material property','material name',#57317);
#24866=PROPERTY_DEFINITION('material property','density of part',#57317);
#24867=PROPERTY_DEFINITION('material property','material name',#57318);
#24868=PROPERTY_DEFINITION('material property','density of part',#57318);
#24869=PROPERTY_DEFINITION('material property','material name',#57319);
#24870=PROPERTY_DEFINITION('material property','density of part',#57319);
#24871=PROPERTY_DEFINITION('material property','material name',#57320);
#24872=PROPERTY_DEFINITION('material property','density of part',#57320);
#24873=PROPERTY_DEFINITION('material property','material name',#57321);
#24874=PROPERTY_DEFINITION('material property','density of part',#57321);
#24875=PROPERTY_DEFINITION('material property','material name',#57322);
#24876=PROPERTY_DEFINITION('material property','density of part',#57322);
#24877=PROPERTY_DEFINITION('material property','material name',#57323);
#24878=PROPERTY_DEFINITION('material property','density of part',#57323);
#24879=PROPERTY_DEFINITION('material property','material name',#57324);
#24880=PROPERTY_DEFINITION('material property','density of part',#57324);
#24881=PROPERTY_DEFINITION('material property','material name',#57325);
#24882=PROPERTY_DEFINITION('material property','density of part',#57325);
#24883=AXIS2_PLACEMENT_3D('',#34632,#27477,#27478);
#24884=AXIS2_PLACEMENT_3D('',#34633,#27479,#27480);
#24885=AXIS2_PLACEMENT_3D('',#34634,#27481,#27482);
#24886=AXIS2_PLACEMENT_3D('',#34636,#27483,#27484);
#24887=AXIS2_PLACEMENT_3D('',#34639,#27486,#27487);
#24888=AXIS2_PLACEMENT_3D('',#34640,#27488,#27489);
#24889=AXIS2_PLACEMENT_3D('',#34642,#27490,#27491);
#24890=AXIS2_PLACEMENT_3D('',#34645,#27493,#27494);
#24891=AXIS2_PLACEMENT_3D('',#34646,#27495,#27496);
#24892=AXIS2_PLACEMENT_3D('',#34648,#27497,#27498);
#24893=AXIS2_PLACEMENT_3D('',#34651,#27500,#27501);
#24894=AXIS2_PLACEMENT_3D('',#34652,#27502,#27503);
#24895=AXIS2_PLACEMENT_3D('',#34654,#27504,#27505);
#24896=AXIS2_PLACEMENT_3D('',#34657,#27507,#27508);
#24897=AXIS2_PLACEMENT_3D('',#34658,#27509,#27510);
#24898=AXIS2_PLACEMENT_3D('',#34660,#27511,#27512);
#24899=AXIS2_PLACEMENT_3D('',#34663,#27514,#27515);
#24900=AXIS2_PLACEMENT_3D('',#34664,#27516,#27517);
#24901=AXIS2_PLACEMENT_3D('',#34666,#27518,#27519);
#24902=AXIS2_PLACEMENT_3D('',#34669,#27521,#27522);
#24903=AXIS2_PLACEMENT_3D('',#34670,#27523,#27524);
#24904=AXIS2_PLACEMENT_3D('',#34672,#27525,#27526);
#24905=AXIS2_PLACEMENT_3D('',#34675,#27528,#27529);
#24906=AXIS2_PLACEMENT_3D('',#34676,#27530,#27531);
#24907=AXIS2_PLACEMENT_3D('',#34678,#27532,#27533);
#24908=AXIS2_PLACEMENT_3D('',#34681,#27535,#27536);
#24909=AXIS2_PLACEMENT_3D('',#34682,#27537,#27538);
#24910=AXIS2_PLACEMENT_3D('',#34684,#27539,#27540);
#24911=AXIS2_PLACEMENT_3D('',#34687,#27542,#27543);
#24912=AXIS2_PLACEMENT_3D('',#34688,#27544,#27545);
#24913=AXIS2_PLACEMENT_3D('',#34691,#27547,#27548);
#24914=AXIS2_PLACEMENT_3D('',#34693,#27549,#27550);
#24915=AXIS2_PLACEMENT_3D('',#34696,#27552,#27553);
#24916=AXIS2_PLACEMENT_3D('',#34697,#27554,#27555);
#24917=AXIS2_PLACEMENT_3D('',#34700,#27557,#27558);
#24918=AXIS2_PLACEMENT_3D('',#34702,#27559,#27560);
#24919=AXIS2_PLACEMENT_3D('',#34705,#27562,#27563);
#24920=AXIS2_PLACEMENT_3D('',#34706,#27564,#27565);
#24921=AXIS2_PLACEMENT_3D('',#34709,#27567,#27568);
#24922=AXIS2_PLACEMENT_3D('',#34711,#27569,#27570);
#24923=AXIS2_PLACEMENT_3D('',#34714,#27572,#27573);
#24924=AXIS2_PLACEMENT_3D('',#34715,#27574,#27575);
#24925=AXIS2_PLACEMENT_3D('',#34718,#27577,#27578);
#24926=AXIS2_PLACEMENT_3D('',#34727,#27583,#27584);
#24927=AXIS2_PLACEMENT_3D('',#34736,#27589,#27590);
#24928=AXIS2_PLACEMENT_3D('',#34742,#27594,#27595);
#24929=AXIS2_PLACEMENT_3D('',#34745,#27598,#27599);
#24930=AXIS2_PLACEMENT_3D('',#34751,#27603,#27604);
#24931=AXIS2_PLACEMENT_3D('',#34757,#27608,#27609);
#24932=AXIS2_PLACEMENT_3D('',#34763,#27613,#27614);
#24933=AXIS2_PLACEMENT_3D('',#34765,#27616,#27617);
#24934=AXIS2_PLACEMENT_3D('',#34767,#27619,#27620);
#24935=AXIS2_PLACEMENT_3D('',#34768,#27621,#27622);
#24936=AXIS2_PLACEMENT_3D('',#34769,#27623,#27624);
#24937=AXIS2_PLACEMENT_3D('',#34770,#27625,#27626);
#24938=AXIS2_PLACEMENT_3D('',#34771,#27627,#27628);
#24939=AXIS2_PLACEMENT_3D('',#34773,#27629,#27630);
#24940=AXIS2_PLACEMENT_3D('',#34777,#27632,#27633);
#24941=AXIS2_PLACEMENT_3D('',#34801,#27636,#27637);
#24942=AXIS2_PLACEMENT_3D('',#34802,#27638,#27639);
#24943=AXIS2_PLACEMENT_3D('',#34804,#27640,#27641);
#24944=AXIS2_PLACEMENT_3D('',#34805,#27642,#27643);
#24945=AXIS2_PLACEMENT_3D('',#34806,#27644,#27645);
#24946=AXIS2_PLACEMENT_3D('',#34808,#27646,#27647);
#24947=AXIS2_PLACEMENT_3D('',#34811,#27649,#27650);
#24948=AXIS2_PLACEMENT_3D('',#34812,#27651,#27652);
#24949=AXIS2_PLACEMENT_3D('',#34814,#27653,#27654);
#24950=AXIS2_PLACEMENT_3D('',#34816,#27656,#27657);
#24951=AXIS2_PLACEMENT_3D('',#34818,#27658,#27659);
#24952=AXIS2_PLACEMENT_3D('',#34819,#27660,#27661);
#24953=AXIS2_PLACEMENT_3D('',#34820,#27662,#27663);
#24954=AXIS2_PLACEMENT_3D('',#34822,#27664,#27665);
#24955=AXIS2_PLACEMENT_3D('',#34825,#27667,#27668);
#24956=AXIS2_PLACEMENT_3D('',#34826,#27669,#27670);
#24957=AXIS2_PLACEMENT_3D('',#34829,#27671,#27672);
#24958=AXIS2_PLACEMENT_3D('',#34830,#27673,#27674);
#24959=AXIS2_PLACEMENT_3D('',#34832,#27676,#27677);
#24960=AXIS2_PLACEMENT_3D('',#34835,#27679,#27680);
#24961=AXIS2_PLACEMENT_3D('',#34836,#27681,#27682);
#24962=AXIS2_PLACEMENT_3D('',#34838,#27683,#27684);
#24963=AXIS2_PLACEMENT_3D('',#34840,#27685,#27686);
#24964=AXIS2_PLACEMENT_3D('',#34841,#27687,#27688);
#24965=AXIS2_PLACEMENT_3D('',#34842,#27689,#27690);
#24966=AXIS2_PLACEMENT_3D('',#34844,#27691,#27692);
#24967=AXIS2_PLACEMENT_3D('',#34846,#27694,#27695);
#24968=AXIS2_PLACEMENT_3D('',#34848,#27696,#27697);
#24969=AXIS2_PLACEMENT_3D('',#34851,#27699,#27700);
#24970=AXIS2_PLACEMENT_3D('',#34852,#27701,#27702);
#24971=AXIS2_PLACEMENT_3D('',#34855,#27703,#27704);
#24972=AXIS2_PLACEMENT_3D('',#34856,#27705,#27706);
#24973=AXIS2_PLACEMENT_3D('',#34859,#27708,#27709);
#24974=AXIS2_PLACEMENT_3D('',#34860,#27710,#27711);
#24975=AXIS2_PLACEMENT_3D('',#34863,#27713,#27714);
#24976=AXIS2_PLACEMENT_3D('',#34864,#27715,#27716);
#24977=AXIS2_PLACEMENT_3D('',#34865,#27717,#27718);
#24978=AXIS2_PLACEMENT_3D('',#34866,#27719,#27720);
#24979=AXIS2_PLACEMENT_3D('',#34867,#27721,#27722);
#24980=AXIS2_PLACEMENT_3D('',#34868,#27723,#27724);
#24981=AXIS2_PLACEMENT_3D('',#34869,#27725,#27726);
#24982=AXIS2_PLACEMENT_3D('',#34876,#27727,#27728);
#24983=AXIS2_PLACEMENT_3D('',#34881,#27729,#27730);
#24984=AXIS2_PLACEMENT_3D('',#34887,#27734,#27735);
#24985=AXIS2_PLACEMENT_3D('',#34888,#27736,#27737);
#24986=AXIS2_PLACEMENT_3D('',#34892,#27740,#27741);
#24987=AXIS2_PLACEMENT_3D('',#34896,#27744,#27745);
#24988=AXIS2_PLACEMENT_3D('',#34897,#27746,#27747);
#24989=AXIS2_PLACEMENT_3D('',#34898,#27748,#27749);
#24990=AXIS2_PLACEMENT_3D('',#34899,#27750,#27751);
#24991=AXIS2_PLACEMENT_3D('',#34900,#27752,#27753);
#24992=AXIS2_PLACEMENT_3D('',#34972,#27755,#27756);
#24993=AXIS2_PLACEMENT_3D('',#34974,#27757,#27758);
#24994=AXIS2_PLACEMENT_3D('',#34977,#27760,#27761);
#24995=AXIS2_PLACEMENT_3D('',#34978,#27762,#27763);
#24996=AXIS2_PLACEMENT_3D('',#34980,#27764,#27765);
#24997=AXIS2_PLACEMENT_3D('',#34983,#27767,#27768);
#24998=AXIS2_PLACEMENT_3D('',#34984,#27769,#27770);
#24999=AXIS2_PLACEMENT_3D('',#34986,#27771,#27772);
#25000=AXIS2_PLACEMENT_3D('',#34989,#27774,#27775);
#25001=AXIS2_PLACEMENT_3D('',#34990,#27776,#27777);
#25002=AXIS2_PLACEMENT_3D('',#34992,#27778,#27779);
#25003=AXIS2_PLACEMENT_3D('',#34995,#27781,#27782);
#25004=AXIS2_PLACEMENT_3D('',#34996,#27783,#27784);
#25005=AXIS2_PLACEMENT_3D('',#34998,#27785,#27786);
#25006=AXIS2_PLACEMENT_3D('',#35001,#27788,#27789);
#25007=AXIS2_PLACEMENT_3D('',#35002,#27790,#27791);
#25008=AXIS2_PLACEMENT_3D('',#35004,#27792,#27793);
#25009=AXIS2_PLACEMENT_3D('',#35007,#27795,#27796);
#25010=AXIS2_PLACEMENT_3D('',#35008,#27797,#27798);
#25011=AXIS2_PLACEMENT_3D('',#35010,#27799,#27800);
#25012=AXIS2_PLACEMENT_3D('',#35013,#27802,#27803);
#25013=AXIS2_PLACEMENT_3D('',#35014,#27804,#27805);
#25014=AXIS2_PLACEMENT_3D('',#35016,#27806,#27807);
#25015=AXIS2_PLACEMENT_3D('',#35019,#27809,#27810);
#25016=AXIS2_PLACEMENT_3D('',#35020,#27811,#27812);
#25017=AXIS2_PLACEMENT_3D('',#35022,#27813,#27814);
#25018=AXIS2_PLACEMENT_3D('',#35025,#27816,#27817);
#25019=AXIS2_PLACEMENT_3D('',#35026,#27818,#27819);
#25020=AXIS2_PLACEMENT_3D('',#35028,#27820,#27821);
#25021=AXIS2_PLACEMENT_3D('',#35031,#27823,#27824);
#25022=AXIS2_PLACEMENT_3D('',#35032,#27825,#27826);
#25023=AXIS2_PLACEMENT_3D('',#35034,#27827,#27828);
#25024=AXIS2_PLACEMENT_3D('',#35037,#27830,#27831);
#25025=AXIS2_PLACEMENT_3D('',#35038,#27832,#27833);
#25026=AXIS2_PLACEMENT_3D('',#35040,#27834,#27835);
#25027=AXIS2_PLACEMENT_3D('',#35043,#27837,#27838);
#25028=AXIS2_PLACEMENT_3D('',#35044,#27839,#27840);
#25029=AXIS2_PLACEMENT_3D('',#35046,#27841,#27842);
#25030=AXIS2_PLACEMENT_3D('',#35047,#27843,#27844);
#25031=AXIS2_PLACEMENT_3D('',#35048,#27845,#27846);
#25032=AXIS2_PLACEMENT_3D('',#35053,#27848,#27849);
#25033=AXIS2_PLACEMENT_3D('',#35056,#27851,#27852);
#25034=AXIS2_PLACEMENT_3D('',#35057,#27853,#27854);
#25035=AXIS2_PLACEMENT_3D('',#35070,#27855,#27856);
#25036=AXIS2_PLACEMENT_3D('',#35081,#27857,#27858);
#25037=AXIS2_PLACEMENT_3D('',#35104,#27859,#27860);
#25038=AXIS2_PLACEMENT_3D('',#35105,#27861,#27862);
#25039=AXIS2_PLACEMENT_3D('',#35109,#27864,#27865);
#25040=AXIS2_PLACEMENT_3D('',#35111,#27867,#27868);
#25041=AXIS2_PLACEMENT_3D('',#35116,#27871,#27872);
#25042=AXIS2_PLACEMENT_3D('',#35117,#27873,#27874);
#25043=AXIS2_PLACEMENT_3D('',#35130,#27875,#27876);
#25044=AXIS2_PLACEMENT_3D('',#35141,#27877,#27878);
#25045=AXIS2_PLACEMENT_3D('',#35164,#27879,#27880);
#25046=AXIS2_PLACEMENT_3D('',#35165,#27881,#27882);
#25047=AXIS2_PLACEMENT_3D('',#35168,#27885,#27886);
#25048=AXIS2_PLACEMENT_3D('',#35169,#27887,#27888);
#25049=AXIS2_PLACEMENT_3D('',#35170,#27889,#27890);
#25050=AXIS2_PLACEMENT_3D('',#35171,#27891,#27892);
#25051=AXIS2_PLACEMENT_3D('',#35172,#27893,#27894);
#25052=AXIS2_PLACEMENT_3D('',#35173,#27895,#27896);
#25053=AXIS2_PLACEMENT_3D('',#35174,#27897,#27898);
#25054=AXIS2_PLACEMENT_3D('',#35175,#27899,#27900);
#25055=AXIS2_PLACEMENT_3D('',#35176,#27901,#27902);
#25056=AXIS2_PLACEMENT_3D('',#35177,#27903,#27904);
#25057=AXIS2_PLACEMENT_3D('',#35178,#27905,#27906);
#25058=AXIS2_PLACEMENT_3D('',#35179,#27907,#27908);
#25059=AXIS2_PLACEMENT_3D('',#35181,#27909,#27910);
#25060=AXIS2_PLACEMENT_3D('',#35184,#27912,#27913);
#25061=AXIS2_PLACEMENT_3D('',#35185,#27914,#27915);
#25062=AXIS2_PLACEMENT_3D('',#35187,#27916,#27917);
#25063=AXIS2_PLACEMENT_3D('',#35190,#27919,#27920);
#25064=AXIS2_PLACEMENT_3D('',#35191,#27921,#27922);
#25065=AXIS2_PLACEMENT_3D('',#35193,#27923,#27924);
#25066=AXIS2_PLACEMENT_3D('',#35196,#27926,#27927);
#25067=AXIS2_PLACEMENT_3D('',#35197,#27928,#27929);
#25068=AXIS2_PLACEMENT_3D('',#35199,#27930,#27931);
#25069=AXIS2_PLACEMENT_3D('',#35202,#27933,#27934);
#25070=AXIS2_PLACEMENT_3D('',#35203,#27935,#27936);
#25071=AXIS2_PLACEMENT_3D('',#35205,#27937,#27938);
#25072=AXIS2_PLACEMENT_3D('',#35208,#27940,#27941);
#25073=AXIS2_PLACEMENT_3D('',#35209,#27942,#27943);
#25074=AXIS2_PLACEMENT_3D('',#35211,#27944,#27945);
#25075=AXIS2_PLACEMENT_3D('',#35214,#27947,#27948);
#25076=AXIS2_PLACEMENT_3D('',#35215,#27949,#27950);
#25077=AXIS2_PLACEMENT_3D('',#35217,#27951,#27952);
#25078=AXIS2_PLACEMENT_3D('',#35220,#27954,#27955);
#25079=AXIS2_PLACEMENT_3D('',#35221,#27956,#27957);
#25080=AXIS2_PLACEMENT_3D('',#35226,#27959,#27960);
#25081=AXIS2_PLACEMENT_3D('',#35228,#27961,#27962);
#25082=AXIS2_PLACEMENT_3D('',#35230,#27963,#27964);
#25083=AXIS2_PLACEMENT_3D('',#35232,#27965,#27966);
#25084=AXIS2_PLACEMENT_3D('',#35234,#27967,#27968);
#25085=AXIS2_PLACEMENT_3D('',#35235,#27969,#27970);
#25086=AXIS2_PLACEMENT_3D('',#35236,#27971,#27972);
#25087=AXIS2_PLACEMENT_3D('',#35241,#27974,#27975);
#25088=AXIS2_PLACEMENT_3D('',#35243,#27976,#27977);
#25089=AXIS2_PLACEMENT_3D('',#35245,#27978,#27979);
#25090=AXIS2_PLACEMENT_3D('',#35247,#27980,#27981);
#25091=AXIS2_PLACEMENT_3D('',#35249,#27982,#27983);
#25092=AXIS2_PLACEMENT_3D('',#35250,#27984,#27985);
#25093=AXIS2_PLACEMENT_3D('',#35251,#27986,#27987);
#25094=AXIS2_PLACEMENT_3D('',#35256,#27989,#27990);
#25095=AXIS2_PLACEMENT_3D('',#35258,#27991,#27992);
#25096=AXIS2_PLACEMENT_3D('',#35260,#27993,#27994);
#25097=AXIS2_PLACEMENT_3D('',#35262,#27995,#27996);
#25098=AXIS2_PLACEMENT_3D('',#35264,#27997,#27998);
#25099=AXIS2_PLACEMENT_3D('',#35265,#27999,#28000);
#25100=AXIS2_PLACEMENT_3D('',#35266,#28001,#28002);
#25101=AXIS2_PLACEMENT_3D('',#35271,#28004,#28005);
#25102=AXIS2_PLACEMENT_3D('',#35273,#28006,#28007);
#25103=AXIS2_PLACEMENT_3D('',#35275,#28008,#28009);
#25104=AXIS2_PLACEMENT_3D('',#35277,#28010,#28011);
#25105=AXIS2_PLACEMENT_3D('',#35279,#28012,#28013);
#25106=AXIS2_PLACEMENT_3D('',#35280,#28014,#28015);
#25107=AXIS2_PLACEMENT_3D('',#35281,#28016,#28017);
#25108=AXIS2_PLACEMENT_3D('',#35283,#28018,#28019);
#25109=AXIS2_PLACEMENT_3D('',#35286,#28021,#28022);
#25110=AXIS2_PLACEMENT_3D('',#35287,#28023,#28024);
#25111=AXIS2_PLACEMENT_3D('',#35289,#28025,#28026);
#25112=AXIS2_PLACEMENT_3D('',#35292,#28028,#28029);
#25113=AXIS2_PLACEMENT_3D('',#35293,#28030,#28031);
#25114=AXIS2_PLACEMENT_3D('',#35295,#28032,#28033);
#25115=AXIS2_PLACEMENT_3D('',#35298,#28035,#28036);
#25116=AXIS2_PLACEMENT_3D('',#35299,#28037,#28038);
#25117=AXIS2_PLACEMENT_3D('',#35301,#28039,#28040);
#25118=AXIS2_PLACEMENT_3D('',#35304,#28042,#28043);
#25119=AXIS2_PLACEMENT_3D('',#35305,#28044,#28045);
#25120=AXIS2_PLACEMENT_3D('',#35307,#28046,#28047);
#25121=AXIS2_PLACEMENT_3D('',#35310,#28049,#28050);
#25122=AXIS2_PLACEMENT_3D('',#35311,#28051,#28052);
#25123=AXIS2_PLACEMENT_3D('',#35313,#28053,#28054);
#25124=AXIS2_PLACEMENT_3D('',#35316,#28056,#28057);
#25125=AXIS2_PLACEMENT_3D('',#35317,#28058,#28059);
#25126=AXIS2_PLACEMENT_3D('',#35319,#28060,#28061);
#25127=AXIS2_PLACEMENT_3D('',#35322,#28063,#28064);
#25128=AXIS2_PLACEMENT_3D('',#35323,#28065,#28066);
#25129=AXIS2_PLACEMENT_3D('',#35325,#28067,#28068);
#25130=AXIS2_PLACEMENT_3D('',#35328,#28070,#28071);
#25131=AXIS2_PLACEMENT_3D('',#35329,#28072,#28073);
#25132=AXIS2_PLACEMENT_3D('',#35330,#28074,#28075);
#25133=AXIS2_PLACEMENT_3D('',#35331,#28076,#28077);
#25134=AXIS2_PLACEMENT_3D('',#35332,#28078,#28079);
#25135=AXIS2_PLACEMENT_3D('',#35333,#28080,#28081);
#25136=AXIS2_PLACEMENT_3D('',#35374,#28102,#28103);
#25137=AXIS2_PLACEMENT_3D('',#35380,#28107,#28108);
#25138=AXIS2_PLACEMENT_3D('',#35384,#28111,#28112);
#25139=AXIS2_PLACEMENT_3D('',#35388,#28115,#28116);
#25140=AXIS2_PLACEMENT_3D('',#35392,#28119,#28120);
#25141=AXIS2_PLACEMENT_3D('',#35396,#28123,#28124);
#25142=AXIS2_PLACEMENT_3D('',#35400,#28127,#28128);
#25143=AXIS2_PLACEMENT_3D('',#35404,#28131,#28132);
#25144=AXIS2_PLACEMENT_3D('',#35408,#28135,#28136);
#25145=AXIS2_PLACEMENT_3D('',#35412,#28139,#28140);
#25146=AXIS2_PLACEMENT_3D('',#35416,#28143,#28144);
#25147=AXIS2_PLACEMENT_3D('',#35420,#28147,#28148);
#25148=AXIS2_PLACEMENT_3D('',#35422,#28150,#28151);
#25149=AXIS2_PLACEMENT_3D('',#35423,#28152,#28153);
#25150=AXIS2_PLACEMENT_3D('',#35440,#28162,#28163);
#25151=AXIS2_PLACEMENT_3D('',#35443,#28166,#28167);
#25152=AXIS2_PLACEMENT_3D('',#35445,#28169,#28170);
#25153=AXIS2_PLACEMENT_3D('',#35447,#28172,#28173);
#25154=AXIS2_PLACEMENT_3D('',#35449,#28175,#28176);
#25155=AXIS2_PLACEMENT_3D('',#35451,#28178,#28179);
#25156=AXIS2_PLACEMENT_3D('',#35453,#28181,#28182);
#25157=AXIS2_PLACEMENT_3D('',#35455,#28184,#28185);
#25158=AXIS2_PLACEMENT_3D('',#35456,#28186,#28187);
#25159=AXIS2_PLACEMENT_3D('',#35469,#28194,#28195);
#25160=AXIS2_PLACEMENT_3D('',#35482,#28202,#28203);
#25161=AXIS2_PLACEMENT_3D('',#35495,#28210,#28211);
#25162=AXIS2_PLACEMENT_3D('',#35508,#28218,#28219);
#25163=AXIS2_PLACEMENT_3D('',#35515,#28224,#28225);
#25164=AXIS2_PLACEMENT_3D('',#35520,#28229,#28230);
#25165=AXIS2_PLACEMENT_3D('',#35525,#28234,#28235);
#25166=AXIS2_PLACEMENT_3D('',#35530,#28239,#28240);
#25167=AXIS2_PLACEMENT_3D('',#35535,#28244,#28245);
#25168=AXIS2_PLACEMENT_3D('',#35538,#28248,#28249);
#25169=AXIS2_PLACEMENT_3D('',#35539,#28250,#28251);
#25170=AXIS2_PLACEMENT_3D('',#35540,#28252,#28253);
#25171=AXIS2_PLACEMENT_3D('',#35541,#28254,#28255);
#25172=AXIS2_PLACEMENT_3D('',#35542,#28256,#28257);
#25173=AXIS2_PLACEMENT_3D('',#35543,#28258,#28259);
#25174=AXIS2_PLACEMENT_3D('',#35544,#28260,#28261);
#25175=AXIS2_PLACEMENT_3D('',#35551,#28266,#28267);
#25176=AXIS2_PLACEMENT_3D('',#35556,#28271,#28272);
#25177=AXIS2_PLACEMENT_3D('',#35561,#28276,#28277);
#25178=AXIS2_PLACEMENT_3D('',#35566,#28281,#28282);
#25179=AXIS2_PLACEMENT_3D('',#35571,#28286,#28287);
#25180=AXIS2_PLACEMENT_3D('',#35574,#28290,#28291);
#25181=AXIS2_PLACEMENT_3D('',#35575,#28292,#28293);
#25182=AXIS2_PLACEMENT_3D('',#35576,#28294,#28295);
#25183=AXIS2_PLACEMENT_3D('',#35577,#28296,#28297);
#25184=AXIS2_PLACEMENT_3D('',#35578,#28298,#28299);
#25185=AXIS2_PLACEMENT_3D('',#35579,#28300,#28301);
#25186=AXIS2_PLACEMENT_3D('',#35580,#28302,#28303);
#25187=AXIS2_PLACEMENT_3D('',#35587,#28308,#28309);
#25188=AXIS2_PLACEMENT_3D('',#35592,#28313,#28314);
#25189=AXIS2_PLACEMENT_3D('',#35597,#28318,#28319);
#25190=AXIS2_PLACEMENT_3D('',#35602,#28323,#28324);
#25191=AXIS2_PLACEMENT_3D('',#35607,#28328,#28329);
#25192=AXIS2_PLACEMENT_3D('',#35610,#28332,#28333);
#25193=AXIS2_PLACEMENT_3D('',#35611,#28334,#28335);
#25194=AXIS2_PLACEMENT_3D('',#35612,#28336,#28337);
#25195=AXIS2_PLACEMENT_3D('',#35613,#28338,#28339);
#25196=AXIS2_PLACEMENT_3D('',#35614,#28340,#28341);
#25197=AXIS2_PLACEMENT_3D('',#35615,#28342,#28343);
#25198=AXIS2_PLACEMENT_3D('',#35616,#28344,#28345);
#25199=AXIS2_PLACEMENT_3D('',#35623,#28350,#28351);
#25200=AXIS2_PLACEMENT_3D('',#35628,#28355,#28356);
#25201=AXIS2_PLACEMENT_3D('',#35633,#28360,#28361);
#25202=AXIS2_PLACEMENT_3D('',#35638,#28365,#28366);
#25203=AXIS2_PLACEMENT_3D('',#35643,#28370,#28371);
#25204=AXIS2_PLACEMENT_3D('',#35646,#28374,#28375);
#25205=AXIS2_PLACEMENT_3D('',#35647,#28376,#28377);
#25206=AXIS2_PLACEMENT_3D('',#35648,#28378,#28379);
#25207=AXIS2_PLACEMENT_3D('',#35649,#28380,#28381);
#25208=AXIS2_PLACEMENT_3D('',#35650,#28382,#28383);
#25209=AXIS2_PLACEMENT_3D('',#35651,#28384,#28385);
#25210=AXIS2_PLACEMENT_3D('',#35652,#28386,#28387);
#25211=AXIS2_PLACEMENT_3D('',#35653,#28388,#28389);
#25212=AXIS2_PLACEMENT_3D('',#35654,#28390,#28391);
#25213=AXIS2_PLACEMENT_3D('',#35655,#28392,#28393);
#25214=AXIS2_PLACEMENT_3D('',#35656,#28394,#28395);
#25215=AXIS2_PLACEMENT_3D('',#35657,#28396,#28397);
#25216=AXIS2_PLACEMENT_3D('',#35729,#28399,#28400);
#25217=AXIS2_PLACEMENT_3D('',#35732,#28401,#28402);
#25218=AXIS2_PLACEMENT_3D('',#35735,#28404,#28405);
#25219=AXIS2_PLACEMENT_3D('',#35736,#28406,#28407);
#25220=AXIS2_PLACEMENT_3D('',#35737,#28408,#28409);
#25221=AXIS2_PLACEMENT_3D('',#35739,#28410,#28411);
#25222=AXIS2_PLACEMENT_3D('',#35742,#28413,#28414);
#25223=AXIS2_PLACEMENT_3D('',#35743,#28415,#28416);
#25224=AXIS2_PLACEMENT_3D('',#35745,#28418,#28419);
#25225=AXIS2_PLACEMENT_3D('',#35748,#28420,#28421);
#25226=AXIS2_PLACEMENT_3D('',#35752,#28423,#28424);
#25227=AXIS2_PLACEMENT_3D('',#35754,#28426,#28427);
#25228=AXIS2_PLACEMENT_3D('',#35756,#28428,#28429);
#25229=AXIS2_PLACEMENT_3D('',#35759,#28431,#28432);
#25230=AXIS2_PLACEMENT_3D('',#35760,#28433,#28434);
#25231=AXIS2_PLACEMENT_3D('',#35763,#28435,#28436);
#25232=AXIS2_PLACEMENT_3D('',#35767,#28438,#28439);
#25233=AXIS2_PLACEMENT_3D('',#35769,#28441,#28442);
#25234=AXIS2_PLACEMENT_3D('',#35772,#28443,#28444);
#25235=AXIS2_PLACEMENT_3D('',#35776,#28446,#28447);
#25236=AXIS2_PLACEMENT_3D('',#35778,#28449,#28450);
#25237=AXIS2_PLACEMENT_3D('',#35781,#28451,#28452);
#25238=AXIS2_PLACEMENT_3D('',#35785,#28454,#28455);
#25239=AXIS2_PLACEMENT_3D('',#35787,#28457,#28458);
#25240=AXIS2_PLACEMENT_3D('',#35788,#28459,#28460);
#25241=AXIS2_PLACEMENT_3D('',#35793,#28465,#28466);
#25242=AXIS2_PLACEMENT_3D('',#35798,#28471,#28472);
#25243=AXIS2_PLACEMENT_3D('',#35799,#28473,#28474);
#25244=AXIS2_PLACEMENT_3D('',#35800,#28475,#28476);
#25245=AXIS2_PLACEMENT_3D('',#35801,#28477,#28478);
#25246=AXIS2_PLACEMENT_3D('',#35802,#28479,#28480);
#25247=AXIS2_PLACEMENT_3D('',#35804,#28481,#28482);
#25248=AXIS2_PLACEMENT_3D('',#35807,#28484,#28485);
#25249=AXIS2_PLACEMENT_3D('',#35808,#28486,#28487);
#25250=AXIS2_PLACEMENT_3D('',#35811,#28488,#28489);
#25251=AXIS2_PLACEMENT_3D('',#35814,#28491,#28492);
#25252=AXIS2_PLACEMENT_3D('',#35815,#28493,#28494);
#25253=AXIS2_PLACEMENT_3D('',#35816,#28495,#28496);
#25254=AXIS2_PLACEMENT_3D('',#35818,#28498,#28499);
#25255=AXIS2_PLACEMENT_3D('',#35819,#28500,#28501);
#25256=AXIS2_PLACEMENT_3D('',#35832,#28508,#28509);
#25257=AXIS2_PLACEMENT_3D('',#35838,#28513,#28514);
#25258=AXIS2_PLACEMENT_3D('',#35842,#28517,#28518);
#25259=AXIS2_PLACEMENT_3D('',#35846,#28521,#28522);
#25260=AXIS2_PLACEMENT_3D('',#35850,#28525,#28526);
#25261=AXIS2_PLACEMENT_3D('',#35854,#28529,#28530);
#25262=AXIS2_PLACEMENT_3D('',#35856,#28532,#28533);
#25263=AXIS2_PLACEMENT_3D('',#35857,#28534,#28535);
#25264=AXIS2_PLACEMENT_3D('',#35858,#28536,#28537);
#25265=AXIS2_PLACEMENT_3D('',#35860,#28538,#28539);
#25266=AXIS2_PLACEMENT_3D('',#35863,#28541,#28542);
#25267=AXIS2_PLACEMENT_3D('',#35864,#28543,#28544);
#25268=AXIS2_PLACEMENT_3D('',#35866,#28545,#28546);
#25269=AXIS2_PLACEMENT_3D('',#35869,#28548,#28549);
#25270=AXIS2_PLACEMENT_3D('',#35870,#28550,#28551);
#25271=AXIS2_PLACEMENT_3D('',#35871,#28552,#28553);
#25272=AXIS2_PLACEMENT_3D('',#35872,#28554,#28555);
#25273=AXIS2_PLACEMENT_3D('',#35873,#28556,#28557);
#25274=AXIS2_PLACEMENT_3D('',#35874,#28558,#28559);
#25275=AXIS2_PLACEMENT_3D('',#35875,#28560,#28561);
#25276=AXIS2_PLACEMENT_3D('',#35876,#28562,#28563);
#25277=AXIS2_PLACEMENT_3D('',#35877,#28564,#28565);
#25278=AXIS2_PLACEMENT_3D('',#35878,#28566,#28567);
#25279=AXIS2_PLACEMENT_3D('',#35880,#28568,#28569);
#25280=AXIS2_PLACEMENT_3D('',#35883,#28571,#28572);
#25281=AXIS2_PLACEMENT_3D('',#35884,#28573,#28574);
#25282=AXIS2_PLACEMENT_3D('',#35886,#28575,#28576);
#25283=AXIS2_PLACEMENT_3D('',#35889,#28578,#28579);
#25284=AXIS2_PLACEMENT_3D('',#35890,#28580,#28581);
#25285=AXIS2_PLACEMENT_3D('',#35892,#28582,#28583);
#25286=AXIS2_PLACEMENT_3D('',#35895,#28585,#28586);
#25287=AXIS2_PLACEMENT_3D('',#35896,#28587,#28588);
#25288=AXIS2_PLACEMENT_3D('',#35921,#28601,#28602);
#25289=AXIS2_PLACEMENT_3D('',#35946,#28615,#28616);
#25290=AXIS2_PLACEMENT_3D('',#35949,#28619,#28620);
#25291=AXIS2_PLACEMENT_3D('',#35951,#28622,#28623);
#25292=AXIS2_PLACEMENT_3D('',#35953,#28625,#28626);
#25293=AXIS2_PLACEMENT_3D('',#35955,#28628,#28629);
#25294=AXIS2_PLACEMENT_3D('',#35957,#28631,#28632);
#25295=AXIS2_PLACEMENT_3D('',#35959,#28634,#28635);
#25296=AXIS2_PLACEMENT_3D('',#35961,#28637,#28638);
#25297=AXIS2_PLACEMENT_3D('',#35963,#28640,#28641);
#25298=AXIS2_PLACEMENT_3D('',#35965,#28643,#28644);
#25299=AXIS2_PLACEMENT_3D('',#35967,#28646,#28647);
#25300=AXIS2_PLACEMENT_3D('',#35969,#28649,#28650);
#25301=AXIS2_PLACEMENT_3D('',#35970,#28651,#28652);
#25302=AXIS2_PLACEMENT_3D('',#35972,#28653,#28654);
#25303=AXIS2_PLACEMENT_3D('',#35974,#28655,#28656);
#25304=AXIS2_PLACEMENT_3D('',#35975,#28657,#28658);
#25305=AXIS2_PLACEMENT_3D('',#35976,#28659,#28660);
#25306=AXIS2_PLACEMENT_3D('',#35979,#28662,#28663);
#25307=AXIS2_PLACEMENT_3D('',#35980,#28664,#28665);
#25308=AXIS2_PLACEMENT_3D('',#35982,#28666,#28667);
#25309=AXIS2_PLACEMENT_3D('',#35983,#28668,#28669);
#25310=AXIS2_PLACEMENT_3D('',#35984,#28670,#28671);
#25311=AXIS2_PLACEMENT_3D('',#35986,#28672,#28673);
#25312=AXIS2_PLACEMENT_3D('',#35989,#28675,#28676);
#25313=AXIS2_PLACEMENT_3D('',#35990,#28677,#28678);
#25314=AXIS2_PLACEMENT_3D('',#35992,#28679,#28680);
#25315=AXIS2_PLACEMENT_3D('',#35995,#28682,#28683);
#25316=AXIS2_PLACEMENT_3D('',#35996,#28684,#28685);
#25317=AXIS2_PLACEMENT_3D('',#35998,#28686,#28687);
#25318=AXIS2_PLACEMENT_3D('',#36000,#28688,#28689);
#25319=AXIS2_PLACEMENT_3D('',#36001,#28690,#28691);
#25320=AXIS2_PLACEMENT_3D('',#36002,#28692,#28693);
#25321=AXIS2_PLACEMENT_3D('',#36005,#28695,#28696);
#25322=AXIS2_PLACEMENT_3D('',#36006,#28697,#28698);
#25323=AXIS2_PLACEMENT_3D('',#36008,#28699,#28700);
#25324=AXIS2_PLACEMENT_3D('',#36009,#28701,#28702);
#25325=AXIS2_PLACEMENT_3D('',#36010,#28703,#28704);
#25326=AXIS2_PLACEMENT_3D('',#36012,#28705,#28706);
#25327=AXIS2_PLACEMENT_3D('',#36015,#28708,#28709);
#25328=AXIS2_PLACEMENT_3D('',#36016,#28710,#28711);
#25329=AXIS2_PLACEMENT_3D('',#36018,#28712,#28713);
#25330=AXIS2_PLACEMENT_3D('',#36021,#28715,#28716);
#25331=AXIS2_PLACEMENT_3D('',#36022,#28717,#28718);
#25332=AXIS2_PLACEMENT_3D('',#36023,#28719,#28720);
#25333=AXIS2_PLACEMENT_3D('',#36024,#28721,#28722);
#25334=AXIS2_PLACEMENT_3D('',#36025,#28723,#28724);
#25335=AXIS2_PLACEMENT_3D('',#36026,#28725,#28726);
#25336=AXIS2_PLACEMENT_3D('',#36027,#28727,#28728);
#25337=AXIS2_PLACEMENT_3D('',#36028,#28729,#28730);
#25338=AXIS2_PLACEMENT_3D('',#36029,#28731,#28732);
#25339=AXIS2_PLACEMENT_3D('',#36031,#28733,#28734);
#25340=AXIS2_PLACEMENT_3D('',#36034,#28736,#28737);
#25341=AXIS2_PLACEMENT_3D('',#36035,#28738,#28739);
#25342=AXIS2_PLACEMENT_3D('',#36037,#28740,#28741);
#25343=AXIS2_PLACEMENT_3D('',#36040,#28743,#28744);
#25344=AXIS2_PLACEMENT_3D('',#36041,#28745,#28746);
#25345=AXIS2_PLACEMENT_3D('',#36044,#28747,#28748);
#25346=AXIS2_PLACEMENT_3D('',#36048,#28750,#28751);
#25347=AXIS2_PLACEMENT_3D('',#36050,#28753,#28754);
#25348=AXIS2_PLACEMENT_3D('',#36053,#28755,#28756);
#25349=AXIS2_PLACEMENT_3D('',#36057,#28758,#28759);
#25350=AXIS2_PLACEMENT_3D('',#36059,#28761,#28762);
#25351=AXIS2_PLACEMENT_3D('',#36064,#28764,#28765);
#25352=AXIS2_PLACEMENT_3D('',#36067,#28767,#28768);
#25353=AXIS2_PLACEMENT_3D('',#36069,#28769,#28770);
#25354=AXIS2_PLACEMENT_3D('',#36073,#28772,#28773);
#25355=AXIS2_PLACEMENT_3D('',#36078,#28777,#28778);
#25356=AXIS2_PLACEMENT_3D('',#36088,#28783,#28784);
#25357=AXIS2_PLACEMENT_3D('',#36091,#28786,#28787);
#25358=AXIS2_PLACEMENT_3D('',#36093,#28788,#28789);
#25359=AXIS2_PLACEMENT_3D('',#36096,#28791,#28792);
#25360=AXIS2_PLACEMENT_3D('',#36097,#28793,#28794);
#25361=AXIS2_PLACEMENT_3D('',#36100,#28797,#28798);
#25362=AXIS2_PLACEMENT_3D('',#36102,#28800,#28801);
#25363=AXIS2_PLACEMENT_3D('',#36104,#28803,#28804);
#25364=AXIS2_PLACEMENT_3D('',#36105,#28805,#28806);
#25365=AXIS2_PLACEMENT_3D('',#36107,#28808,#28809);
#25366=AXIS2_PLACEMENT_3D('',#36109,#28811,#28812);
#25367=AXIS2_PLACEMENT_3D('',#36111,#28814,#28815);
#25368=AXIS2_PLACEMENT_3D('',#36113,#28817,#28818);
#25369=AXIS2_PLACEMENT_3D('',#36114,#28819,#28820);
#25370=AXIS2_PLACEMENT_3D('',#36115,#28821,#28822);
#25371=AXIS2_PLACEMENT_3D('',#36116,#28823,#28824);
#25372=AXIS2_PLACEMENT_3D('',#36117,#28825,#28826);
#25373=AXIS2_PLACEMENT_3D('',#36118,#28827,#28828);
#25374=AXIS2_PLACEMENT_3D('',#36120,#28829,#28830);
#25375=AXIS2_PLACEMENT_3D('',#36123,#28832,#28833);
#25376=AXIS2_PLACEMENT_3D('',#36124,#28834,#28835);
#25377=AXIS2_PLACEMENT_3D('',#36126,#28836,#28837);
#25378=AXIS2_PLACEMENT_3D('',#36129,#28839,#28840);
#25379=AXIS2_PLACEMENT_3D('',#36130,#28841,#28842);
#25380=AXIS2_PLACEMENT_3D('',#36132,#28843,#28844);
#25381=AXIS2_PLACEMENT_3D('',#36135,#28846,#28847);
#25382=AXIS2_PLACEMENT_3D('',#36136,#28848,#28849);
#25383=AXIS2_PLACEMENT_3D('',#36138,#28850,#28851);
#25384=AXIS2_PLACEMENT_3D('',#36141,#28853,#28854);
#25385=AXIS2_PLACEMENT_3D('',#36142,#28855,#28856);
#25386=AXIS2_PLACEMENT_3D('',#36151,#28861,#28862);
#25387=AXIS2_PLACEMENT_3D('',#36161,#28868,#28869);
#25388=AXIS2_PLACEMENT_3D('',#36169,#28874,#28875);
#25389=AXIS2_PLACEMENT_3D('',#36179,#28881,#28882);
#25390=AXIS2_PLACEMENT_3D('',#36186,#28887,#28888);
#25391=AXIS2_PLACEMENT_3D('',#36190,#28891,#28892);
#25392=AXIS2_PLACEMENT_3D('',#36191,#28893,#28894);
#25393=AXIS2_PLACEMENT_3D('',#36195,#28897,#28898);
#25394=AXIS2_PLACEMENT_3D('',#36197,#28900,#28901);
#25395=AXIS2_PLACEMENT_3D('',#36201,#28904,#28905);
#25396=AXIS2_PLACEMENT_3D('',#36203,#28907,#28908);
#25397=AXIS2_PLACEMENT_3D('',#36204,#28909,#28910);
#25398=AXIS2_PLACEMENT_3D('',#36205,#28911,#28912);
#25399=AXIS2_PLACEMENT_3D('',#36207,#28913,#28914);
#25400=AXIS2_PLACEMENT_3D('',#36210,#28916,#28917);
#25401=AXIS2_PLACEMENT_3D('',#36211,#28918,#28919);
#25402=AXIS2_PLACEMENT_3D('',#36213,#28920,#28921);
#25403=AXIS2_PLACEMENT_3D('',#36216,#28923,#28924);
#25404=AXIS2_PLACEMENT_3D('',#36217,#28925,#28926);
#25405=AXIS2_PLACEMENT_3D('',#36219,#28927,#28928);
#25406=AXIS2_PLACEMENT_3D('',#36222,#28930,#28931);
#25407=AXIS2_PLACEMENT_3D('',#36223,#28932,#28933);
#25408=AXIS2_PLACEMENT_3D('',#36225,#28934,#28935);
#25409=AXIS2_PLACEMENT_3D('',#36228,#28937,#28938);
#25410=AXIS2_PLACEMENT_3D('',#36229,#28939,#28940);
#25411=AXIS2_PLACEMENT_3D('',#36238,#28945,#28946);
#25412=AXIS2_PLACEMENT_3D('',#36248,#28952,#28953);
#25413=AXIS2_PLACEMENT_3D('',#36256,#28958,#28959);
#25414=AXIS2_PLACEMENT_3D('',#36266,#28965,#28966);
#25415=AXIS2_PLACEMENT_3D('',#36273,#28971,#28972);
#25416=AXIS2_PLACEMENT_3D('',#36277,#28975,#28976);
#25417=AXIS2_PLACEMENT_3D('',#36278,#28977,#28978);
#25418=AXIS2_PLACEMENT_3D('',#36282,#28981,#28982);
#25419=AXIS2_PLACEMENT_3D('',#36284,#28984,#28985);
#25420=AXIS2_PLACEMENT_3D('',#36288,#28988,#28989);
#25421=AXIS2_PLACEMENT_3D('',#36290,#28991,#28992);
#25422=AXIS2_PLACEMENT_3D('',#36291,#28993,#28994);
#25423=AXIS2_PLACEMENT_3D('',#36292,#28995,#28996);
#25424=AXIS2_PLACEMENT_3D('',#36294,#28997,#28998);
#25425=AXIS2_PLACEMENT_3D('',#36297,#29000,#29001);
#25426=AXIS2_PLACEMENT_3D('',#36298,#29002,#29003);
#25427=AXIS2_PLACEMENT_3D('',#36300,#29004,#29005);
#25428=AXIS2_PLACEMENT_3D('',#36303,#29007,#29008);
#25429=AXIS2_PLACEMENT_3D('',#36304,#29009,#29010);
#25430=AXIS2_PLACEMENT_3D('',#36306,#29011,#29012);
#25431=AXIS2_PLACEMENT_3D('',#36309,#29014,#29015);
#25432=AXIS2_PLACEMENT_3D('',#36310,#29016,#29017);
#25433=AXIS2_PLACEMENT_3D('',#36312,#29018,#29019);
#25434=AXIS2_PLACEMENT_3D('',#36315,#29021,#29022);
#25435=AXIS2_PLACEMENT_3D('',#36316,#29023,#29024);
#25436=AXIS2_PLACEMENT_3D('',#36318,#29025,#29026);
#25437=AXIS2_PLACEMENT_3D('',#36321,#29028,#29029);
#25438=AXIS2_PLACEMENT_3D('',#36322,#29030,#29031);
#25439=AXIS2_PLACEMENT_3D('',#36324,#29032,#29033);
#25440=AXIS2_PLACEMENT_3D('',#36327,#29035,#29036);
#25441=AXIS2_PLACEMENT_3D('',#36328,#29037,#29038);
#25442=AXIS2_PLACEMENT_3D('',#36330,#29039,#29040);
#25443=AXIS2_PLACEMENT_3D('',#36333,#29042,#29043);
#25444=AXIS2_PLACEMENT_3D('',#36334,#29044,#29045);
#25445=AXIS2_PLACEMENT_3D('',#36336,#29046,#29047);
#25446=AXIS2_PLACEMENT_3D('',#36339,#29049,#29050);
#25447=AXIS2_PLACEMENT_3D('',#36340,#29051,#29052);
#25448=AXIS2_PLACEMENT_3D('',#36342,#29053,#29054);
#25449=AXIS2_PLACEMENT_3D('',#36345,#29056,#29057);
#25450=AXIS2_PLACEMENT_3D('',#36346,#29058,#29059);
#25451=AXIS2_PLACEMENT_3D('',#36348,#29060,#29061);
#25452=AXIS2_PLACEMENT_3D('',#36351,#29063,#29064);
#25453=AXIS2_PLACEMENT_3D('',#36352,#29065,#29066);
#25454=AXIS2_PLACEMENT_3D('',#36354,#29067,#29068);
#25455=AXIS2_PLACEMENT_3D('',#36357,#29070,#29071);
#25456=AXIS2_PLACEMENT_3D('',#36358,#29072,#29073);
#25457=AXIS2_PLACEMENT_3D('',#36360,#29074,#29075);
#25458=AXIS2_PLACEMENT_3D('',#36363,#29077,#29078);
#25459=AXIS2_PLACEMENT_3D('',#36364,#29079,#29080);
#25460=AXIS2_PLACEMENT_3D('',#36373,#29085,#29086);
#25461=AXIS2_PLACEMENT_3D('',#36379,#29090,#29091);
#25462=AXIS2_PLACEMENT_3D('',#36383,#29094,#29095);
#25463=AXIS2_PLACEMENT_3D('',#36387,#29098,#29099);
#25464=AXIS2_PLACEMENT_3D('',#36389,#29101,#29102);
#25465=AXIS2_PLACEMENT_3D('',#36390,#29103,#29104);
#25466=AXIS2_PLACEMENT_3D('',#36391,#29105,#29106);
#25467=AXIS2_PLACEMENT_3D('',#36392,#29107,#29108);
#25468=AXIS2_PLACEMENT_3D('',#36393,#29109,#29110);
#25469=AXIS2_PLACEMENT_3D('',#36394,#29111,#29112);
#25470=AXIS2_PLACEMENT_3D('',#36395,#29113,#29114);
#25471=AXIS2_PLACEMENT_3D('',#36396,#29115,#29116);
#25472=AXIS2_PLACEMENT_3D('',#36398,#29117,#29118);
#25473=AXIS2_PLACEMENT_3D('',#36399,#29119,#29120);
#25474=AXIS2_PLACEMENT_3D('',#36402,#29122,#29123);
#25475=AXIS2_PLACEMENT_3D('',#36403,#29124,#29125);
#25476=AXIS2_PLACEMENT_3D('',#36405,#29126,#29127);
#25477=AXIS2_PLACEMENT_3D('',#36408,#29129,#29130);
#25478=AXIS2_PLACEMENT_3D('',#36409,#29131,#29132);
#25479=AXIS2_PLACEMENT_3D('',#36411,#29133,#29134);
#25480=AXIS2_PLACEMENT_3D('',#36412,#29135,#29136);
#25481=AXIS2_PLACEMENT_3D('',#36414,#29137,#29138);
#25482=AXIS2_PLACEMENT_3D('',#36416,#29140,#29141);
#25483=AXIS2_PLACEMENT_3D('',#36419,#29142,#29143);
#25484=AXIS2_PLACEMENT_3D('',#36421,#29144,#29145);
#25485=AXIS2_PLACEMENT_3D('',#36422,#29146,#29147);
#25486=AXIS2_PLACEMENT_3D('',#36592,#29148,#29149);
#25487=AXIS2_PLACEMENT_3D('',#36679,#29150,#29151);
#25488=AXIS2_PLACEMENT_3D('',#36906,#29152,#29153);
#25489=AXIS2_PLACEMENT_3D('',#36965,#29154,#29155);
#25490=AXIS2_PLACEMENT_3D('',#36967,#29156,#29157);
#25491=AXIS2_PLACEMENT_3D('',#36968,#29158,#29159);
#25492=AXIS2_PLACEMENT_3D('',#36979,#29160,#29161);
#25493=AXIS2_PLACEMENT_3D('',#36980,#29162,#29163);
#25494=AXIS2_PLACEMENT_3D('',#37204,#29164,#29165);
#25495=AXIS2_PLACEMENT_3D('',#37540,#29166,#29167);
#25496=AXIS2_PLACEMENT_3D('',#37831,#29168,#29169);
#25497=AXIS2_PLACEMENT_3D('',#37854,#29170,#29171);
#25498=AXIS2_PLACEMENT_3D('',#37855,#29172,#29173);
#25499=AXIS2_PLACEMENT_3D('',#37894,#29174,#29175);
#25500=AXIS2_PLACEMENT_3D('',#38069,#29176,#29177);
#25501=AXIS2_PLACEMENT_3D('',#38080,#29178,#29179);
#25502=AXIS2_PLACEMENT_3D('',#38082,#29180,#29181);
#25503=AXIS2_PLACEMENT_3D('',#38083,#29182,#29183);
#25504=AXIS2_PLACEMENT_3D('',#38108,#29184,#29185);
#25505=AXIS2_PLACEMENT_3D('',#38508,#29186,#29187);
#25506=AXIS2_PLACEMENT_3D('',#38630,#29188,#29189);
#25507=AXIS2_PLACEMENT_3D('',#38631,#29190,#29191);
#25508=AXIS2_PLACEMENT_3D('',#38728,#29192,#29193);
#25509=AXIS2_PLACEMENT_3D('',#39211,#29194,#29195);
#25510=AXIS2_PLACEMENT_3D('',#39438,#29196,#29197);
#25511=AXIS2_PLACEMENT_3D('',#39497,#29198,#29199);
#25512=AXIS2_PLACEMENT_3D('',#39499,#29200,#29201);
#25513=AXIS2_PLACEMENT_3D('',#39500,#29202,#29203);
#25514=AXIS2_PLACEMENT_3D('',#39511,#29204,#29205);
#25515=AXIS2_PLACEMENT_3D('',#39512,#29206,#29207);
#25516=AXIS2_PLACEMENT_3D('',#39734,#29208,#29209);
#25517=AXIS2_PLACEMENT_3D('',#40070,#29210,#29211);
#25518=AXIS2_PLACEMENT_3D('',#40370,#29212,#29213);
#25519=AXIS2_PLACEMENT_3D('',#40393,#29214,#29215);
#25520=AXIS2_PLACEMENT_3D('',#40394,#29216,#29217);
#25521=AXIS2_PLACEMENT_3D('',#40433,#29218,#29219);
#25522=AXIS2_PLACEMENT_3D('',#40608,#29220,#29221);
#25523=AXIS2_PLACEMENT_3D('',#40619,#29222,#29223);
#25524=AXIS2_PLACEMENT_3D('',#40621,#29224,#29225);
#25525=AXIS2_PLACEMENT_3D('',#40622,#29226,#29227);
#25526=AXIS2_PLACEMENT_3D('',#40647,#29228,#29229);
#25527=AXIS2_PLACEMENT_3D('',#41047,#29230,#29231);
#25528=AXIS2_PLACEMENT_3D('',#41169,#29232,#29233);
#25529=AXIS2_PLACEMENT_3D('',#41170,#29234,#29235);
#25530=AXIS2_PLACEMENT_3D('',#41267,#29236,#29237);
#25531=AXIS2_PLACEMENT_3D('',#41771,#29238,#29239);
#25532=AXIS2_PLACEMENT_3D('',#41998,#29240,#29241);
#25533=AXIS2_PLACEMENT_3D('',#42057,#29242,#29243);
#25534=AXIS2_PLACEMENT_3D('',#42059,#29244,#29245);
#25535=AXIS2_PLACEMENT_3D('',#42060,#29246,#29247);
#25536=AXIS2_PLACEMENT_3D('',#42071,#29248,#29249);
#25537=AXIS2_PLACEMENT_3D('',#42072,#29250,#29251);
#25538=AXIS2_PLACEMENT_3D('',#42295,#29252,#29253);
#25539=AXIS2_PLACEMENT_3D('',#42635,#29254,#29255);
#25540=AXIS2_PLACEMENT_3D('',#42908,#29256,#29257);
#25541=AXIS2_PLACEMENT_3D('',#42931,#29258,#29259);
#25542=AXIS2_PLACEMENT_3D('',#42932,#29260,#29261);
#25543=AXIS2_PLACEMENT_3D('',#42971,#29262,#29263);
#25544=AXIS2_PLACEMENT_3D('',#43146,#29264,#29265);
#25545=AXIS2_PLACEMENT_3D('',#43157,#29266,#29267);
#25546=AXIS2_PLACEMENT_3D('',#43159,#29268,#29269);
#25547=AXIS2_PLACEMENT_3D('',#43160,#29270,#29271);
#25548=AXIS2_PLACEMENT_3D('',#43185,#29272,#29273);
#25549=AXIS2_PLACEMENT_3D('',#43585,#29274,#29275);
#25550=AXIS2_PLACEMENT_3D('',#43707,#29276,#29277);
#25551=AXIS2_PLACEMENT_3D('',#43708,#29278,#29279);
#25552=AXIS2_PLACEMENT_3D('',#43805,#29280,#29281);
#25553=AXIS2_PLACEMENT_3D('',#44297,#29282,#29283);
#25554=AXIS2_PLACEMENT_3D('',#44527,#29284,#29285);
#25555=AXIS2_PLACEMENT_3D('',#44586,#29286,#29287);
#25556=AXIS2_PLACEMENT_3D('',#44588,#29288,#29289);
#25557=AXIS2_PLACEMENT_3D('',#44589,#29290,#29291);
#25558=AXIS2_PLACEMENT_3D('',#44600,#29292,#29293);
#25559=AXIS2_PLACEMENT_3D('',#44601,#29294,#29295);
#25560=AXIS2_PLACEMENT_3D('',#44825,#29296,#29297);
#25561=AXIS2_PLACEMENT_3D('',#45161,#29298,#29299);
#25562=AXIS2_PLACEMENT_3D('',#45443,#29300,#29301);
#25563=AXIS2_PLACEMENT_3D('',#45466,#29302,#29303);
#25564=AXIS2_PLACEMENT_3D('',#45467,#29304,#29305);
#25565=AXIS2_PLACEMENT_3D('',#45502,#29306,#29307);
#25566=AXIS2_PLACEMENT_3D('',#45680,#29308,#29309);
#25567=AXIS2_PLACEMENT_3D('',#45691,#29310,#29311);
#25568=AXIS2_PLACEMENT_3D('',#45693,#29312,#29313);
#25569=AXIS2_PLACEMENT_3D('',#45694,#29314,#29315);
#25570=AXIS2_PLACEMENT_3D('',#45719,#29316,#29317);
#25571=AXIS2_PLACEMENT_3D('',#46119,#29318,#29319);
#25572=AXIS2_PLACEMENT_3D('',#46241,#29320,#29321);
#25573=AXIS2_PLACEMENT_3D('',#46242,#29322,#29323);
#25574=AXIS2_PLACEMENT_3D('',#46344,#29324,#29325);
#25575=AXIS2_PLACEMENT_3D('',#46780,#29326,#29327);
#25576=AXIS2_PLACEMENT_3D('',#46783,#29328,#29329);
#25577=AXIS2_PLACEMENT_3D('',#46785,#29330,#29331);
#25578=AXIS2_PLACEMENT_3D('',#46786,#29332,#29333);
#25579=AXIS2_PLACEMENT_3D('',#46804,#29334,#29335);
#25580=AXIS2_PLACEMENT_3D('',#46806,#29336,#29337);
#25581=AXIS2_PLACEMENT_3D('',#46817,#29338,#29339);
#25582=AXIS2_PLACEMENT_3D('',#46819,#29340,#29341);
#25583=AXIS2_PLACEMENT_3D('',#46820,#29342,#29343);
#25584=AXIS2_PLACEMENT_3D('',#47069,#29344,#29345);
#25585=AXIS2_PLACEMENT_3D('',#47160,#29346,#29347);
#25586=AXIS2_PLACEMENT_3D('',#47686,#29348,#29349);
#25587=AXIS2_PLACEMENT_3D('',#47687,#29350,#29351);
#25588=AXIS2_PLACEMENT_3D('',#47689,#29352,#29353);
#25589=AXIS2_PLACEMENT_3D('',#47690,#29354,#29355);
#25590=AXIS2_PLACEMENT_3D('',#47937,#29356,#29357);
#25591=AXIS2_PLACEMENT_3D('',#48167,#29358,#29359);
#25592=AXIS2_PLACEMENT_3D('',#48226,#29360,#29361);
#25593=AXIS2_PLACEMENT_3D('',#48228,#29362,#29363);
#25594=AXIS2_PLACEMENT_3D('',#48229,#29364,#29365);
#25595=AXIS2_PLACEMENT_3D('',#48240,#29366,#29367);
#25596=AXIS2_PLACEMENT_3D('',#48241,#29368,#29369);
#25597=AXIS2_PLACEMENT_3D('',#48463,#29370,#29371);
#25598=AXIS2_PLACEMENT_3D('',#48811,#29372,#29373);
#25599=AXIS2_PLACEMENT_3D('',#49111,#29374,#29375);
#25600=AXIS2_PLACEMENT_3D('',#49134,#29376,#29377);
#25601=AXIS2_PLACEMENT_3D('',#49135,#29378,#29379);
#25602=AXIS2_PLACEMENT_3D('',#49174,#29380,#29381);
#25603=AXIS2_PLACEMENT_3D('',#49349,#29382,#29383);
#25604=AXIS2_PLACEMENT_3D('',#49360,#29384,#29385);
#25605=AXIS2_PLACEMENT_3D('',#49362,#29386,#29387);
#25606=AXIS2_PLACEMENT_3D('',#49363,#29388,#29389);
#25607=AXIS2_PLACEMENT_3D('',#49388,#29390,#29391);
#25608=AXIS2_PLACEMENT_3D('',#49788,#29392,#29393);
#25609=AXIS2_PLACEMENT_3D('',#49910,#29394,#29395);
#25610=AXIS2_PLACEMENT_3D('',#49911,#29396,#29397);
#25611=AXIS2_PLACEMENT_3D('',#50005,#29398,#29399);
#25612=AXIS2_PLACEMENT_3D('',#50501,#29400,#29401);
#25613=AXIS2_PLACEMENT_3D('',#50502,#29402,#29403);
#25614=AXIS2_PLACEMENT_3D('',#50606,#29404,#29405);
#25615=AXIS2_PLACEMENT_3D('',#50607,#29406,#29407);
#25616=AXIS2_PLACEMENT_3D('',#50617,#29408,#29409);
#25617=AXIS2_PLACEMENT_3D('',#50618,#29410,#29411);
#25618=AXIS2_PLACEMENT_3D('',#50628,#29412,#29413);
#25619=AXIS2_PLACEMENT_3D('',#50629,#29414,#29415);
#25620=AXIS2_PLACEMENT_3D('',#50639,#29416,#29417);
#25621=AXIS2_PLACEMENT_3D('',#50640,#29418,#29419);
#25622=AXIS2_PLACEMENT_3D('',#50650,#29420,#29421);
#25623=AXIS2_PLACEMENT_3D('',#50651,#29422,#29423);
#25624=AXIS2_PLACEMENT_3D('',#50652,#29424,#29425);
#25625=AXIS2_PLACEMENT_3D('',#50654,#29426,#29427);
#25626=AXIS2_PLACEMENT_3D('',#50655,#29428,#29429);
#25627=AXIS2_PLACEMENT_3D('',#50657,#29430,#29431);
#25628=AXIS2_PLACEMENT_3D('',#50659,#29433,#29434);
#25629=AXIS2_PLACEMENT_3D('',#50661,#29435,#29436);
#25630=AXIS2_PLACEMENT_3D('',#50662,#29437,#29438);
#25631=AXIS2_PLACEMENT_3D('',#50664,#29439,#29440);
#25632=AXIS2_PLACEMENT_3D('',#50666,#29442,#29443);
#25633=AXIS2_PLACEMENT_3D('',#50704,#29444,#29445);
#25634=AXIS2_PLACEMENT_3D('',#51386,#29446,#29447);
#25635=AXIS2_PLACEMENT_3D('',#51644,#29448,#29449);
#25636=AXIS2_PLACEMENT_3D('',#51646,#29450,#29451);
#25637=AXIS2_PLACEMENT_3D('',#51647,#29452,#29453);
#25638=AXIS2_PLACEMENT_3D('',#51650,#29455,#29456);
#25639=AXIS2_PLACEMENT_3D('',#51651,#29457,#29458);
#25640=AXIS2_PLACEMENT_3D('',#51653,#29459,#29460);
#25641=AXIS2_PLACEMENT_3D('',#51654,#29461,#29462);
#25642=AXIS2_PLACEMENT_3D('',#51657,#29464,#29465);
#25643=AXIS2_PLACEMENT_3D('',#51658,#29466,#29467);
#25644=AXIS2_PLACEMENT_3D('',#51659,#29468,#29469);
#25645=AXIS2_PLACEMENT_3D('',#51660,#29470,#29471);
#25646=AXIS2_PLACEMENT_3D('',#51662,#29472,#29473);
#25647=AXIS2_PLACEMENT_3D('',#51675,#29480,#29481);
#25648=AXIS2_PLACEMENT_3D('',#51677,#29482,#29483);
#25649=AXIS2_PLACEMENT_3D('',#51678,#29484,#29485);
#25650=AXIS2_PLACEMENT_3D('',#51680,#29487,#29488);
#25651=AXIS2_PLACEMENT_3D('',#51693,#29495,#29496);
#25652=AXIS2_PLACEMENT_3D('',#51696,#29499,#29500);
#25653=AXIS2_PLACEMENT_3D('',#51698,#29502,#29503);
#25654=AXIS2_PLACEMENT_3D('',#51700,#29505,#29506);
#25655=AXIS2_PLACEMENT_3D('',#51702,#29508,#29509);
#25656=AXIS2_PLACEMENT_3D('',#51704,#29511,#29512);
#25657=AXIS2_PLACEMENT_3D('',#51705,#29513,#29514);
#25658=AXIS2_PLACEMENT_3D('',#51706,#29515,#29516);
#25659=AXIS2_PLACEMENT_3D('',#51709,#29517,#29518);
#25660=AXIS2_PLACEMENT_3D('',#51711,#29519,#29520);
#25661=AXIS2_PLACEMENT_3D('',#51713,#29521,#29522);
#25662=AXIS2_PLACEMENT_3D('',#51714,#29523,#29524);
#25663=AXIS2_PLACEMENT_3D('',#51715,#29525,#29526);
#25664=AXIS2_PLACEMENT_3D('',#51717,#29527,#29528);
#25665=AXIS2_PLACEMENT_3D('',#51722,#29530,#29531);
#25666=AXIS2_PLACEMENT_3D('',#51726,#29534,#29535);
#25667=AXIS2_PLACEMENT_3D('',#51728,#29536,#29537);
#25668=AXIS2_PLACEMENT_3D('',#51730,#29539,#29540);
#25669=AXIS2_PLACEMENT_3D('',#51755,#29543,#29544);
#25670=AXIS2_PLACEMENT_3D('',#51756,#29545,#29546);
#25671=AXIS2_PLACEMENT_3D('',#51759,#29547,#29548);
#25672=AXIS2_PLACEMENT_3D('',#51761,#29549,#29550);
#25673=AXIS2_PLACEMENT_3D('',#51763,#29551,#29552);
#25674=AXIS2_PLACEMENT_3D('',#51764,#29553,#29554);
#25675=AXIS2_PLACEMENT_3D('',#51765,#29555,#29556);
#25676=AXIS2_PLACEMENT_3D('',#51768,#29557,#29558);
#25677=AXIS2_PLACEMENT_3D('',#51770,#29559,#29560);
#25678=AXIS2_PLACEMENT_3D('',#51772,#29561,#29562);
#25679=AXIS2_PLACEMENT_3D('',#51773,#29563,#29564);
#25680=AXIS2_PLACEMENT_3D('',#51774,#29565,#29566);
#25681=AXIS2_PLACEMENT_3D('',#51777,#29567,#29568);
#25682=AXIS2_PLACEMENT_3D('',#51780,#29571,#29572);
#25683=AXIS2_PLACEMENT_3D('',#51784,#29574,#29575);
#25684=AXIS2_PLACEMENT_3D('',#51786,#29577,#29578);
#25685=AXIS2_PLACEMENT_3D('',#51790,#29580,#29581);
#25686=AXIS2_PLACEMENT_3D('',#51792,#29583,#29584);
#25687=AXIS2_PLACEMENT_3D('',#51795,#29586,#29587);
#25688=AXIS2_PLACEMENT_3D('',#51796,#29588,#29589);
#25689=AXIS2_PLACEMENT_3D('',#51799,#29591,#29592);
#25690=AXIS2_PLACEMENT_3D('',#51800,#29593,#29594);
#25691=AXIS2_PLACEMENT_3D('',#51802,#29595,#29596);
#25692=AXIS2_PLACEMENT_3D('',#51804,#29598,#29599);
#25693=AXIS2_PLACEMENT_3D('',#51806,#29600,#29601);
#25694=AXIS2_PLACEMENT_3D('',#51808,#29602,#29603);
#25695=AXIS2_PLACEMENT_3D('',#51810,#29604,#29605);
#25696=AXIS2_PLACEMENT_3D('',#51812,#29606,#29607);
#25697=AXIS2_PLACEMENT_3D('',#51813,#29608,#29609);
#25698=AXIS2_PLACEMENT_3D('',#51814,#29610,#29611);
#25699=AXIS2_PLACEMENT_3D('',#51815,#29612,#29613);
#25700=AXIS2_PLACEMENT_3D('',#51823,#29617,#29618);
#25701=AXIS2_PLACEMENT_3D('',#51824,#29619,#29620);
#25702=AXIS2_PLACEMENT_3D('',#51826,#29622,#29623);
#25703=AXIS2_PLACEMENT_3D('',#51828,#29625,#29626);
#25704=AXIS2_PLACEMENT_3D('',#51830,#29628,#29629);
#25705=AXIS2_PLACEMENT_3D('',#51833,#29632,#29633);
#25706=AXIS2_PLACEMENT_3D('',#51837,#29636,#29637);
#25707=AXIS2_PLACEMENT_3D('',#51838,#29638,#29639);
#25708=AXIS2_PLACEMENT_3D('',#51839,#29640,#29641);
#25709=AXIS2_PLACEMENT_3D('',#51840,#29642,#29643);
#25710=AXIS2_PLACEMENT_3D('',#51883,#29645,#29646);
#25711=AXIS2_PLACEMENT_3D('',#51905,#29649,#29650);
#25712=AXIS2_PLACEMENT_3D('',#51909,#29652,#29653);
#25713=AXIS2_PLACEMENT_3D('',#51913,#29655,#29656);
#25714=AXIS2_PLACEMENT_3D('',#51917,#29658,#29659);
#25715=AXIS2_PLACEMENT_3D('',#51921,#29661,#29662);
#25716=AXIS2_PLACEMENT_3D('',#51925,#29664,#29665);
#25717=AXIS2_PLACEMENT_3D('',#51929,#29667,#29668);
#25718=AXIS2_PLACEMENT_3D('',#51933,#29670,#29671);
#25719=AXIS2_PLACEMENT_3D('',#51939,#29674,#29675);
#25720=AXIS2_PLACEMENT_3D('',#51941,#29676,#29677);
#25721=AXIS2_PLACEMENT_3D('',#51945,#29679,#29680);
#25722=AXIS2_PLACEMENT_3D('',#51946,#29681,#29682);
#25723=AXIS2_PLACEMENT_3D('',#51949,#29683,#29684);
#25724=AXIS2_PLACEMENT_3D('',#51953,#29686,#29687);
#25725=AXIS2_PLACEMENT_3D('',#51955,#29688,#29689);
#25726=AXIS2_PLACEMENT_3D('',#51959,#29691,#29692);
#25727=AXIS2_PLACEMENT_3D('',#51963,#29694,#29695);
#25728=AXIS2_PLACEMENT_3D('',#51965,#29696,#29697);
#25729=AXIS2_PLACEMENT_3D('',#51968,#29699,#29700);
#25730=AXIS2_PLACEMENT_3D('',#51971,#29701,#29702);
#25731=AXIS2_PLACEMENT_3D('',#51975,#29704,#29705);
#25732=AXIS2_PLACEMENT_3D('',#51977,#29706,#29707);
#25733=AXIS2_PLACEMENT_3D('',#51980,#29709,#29710);
#25734=AXIS2_PLACEMENT_3D('',#51981,#29711,#29712);
#25735=AXIS2_PLACEMENT_3D('',#51984,#29713,#29714);
#25736=AXIS2_PLACEMENT_3D('',#51988,#29716,#29717);
#25737=AXIS2_PLACEMENT_3D('',#51992,#29719,#29720);
#25738=AXIS2_PLACEMENT_3D('',#51996,#29722,#29723);
#25739=AXIS2_PLACEMENT_3D('',#51998,#29725,#29726);
#25740=AXIS2_PLACEMENT_3D('',#52001,#29729,#29730);
#25741=AXIS2_PLACEMENT_3D('',#52003,#29732,#29733);
#25742=AXIS2_PLACEMENT_3D('',#52005,#29735,#29736);
#25743=AXIS2_PLACEMENT_3D('',#52007,#29738,#29739);
#25744=AXIS2_PLACEMENT_3D('',#52009,#29741,#29742);
#25745=AXIS2_PLACEMENT_3D('',#52011,#29744,#29745);
#25746=AXIS2_PLACEMENT_3D('',#52013,#29747,#29748);
#25747=AXIS2_PLACEMENT_3D('',#52014,#29749,#29750);
#25748=AXIS2_PLACEMENT_3D('',#52018,#29752,#29753);
#25749=AXIS2_PLACEMENT_3D('',#52020,#29755,#29756);
#25750=AXIS2_PLACEMENT_3D('',#52024,#29759,#29760);
#25751=AXIS2_PLACEMENT_3D('',#52027,#29762,#29763);
#25752=AXIS2_PLACEMENT_3D('',#52028,#29764,#29765);
#25753=AXIS2_PLACEMENT_3D('',#52034,#29769,#29770);
#25754=AXIS2_PLACEMENT_3D('',#52037,#29772,#29773);
#25755=AXIS2_PLACEMENT_3D('',#52038,#29774,#29775);
#25756=AXIS2_PLACEMENT_3D('',#52041,#29777,#29778);
#25757=AXIS2_PLACEMENT_3D('',#52042,#29779,#29780);
#25758=AXIS2_PLACEMENT_3D('',#52046,#29783,#29784);
#25759=AXIS2_PLACEMENT_3D('',#52049,#29786,#29787);
#25760=AXIS2_PLACEMENT_3D('',#52050,#29788,#29789);
#25761=AXIS2_PLACEMENT_3D('',#52054,#29792,#29793);
#25762=AXIS2_PLACEMENT_3D('',#52055,#29794,#29795);
#25763=AXIS2_PLACEMENT_3D('',#52056,#29796,#29797);
#25764=AXIS2_PLACEMENT_3D('',#52057,#29798,#29799);
#25765=AXIS2_PLACEMENT_3D('',#52058,#29800,#29801);
#25766=AXIS2_PLACEMENT_3D('',#52059,#29802,#29803);
#25767=AXIS2_PLACEMENT_3D('',#52062,#29804,#29805);
#25768=AXIS2_PLACEMENT_3D('',#52066,#29807,#29808);
#25769=AXIS2_PLACEMENT_3D('',#52068,#29809,#29810);
#25770=AXIS2_PLACEMENT_3D('',#52071,#29812,#29813);
#25771=AXIS2_PLACEMENT_3D('',#52072,#29814,#29815);
#25772=AXIS2_PLACEMENT_3D('',#52075,#29818,#29819);
#25773=AXIS2_PLACEMENT_3D('',#52077,#29821,#29822);
#25774=AXIS2_PLACEMENT_3D('',#52079,#29824,#29825);
#25775=AXIS2_PLACEMENT_3D('',#52081,#29827,#29828);
#25776=AXIS2_PLACEMENT_3D('',#52083,#29830,#29831);
#25777=AXIS2_PLACEMENT_3D('',#52084,#29832,#29833);
#25778=AXIS2_PLACEMENT_3D('',#52090,#29837,#29838);
#25779=AXIS2_PLACEMENT_3D('',#52093,#29840,#29841);
#25780=AXIS2_PLACEMENT_3D('',#52094,#29842,#29843);
#25781=AXIS2_PLACEMENT_3D('',#52097,#29845,#29846);
#25782=AXIS2_PLACEMENT_3D('',#52098,#29847,#29848);
#25783=AXIS2_PLACEMENT_3D('',#52102,#29851,#29852);
#25784=AXIS2_PLACEMENT_3D('',#52104,#29853,#29854);
#25785=AXIS2_PLACEMENT_3D('',#52106,#29856,#29857);
#25786=AXIS2_PLACEMENT_3D('',#52107,#29858,#29859);
#25787=AXIS2_PLACEMENT_3D('',#52108,#29860,#29861);
#25788=AXIS2_PLACEMENT_3D('',#52109,#29862,#29863);
#25789=AXIS2_PLACEMENT_3D('',#52113,#29865,#29866);
#25790=AXIS2_PLACEMENT_3D('',#52115,#29868,#29869);
#25791=AXIS2_PLACEMENT_3D('',#52119,#29872,#29873);
#25792=AXIS2_PLACEMENT_3D('',#52122,#29875,#29876);
#25793=AXIS2_PLACEMENT_3D('',#52123,#29877,#29878);
#25794=AXIS2_PLACEMENT_3D('',#52142,#29880,#29881);
#25795=AXIS2_PLACEMENT_3D('',#52146,#29884,#29885);
#25796=AXIS2_PLACEMENT_3D('',#52150,#29887,#29888);
#25797=AXIS2_PLACEMENT_3D('',#52152,#29890,#29891);
#25798=AXIS2_PLACEMENT_3D('',#52156,#29894,#29895);
#25799=AXIS2_PLACEMENT_3D('',#52159,#29897,#29898);
#25800=AXIS2_PLACEMENT_3D('',#52160,#29899,#29900);
#25801=AXIS2_PLACEMENT_3D('',#52164,#29903,#29904);
#25802=AXIS2_PLACEMENT_3D('',#52167,#29906,#29907);
#25803=AXIS2_PLACEMENT_3D('',#52168,#29908,#29909);
#25804=AXIS2_PLACEMENT_3D('',#52170,#29911,#29912);
#25805=AXIS2_PLACEMENT_3D('',#52191,#29914,#29915);
#25806=AXIS2_PLACEMENT_3D('',#52193,#29917,#29918);
#25807=AXIS2_PLACEMENT_3D('',#52194,#29919,#29920);
#25808=AXIS2_PLACEMENT_3D('',#52195,#29921,#29922);
#25809=AXIS2_PLACEMENT_3D('',#52197,#29923,#29924);
#25810=AXIS2_PLACEMENT_3D('',#52210,#29931,#29932);
#25811=AXIS2_PLACEMENT_3D('',#52212,#29933,#29934);
#25812=AXIS2_PLACEMENT_3D('',#52213,#29935,#29936);
#25813=AXIS2_PLACEMENT_3D('',#52215,#29938,#29939);
#25814=AXIS2_PLACEMENT_3D('',#52228,#29946,#29947);
#25815=AXIS2_PLACEMENT_3D('',#52231,#29950,#29951);
#25816=AXIS2_PLACEMENT_3D('',#52233,#29953,#29954);
#25817=AXIS2_PLACEMENT_3D('',#52235,#29956,#29957);
#25818=AXIS2_PLACEMENT_3D('',#52237,#29959,#29960);
#25819=AXIS2_PLACEMENT_3D('',#52239,#29962,#29963);
#25820=AXIS2_PLACEMENT_3D('',#52240,#29964,#29965);
#25821=AXIS2_PLACEMENT_3D('',#52241,#29966,#29967);
#25822=AXIS2_PLACEMENT_3D('',#52244,#29968,#29969);
#25823=AXIS2_PLACEMENT_3D('',#52246,#29970,#29971);
#25824=AXIS2_PLACEMENT_3D('',#52248,#29972,#29973);
#25825=AXIS2_PLACEMENT_3D('',#52249,#29974,#29975);
#25826=AXIS2_PLACEMENT_3D('',#52250,#29976,#29977);
#25827=AXIS2_PLACEMENT_3D('',#52252,#29978,#29979);
#25828=AXIS2_PLACEMENT_3D('',#52260,#29983,#29984);
#25829=AXIS2_PLACEMENT_3D('',#52261,#29985,#29986);
#25830=AXIS2_PLACEMENT_3D('',#52263,#29987,#29988);
#25831=AXIS2_PLACEMENT_3D('',#52265,#29990,#29991);
#25832=AXIS2_PLACEMENT_3D('',#52290,#29994,#29995);
#25833=AXIS2_PLACEMENT_3D('',#52291,#29996,#29997);
#25834=AXIS2_PLACEMENT_3D('',#52294,#29998,#29999);
#25835=AXIS2_PLACEMENT_3D('',#52296,#30000,#30001);
#25836=AXIS2_PLACEMENT_3D('',#52298,#30002,#30003);
#25837=AXIS2_PLACEMENT_3D('',#52299,#30004,#30005);
#25838=AXIS2_PLACEMENT_3D('',#52300,#30006,#30007);
#25839=AXIS2_PLACEMENT_3D('',#52303,#30008,#30009);
#25840=AXIS2_PLACEMENT_3D('',#52305,#30010,#30011);
#25841=AXIS2_PLACEMENT_3D('',#52307,#30012,#30013);
#25842=AXIS2_PLACEMENT_3D('',#52308,#30014,#30015);
#25843=AXIS2_PLACEMENT_3D('',#52309,#30016,#30017);
#25844=AXIS2_PLACEMENT_3D('',#52312,#30018,#30019);
#25845=AXIS2_PLACEMENT_3D('',#52315,#30022,#30023);
#25846=AXIS2_PLACEMENT_3D('',#52319,#30025,#30026);
#25847=AXIS2_PLACEMENT_3D('',#52321,#30028,#30029);
#25848=AXIS2_PLACEMENT_3D('',#52325,#30031,#30032);
#25849=AXIS2_PLACEMENT_3D('',#52327,#30034,#30035);
#25850=AXIS2_PLACEMENT_3D('',#52330,#30037,#30038);
#25851=AXIS2_PLACEMENT_3D('',#52331,#30039,#30040);
#25852=AXIS2_PLACEMENT_3D('',#52334,#30042,#30043);
#25853=AXIS2_PLACEMENT_3D('',#52335,#30044,#30045);
#25854=AXIS2_PLACEMENT_3D('',#52337,#30046,#30047);
#25855=AXIS2_PLACEMENT_3D('',#52339,#30049,#30050);
#25856=AXIS2_PLACEMENT_3D('',#52341,#30051,#30052);
#25857=AXIS2_PLACEMENT_3D('',#52343,#30053,#30054);
#25858=AXIS2_PLACEMENT_3D('',#52345,#30055,#30056);
#25859=AXIS2_PLACEMENT_3D('',#52347,#30057,#30058);
#25860=AXIS2_PLACEMENT_3D('',#52348,#30059,#30060);
#25861=AXIS2_PLACEMENT_3D('',#52349,#30061,#30062);
#25862=AXIS2_PLACEMENT_3D('',#52350,#30063,#30064);
#25863=AXIS2_PLACEMENT_3D('',#52355,#30066,#30067);
#25864=AXIS2_PLACEMENT_3D('',#52359,#30070,#30071);
#25865=AXIS2_PLACEMENT_3D('',#52361,#30073,#30074);
#25866=AXIS2_PLACEMENT_3D('',#52363,#30076,#30077);
#25867=AXIS2_PLACEMENT_3D('',#52365,#30079,#30080);
#25868=AXIS2_PLACEMENT_3D('',#52395,#30085,#30086);
#25869=AXIS2_PLACEMENT_3D('',#52399,#30089,#30090);
#25870=AXIS2_PLACEMENT_3D('',#52403,#30093,#30094);
#25871=AXIS2_PLACEMENT_3D('',#52405,#30095,#30096);
#25872=AXIS2_PLACEMENT_3D('',#52407,#30098,#30099);
#25873=AXIS2_PLACEMENT_3D('',#52409,#30100,#30101);
#25874=AXIS2_PLACEMENT_3D('',#52412,#30103,#30104);
#25875=AXIS2_PLACEMENT_3D('',#52413,#30105,#30106);
#25876=AXIS2_PLACEMENT_3D('',#52415,#30108,#30109);
#25877=AXIS2_PLACEMENT_3D('',#52417,#30111,#30112);
#25878=AXIS2_PLACEMENT_3D('',#52460,#30114,#30115);
#25879=AXIS2_PLACEMENT_3D('',#52482,#30118,#30119);
#25880=AXIS2_PLACEMENT_3D('',#52486,#30121,#30122);
#25881=AXIS2_PLACEMENT_3D('',#52490,#30124,#30125);
#25882=AXIS2_PLACEMENT_3D('',#52494,#30127,#30128);
#25883=AXIS2_PLACEMENT_3D('',#52498,#30130,#30131);
#25884=AXIS2_PLACEMENT_3D('',#52502,#30133,#30134);
#25885=AXIS2_PLACEMENT_3D('',#52506,#30136,#30137);
#25886=AXIS2_PLACEMENT_3D('',#52510,#30139,#30140);
#25887=AXIS2_PLACEMENT_3D('',#52516,#30143,#30144);
#25888=AXIS2_PLACEMENT_3D('',#52518,#30145,#30146);
#25889=AXIS2_PLACEMENT_3D('',#52522,#30148,#30149);
#25890=AXIS2_PLACEMENT_3D('',#52523,#30150,#30151);
#25891=AXIS2_PLACEMENT_3D('',#52526,#30152,#30153);
#25892=AXIS2_PLACEMENT_3D('',#52530,#30155,#30156);
#25893=AXIS2_PLACEMENT_3D('',#52532,#30157,#30158);
#25894=AXIS2_PLACEMENT_3D('',#52536,#30160,#30161);
#25895=AXIS2_PLACEMENT_3D('',#52540,#30163,#30164);
#25896=AXIS2_PLACEMENT_3D('',#52542,#30165,#30166);
#25897=AXIS2_PLACEMENT_3D('',#52545,#30168,#30169);
#25898=AXIS2_PLACEMENT_3D('',#52548,#30170,#30171);
#25899=AXIS2_PLACEMENT_3D('',#52552,#30173,#30174);
#25900=AXIS2_PLACEMENT_3D('',#52554,#30175,#30176);
#25901=AXIS2_PLACEMENT_3D('',#52557,#30178,#30179);
#25902=AXIS2_PLACEMENT_3D('',#52558,#30180,#30181);
#25903=AXIS2_PLACEMENT_3D('',#52561,#30182,#30183);
#25904=AXIS2_PLACEMENT_3D('',#52565,#30185,#30186);
#25905=AXIS2_PLACEMENT_3D('',#52569,#30188,#30189);
#25906=AXIS2_PLACEMENT_3D('',#52573,#30191,#30192);
#25907=AXIS2_PLACEMENT_3D('',#52575,#30194,#30195);
#25908=AXIS2_PLACEMENT_3D('',#52578,#30198,#30199);
#25909=AXIS2_PLACEMENT_3D('',#52580,#30201,#30202);
#25910=AXIS2_PLACEMENT_3D('',#52582,#30204,#30205);
#25911=AXIS2_PLACEMENT_3D('',#52584,#30207,#30208);
#25912=AXIS2_PLACEMENT_3D('',#52586,#30210,#30211);
#25913=AXIS2_PLACEMENT_3D('',#52588,#30213,#30214);
#25914=AXIS2_PLACEMENT_3D('',#52590,#30216,#30217);
#25915=AXIS2_PLACEMENT_3D('',#52591,#30218,#30219);
#25916=AXIS2_PLACEMENT_3D('',#52595,#30221,#30222);
#25917=AXIS2_PLACEMENT_3D('',#52597,#30224,#30225);
#25918=AXIS2_PLACEMENT_3D('',#52601,#30228,#30229);
#25919=AXIS2_PLACEMENT_3D('',#52604,#30231,#30232);
#25920=AXIS2_PLACEMENT_3D('',#52605,#30233,#30234);
#25921=AXIS2_PLACEMENT_3D('',#52611,#30238,#30239);
#25922=AXIS2_PLACEMENT_3D('',#52614,#30241,#30242);
#25923=AXIS2_PLACEMENT_3D('',#52615,#30243,#30244);
#25924=AXIS2_PLACEMENT_3D('',#52618,#30246,#30247);
#25925=AXIS2_PLACEMENT_3D('',#52619,#30248,#30249);
#25926=AXIS2_PLACEMENT_3D('',#52623,#30252,#30253);
#25927=AXIS2_PLACEMENT_3D('',#52626,#30255,#30256);
#25928=AXIS2_PLACEMENT_3D('',#52627,#30257,#30258);
#25929=AXIS2_PLACEMENT_3D('',#52631,#30261,#30262);
#25930=AXIS2_PLACEMENT_3D('',#52632,#30263,#30264);
#25931=AXIS2_PLACEMENT_3D('',#52633,#30265,#30266);
#25932=AXIS2_PLACEMENT_3D('',#52634,#30267,#30268);
#25933=AXIS2_PLACEMENT_3D('',#52635,#30269,#30270);
#25934=AXIS2_PLACEMENT_3D('',#52636,#30271,#30272);
#25935=AXIS2_PLACEMENT_3D('',#52639,#30273,#30274);
#25936=AXIS2_PLACEMENT_3D('',#52643,#30276,#30277);
#25937=AXIS2_PLACEMENT_3D('',#52645,#30278,#30279);
#25938=AXIS2_PLACEMENT_3D('',#52648,#30281,#30282);
#25939=AXIS2_PLACEMENT_3D('',#52649,#30283,#30284);
#25940=AXIS2_PLACEMENT_3D('',#52652,#30287,#30288);
#25941=AXIS2_PLACEMENT_3D('',#52654,#30290,#30291);
#25942=AXIS2_PLACEMENT_3D('',#52656,#30293,#30294);
#25943=AXIS2_PLACEMENT_3D('',#52658,#30296,#30297);
#25944=AXIS2_PLACEMENT_3D('',#52660,#30299,#30300);
#25945=AXIS2_PLACEMENT_3D('',#52661,#30301,#30302);
#25946=AXIS2_PLACEMENT_3D('',#52667,#30306,#30307);
#25947=AXIS2_PLACEMENT_3D('',#52670,#30309,#30310);
#25948=AXIS2_PLACEMENT_3D('',#52671,#30311,#30312);
#25949=AXIS2_PLACEMENT_3D('',#52674,#30314,#30315);
#25950=AXIS2_PLACEMENT_3D('',#52675,#30316,#30317);
#25951=AXIS2_PLACEMENT_3D('',#52679,#30320,#30321);
#25952=AXIS2_PLACEMENT_3D('',#52681,#30322,#30323);
#25953=AXIS2_PLACEMENT_3D('',#52683,#30325,#30326);
#25954=AXIS2_PLACEMENT_3D('',#52684,#30327,#30328);
#25955=AXIS2_PLACEMENT_3D('',#52685,#30329,#30330);
#25956=AXIS2_PLACEMENT_3D('',#52686,#30331,#30332);
#25957=AXIS2_PLACEMENT_3D('',#52690,#30334,#30335);
#25958=AXIS2_PLACEMENT_3D('',#52692,#30337,#30338);
#25959=AXIS2_PLACEMENT_3D('',#52696,#30341,#30342);
#25960=AXIS2_PLACEMENT_3D('',#52699,#30344,#30345);
#25961=AXIS2_PLACEMENT_3D('',#52700,#30346,#30347);
#25962=AXIS2_PLACEMENT_3D('',#52719,#30349,#30350);
#25963=AXIS2_PLACEMENT_3D('',#52723,#30353,#30354);
#25964=AXIS2_PLACEMENT_3D('',#52727,#30356,#30357);
#25965=AXIS2_PLACEMENT_3D('',#52729,#30359,#30360);
#25966=AXIS2_PLACEMENT_3D('',#52733,#30363,#30364);
#25967=AXIS2_PLACEMENT_3D('',#52736,#30366,#30367);
#25968=AXIS2_PLACEMENT_3D('',#52737,#30368,#30369);
#25969=AXIS2_PLACEMENT_3D('',#52741,#30372,#30373);
#25970=AXIS2_PLACEMENT_3D('',#52744,#30375,#30376);
#25971=AXIS2_PLACEMENT_3D('',#52745,#30377,#30378);
#25972=AXIS2_PLACEMENT_3D('',#52747,#30380,#30381);
#25973=AXIS2_PLACEMENT_3D('',#52768,#30383,#30384);
#25974=AXIS2_PLACEMENT_3D('',#52770,#30386,#30387);
#25975=AXIS2_PLACEMENT_3D('',#52771,#30388,#30389);
#25976=AXIS2_PLACEMENT_3D('',#52772,#30390,#30391);
#25977=AXIS2_PLACEMENT_3D('',#52773,#30392,#30393);
#25978=AXIS2_PLACEMENT_3D('',#52774,#30394,#30395);
#25979=AXIS2_PLACEMENT_3D('',#52775,#30396,#30397);
#25980=AXIS2_PLACEMENT_3D('',#52776,#30398,#30399);
#25981=AXIS2_PLACEMENT_3D('',#52777,#30400,#30401);
#25982=AXIS2_PLACEMENT_3D('',#52778,#30402,#30403);
#25983=AXIS2_PLACEMENT_3D('',#52779,#30404,#30405);
#25984=AXIS2_PLACEMENT_3D('',#52781,#30406,#30407);
#25985=AXIS2_PLACEMENT_3D('',#52784,#30409,#30410);
#25986=AXIS2_PLACEMENT_3D('',#52785,#30411,#30412);
#25987=AXIS2_PLACEMENT_3D('',#52787,#30413,#30414);
#25988=AXIS2_PLACEMENT_3D('',#52790,#30416,#30417);
#25989=AXIS2_PLACEMENT_3D('',#52791,#30418,#30419);
#25990=AXIS2_PLACEMENT_3D('',#52793,#30420,#30421);
#25991=AXIS2_PLACEMENT_3D('',#52796,#30423,#30424);
#25992=AXIS2_PLACEMENT_3D('',#52797,#30425,#30426);
#25993=AXIS2_PLACEMENT_3D('',#52799,#30427,#30428);
#25994=AXIS2_PLACEMENT_3D('',#52802,#30430,#30431);
#25995=AXIS2_PLACEMENT_3D('',#52803,#30432,#30433);
#25996=AXIS2_PLACEMENT_3D('',#52805,#30434,#30435);
#25997=AXIS2_PLACEMENT_3D('',#52808,#30437,#30438);
#25998=AXIS2_PLACEMENT_3D('',#52809,#30439,#30440);
#25999=AXIS2_PLACEMENT_3D('',#52811,#30441,#30442);
#26000=AXIS2_PLACEMENT_3D('',#52814,#30444,#30445);
#26001=AXIS2_PLACEMENT_3D('',#52815,#30446,#30447);
#26002=AXIS2_PLACEMENT_3D('',#52817,#30448,#30449);
#26003=AXIS2_PLACEMENT_3D('',#52820,#30451,#30452);
#26004=AXIS2_PLACEMENT_3D('',#52821,#30453,#30454);
#26005=AXIS2_PLACEMENT_3D('',#52826,#30456,#30457);
#26006=AXIS2_PLACEMENT_3D('',#52833,#30461,#30462);
#26007=AXIS2_PLACEMENT_3D('',#52834,#30463,#30464);
#26008=AXIS2_PLACEMENT_3D('',#52840,#30468,#30469);
#26009=AXIS2_PLACEMENT_3D('',#52844,#30471,#30472);
#26010=AXIS2_PLACEMENT_3D('',#52846,#30473,#30474);
#26011=AXIS2_PLACEMENT_3D('',#52850,#30477,#30478);
#26012=AXIS2_PLACEMENT_3D('',#52853,#30481,#30482);
#26013=AXIS2_PLACEMENT_3D('',#52855,#30484,#30485);
#26014=AXIS2_PLACEMENT_3D('',#52857,#30487,#30488);
#26015=AXIS2_PLACEMENT_3D('',#52858,#30489,#30490);
#26016=AXIS2_PLACEMENT_3D('',#52859,#30491,#30492);
#26017=AXIS2_PLACEMENT_3D('',#52860,#30493,#30494);
#26018=AXIS2_PLACEMENT_3D('',#52862,#30495,#30496);
#26019=AXIS2_PLACEMENT_3D('',#52865,#30498,#30499);
#26020=AXIS2_PLACEMENT_3D('',#52866,#30500,#30501);
#26021=AXIS2_PLACEMENT_3D('',#52868,#30502,#30503);
#26022=AXIS2_PLACEMENT_3D('',#52871,#30505,#30506);
#26023=AXIS2_PLACEMENT_3D('',#52872,#30507,#30508);
#26024=AXIS2_PLACEMENT_3D('',#52874,#30509,#30510);
#26025=AXIS2_PLACEMENT_3D('',#52877,#30512,#30513);
#26026=AXIS2_PLACEMENT_3D('',#52878,#30514,#30515);
#26027=AXIS2_PLACEMENT_3D('',#52880,#30516,#30517);
#26028=AXIS2_PLACEMENT_3D('',#52883,#30519,#30520);
#26029=AXIS2_PLACEMENT_3D('',#52884,#30521,#30522);
#26030=AXIS2_PLACEMENT_3D('',#52886,#30523,#30524);
#26031=AXIS2_PLACEMENT_3D('',#52889,#30526,#30527);
#26032=AXIS2_PLACEMENT_3D('',#52890,#30528,#30529);
#26033=AXIS2_PLACEMENT_3D('',#52892,#30530,#30531);
#26034=AXIS2_PLACEMENT_3D('',#52895,#30533,#30534);
#26035=AXIS2_PLACEMENT_3D('',#52896,#30535,#30536);
#26036=AXIS2_PLACEMENT_3D('',#52905,#30541,#30542);
#26037=AXIS2_PLACEMENT_3D('',#52911,#30546,#30547);
#26038=AXIS2_PLACEMENT_3D('',#52917,#30551,#30552);
#26039=AXIS2_PLACEMENT_3D('',#52920,#30555,#30556);
#26040=AXIS2_PLACEMENT_3D('',#52921,#30557,#30558);
#26041=AXIS2_PLACEMENT_3D('',#52922,#30559,#30560);
#26042=AXIS2_PLACEMENT_3D('',#52923,#30561,#30562);
#26043=AXIS2_PLACEMENT_3D('',#52924,#30563,#30564);
#26044=AXIS2_PLACEMENT_3D('',#52925,#30565,#30566);
#26045=AXIS2_PLACEMENT_3D('',#52927,#30567,#30568);
#26046=AXIS2_PLACEMENT_3D('',#52930,#30570,#30571);
#26047=AXIS2_PLACEMENT_3D('',#52931,#30572,#30573);
#26048=AXIS2_PLACEMENT_3D('',#52933,#30574,#30575);
#26049=AXIS2_PLACEMENT_3D('',#52936,#30577,#30578);
#26050=AXIS2_PLACEMENT_3D('',#52937,#30579,#30580);
#26051=AXIS2_PLACEMENT_3D('',#52939,#30581,#30582);
#26052=AXIS2_PLACEMENT_3D('',#52942,#30584,#30585);
#26053=AXIS2_PLACEMENT_3D('',#52943,#30586,#30587);
#26054=AXIS2_PLACEMENT_3D('',#52945,#30588,#30589);
#26055=AXIS2_PLACEMENT_3D('',#52948,#30591,#30592);
#26056=AXIS2_PLACEMENT_3D('',#52949,#30593,#30594);
#26057=AXIS2_PLACEMENT_3D('',#52951,#30595,#30596);
#26058=AXIS2_PLACEMENT_3D('',#52954,#30598,#30599);
#26059=AXIS2_PLACEMENT_3D('',#52955,#30600,#30601);
#26060=AXIS2_PLACEMENT_3D('',#52957,#30602,#30603);
#26061=AXIS2_PLACEMENT_3D('',#52960,#30605,#30606);
#26062=AXIS2_PLACEMENT_3D('',#52961,#30607,#30608);
#26063=AXIS2_PLACEMENT_3D('',#52970,#30613,#30614);
#26064=AXIS2_PLACEMENT_3D('',#52976,#30618,#30619);
#26065=AXIS2_PLACEMENT_3D('',#52982,#30623,#30624);
#26066=AXIS2_PLACEMENT_3D('',#52985,#30627,#30628);
#26067=AXIS2_PLACEMENT_3D('',#52986,#30629,#30630);
#26068=AXIS2_PLACEMENT_3D('',#52987,#30631,#30632);
#26069=AXIS2_PLACEMENT_3D('',#52988,#30633,#30634);
#26070=AXIS2_PLACEMENT_3D('',#52997,#30639,#30640);
#26071=AXIS2_PLACEMENT_3D('',#53003,#30644,#30645);
#26072=AXIS2_PLACEMENT_3D('',#53009,#30649,#30650);
#26073=AXIS2_PLACEMENT_3D('',#53015,#30654,#30655);
#26074=AXIS2_PLACEMENT_3D('',#53018,#30658,#30659);
#26075=AXIS2_PLACEMENT_3D('',#53019,#30660,#30661);
#26076=AXIS2_PLACEMENT_3D('',#53020,#30662,#30663);
#26077=AXIS2_PLACEMENT_3D('',#53029,#30668,#30669);
#26078=AXIS2_PLACEMENT_3D('',#53035,#30673,#30674);
#26079=AXIS2_PLACEMENT_3D('',#53041,#30678,#30679);
#26080=AXIS2_PLACEMENT_3D('',#53047,#30683,#30684);
#26081=AXIS2_PLACEMENT_3D('',#53050,#30687,#30688);
#26082=AXIS2_PLACEMENT_3D('',#53051,#30689,#30690);
#26083=AXIS2_PLACEMENT_3D('',#53052,#30691,#30692);
#26084=AXIS2_PLACEMENT_3D('',#53055,#30693,#30694);
#26085=AXIS2_PLACEMENT_3D('',#53059,#30696,#30697);
#26086=AXIS2_PLACEMENT_3D('',#53061,#30699,#30700);
#26087=AXIS2_PLACEMENT_3D('',#53063,#30701,#30702);
#26088=AXIS2_PLACEMENT_3D('',#53066,#30704,#30705);
#26089=AXIS2_PLACEMENT_3D('',#53067,#30706,#30707);
#26090=AXIS2_PLACEMENT_3D('',#53069,#30708,#30709);
#26091=AXIS2_PLACEMENT_3D('',#53072,#30711,#30712);
#26092=AXIS2_PLACEMENT_3D('',#53073,#30713,#30714);
#26093=AXIS2_PLACEMENT_3D('',#53075,#30715,#30716);
#26094=AXIS2_PLACEMENT_3D('',#53078,#30718,#30719);
#26095=AXIS2_PLACEMENT_3D('',#53079,#30720,#30721);
#26096=AXIS2_PLACEMENT_3D('',#53081,#30722,#30723);
#26097=AXIS2_PLACEMENT_3D('',#53084,#30725,#30726);
#26098=AXIS2_PLACEMENT_3D('',#53085,#30727,#30728);
#26099=AXIS2_PLACEMENT_3D('',#53087,#30729,#30730);
#26100=AXIS2_PLACEMENT_3D('',#53090,#30732,#30733);
#26101=AXIS2_PLACEMENT_3D('',#53091,#30734,#30735);
#26102=AXIS2_PLACEMENT_3D('',#53093,#30736,#30737);
#26103=AXIS2_PLACEMENT_3D('',#53096,#30739,#30740);
#26104=AXIS2_PLACEMENT_3D('',#53097,#30741,#30742);
#26105=AXIS2_PLACEMENT_3D('',#53099,#30743,#30744);
#26106=AXIS2_PLACEMENT_3D('',#53102,#30746,#30747);
#26107=AXIS2_PLACEMENT_3D('',#53103,#30748,#30749);
#26108=AXIS2_PLACEMENT_3D('',#53105,#30750,#30751);
#26109=AXIS2_PLACEMENT_3D('',#53108,#30753,#30754);
#26110=AXIS2_PLACEMENT_3D('',#53109,#30755,#30756);
#26111=AXIS2_PLACEMENT_3D('',#53111,#30757,#30758);
#26112=AXIS2_PLACEMENT_3D('',#53114,#30760,#30761);
#26113=AXIS2_PLACEMENT_3D('',#53115,#30762,#30763);
#26114=AXIS2_PLACEMENT_3D('',#53117,#30764,#30765);
#26115=AXIS2_PLACEMENT_3D('',#53120,#30767,#30768);
#26116=AXIS2_PLACEMENT_3D('',#53121,#30769,#30770);
#26117=AXIS2_PLACEMENT_3D('',#53123,#30771,#30772);
#26118=AXIS2_PLACEMENT_3D('',#53126,#30774,#30775);
#26119=AXIS2_PLACEMENT_3D('',#53127,#30776,#30777);
#26120=AXIS2_PLACEMENT_3D('',#53129,#30778,#30779);
#26121=AXIS2_PLACEMENT_3D('',#53132,#30781,#30782);
#26122=AXIS2_PLACEMENT_3D('',#53133,#30783,#30784);
#26123=AXIS2_PLACEMENT_3D('',#53135,#30785,#30786);
#26124=AXIS2_PLACEMENT_3D('',#53138,#30788,#30789);
#26125=AXIS2_PLACEMENT_3D('',#53139,#30790,#30791);
#26126=AXIS2_PLACEMENT_3D('',#53141,#30792,#30793);
#26127=AXIS2_PLACEMENT_3D('',#53144,#30795,#30796);
#26128=AXIS2_PLACEMENT_3D('',#53145,#30797,#30798);
#26129=AXIS2_PLACEMENT_3D('',#53147,#30799,#30800);
#26130=AXIS2_PLACEMENT_3D('',#53150,#30802,#30803);
#26131=AXIS2_PLACEMENT_3D('',#53151,#30804,#30805);
#26132=AXIS2_PLACEMENT_3D('',#53153,#30806,#30807);
#26133=AXIS2_PLACEMENT_3D('',#53156,#30809,#30810);
#26134=AXIS2_PLACEMENT_3D('',#53157,#30811,#30812);
#26135=AXIS2_PLACEMENT_3D('',#53159,#30813,#30814);
#26136=AXIS2_PLACEMENT_3D('',#53162,#30816,#30817);
#26137=AXIS2_PLACEMENT_3D('',#53163,#30818,#30819);
#26138=AXIS2_PLACEMENT_3D('',#53165,#30820,#30821);
#26139=AXIS2_PLACEMENT_3D('',#53168,#30823,#30824);
#26140=AXIS2_PLACEMENT_3D('',#53169,#30825,#30826);
#26141=AXIS2_PLACEMENT_3D('',#53171,#30827,#30828);
#26142=AXIS2_PLACEMENT_3D('',#53174,#30830,#30831);
#26143=AXIS2_PLACEMENT_3D('',#53175,#30832,#30833);
#26144=AXIS2_PLACEMENT_3D('',#53177,#30834,#30835);
#26145=AXIS2_PLACEMENT_3D('',#53180,#30837,#30838);
#26146=AXIS2_PLACEMENT_3D('',#53181,#30839,#30840);
#26147=AXIS2_PLACEMENT_3D('',#53183,#30841,#30842);
#26148=AXIS2_PLACEMENT_3D('',#53186,#30844,#30845);
#26149=AXIS2_PLACEMENT_3D('',#53187,#30846,#30847);
#26150=AXIS2_PLACEMENT_3D('',#53189,#30848,#30849);
#26151=AXIS2_PLACEMENT_3D('',#53192,#30851,#30852);
#26152=AXIS2_PLACEMENT_3D('',#53193,#30853,#30854);
#26153=AXIS2_PLACEMENT_3D('',#53195,#30855,#30856);
#26154=AXIS2_PLACEMENT_3D('',#53198,#30858,#30859);
#26155=AXIS2_PLACEMENT_3D('',#53199,#30860,#30861);
#26156=AXIS2_PLACEMENT_3D('',#53201,#30862,#30863);
#26157=AXIS2_PLACEMENT_3D('',#53204,#30865,#30866);
#26158=AXIS2_PLACEMENT_3D('',#53205,#30867,#30868);
#26159=AXIS2_PLACEMENT_3D('',#53207,#30869,#30870);
#26160=AXIS2_PLACEMENT_3D('',#53210,#30872,#30873);
#26161=AXIS2_PLACEMENT_3D('',#53211,#30874,#30875);
#26162=AXIS2_PLACEMENT_3D('',#53213,#30876,#30877);
#26163=AXIS2_PLACEMENT_3D('',#53216,#30879,#30880);
#26164=AXIS2_PLACEMENT_3D('',#53217,#30881,#30882);
#26165=AXIS2_PLACEMENT_3D('',#53219,#30883,#30884);
#26166=AXIS2_PLACEMENT_3D('',#53222,#30886,#30887);
#26167=AXIS2_PLACEMENT_3D('',#53223,#30888,#30889);
#26168=AXIS2_PLACEMENT_3D('',#53225,#30890,#30891);
#26169=AXIS2_PLACEMENT_3D('',#53228,#30893,#30894);
#26170=AXIS2_PLACEMENT_3D('',#53229,#30895,#30896);
#26171=AXIS2_PLACEMENT_3D('',#53231,#30897,#30898);
#26172=AXIS2_PLACEMENT_3D('',#53234,#30900,#30901);
#26173=AXIS2_PLACEMENT_3D('',#53235,#30902,#30903);
#26174=AXIS2_PLACEMENT_3D('',#53237,#30904,#30905);
#26175=AXIS2_PLACEMENT_3D('',#53240,#30907,#30908);
#26176=AXIS2_PLACEMENT_3D('',#53241,#30909,#30910);
#26177=AXIS2_PLACEMENT_3D('',#53243,#30911,#30912);
#26178=AXIS2_PLACEMENT_3D('',#53246,#30914,#30915);
#26179=AXIS2_PLACEMENT_3D('',#53247,#30916,#30917);
#26180=AXIS2_PLACEMENT_3D('',#53249,#30918,#30919);
#26181=AXIS2_PLACEMENT_3D('',#53252,#30921,#30922);
#26182=AXIS2_PLACEMENT_3D('',#53253,#30923,#30924);
#26183=AXIS2_PLACEMENT_3D('',#53255,#30925,#30926);
#26184=AXIS2_PLACEMENT_3D('',#53258,#30928,#30929);
#26185=AXIS2_PLACEMENT_3D('',#53259,#30930,#30931);
#26186=AXIS2_PLACEMENT_3D('',#53261,#30932,#30933);
#26187=AXIS2_PLACEMENT_3D('',#53264,#30935,#30936);
#26188=AXIS2_PLACEMENT_3D('',#53265,#30937,#30938);
#26189=AXIS2_PLACEMENT_3D('',#53267,#30939,#30940);
#26190=AXIS2_PLACEMENT_3D('',#53270,#30942,#30943);
#26191=AXIS2_PLACEMENT_3D('',#53271,#30944,#30945);
#26192=AXIS2_PLACEMENT_3D('',#53273,#30946,#30947);
#26193=AXIS2_PLACEMENT_3D('',#53276,#30949,#30950);
#26194=AXIS2_PLACEMENT_3D('',#53277,#30951,#30952);
#26195=AXIS2_PLACEMENT_3D('',#53279,#30953,#30954);
#26196=AXIS2_PLACEMENT_3D('',#53282,#30956,#30957);
#26197=AXIS2_PLACEMENT_3D('',#53283,#30958,#30959);
#26198=AXIS2_PLACEMENT_3D('',#53285,#30960,#30961);
#26199=AXIS2_PLACEMENT_3D('',#53288,#30963,#30964);
#26200=AXIS2_PLACEMENT_3D('',#53289,#30965,#30966);
#26201=AXIS2_PLACEMENT_3D('',#53291,#30967,#30968);
#26202=AXIS2_PLACEMENT_3D('',#53294,#30970,#30971);
#26203=AXIS2_PLACEMENT_3D('',#53295,#30972,#30973);
#26204=AXIS2_PLACEMENT_3D('',#53297,#30974,#30975);
#26205=AXIS2_PLACEMENT_3D('',#53300,#30977,#30978);
#26206=AXIS2_PLACEMENT_3D('',#53301,#30979,#30980);
#26207=AXIS2_PLACEMENT_3D('',#53303,#30981,#30982);
#26208=AXIS2_PLACEMENT_3D('',#53306,#30984,#30985);
#26209=AXIS2_PLACEMENT_3D('',#53307,#30986,#30987);
#26210=AXIS2_PLACEMENT_3D('',#53309,#30988,#30989);
#26211=AXIS2_PLACEMENT_3D('',#53312,#30991,#30992);
#26212=AXIS2_PLACEMENT_3D('',#53313,#30993,#30994);
#26213=AXIS2_PLACEMENT_3D('',#53315,#30995,#30996);
#26214=AXIS2_PLACEMENT_3D('',#53318,#30998,#30999);
#26215=AXIS2_PLACEMENT_3D('',#53319,#31000,#31001);
#26216=AXIS2_PLACEMENT_3D('',#53321,#31002,#31003);
#26217=AXIS2_PLACEMENT_3D('',#53324,#31005,#31006);
#26218=AXIS2_PLACEMENT_3D('',#53325,#31007,#31008);
#26219=AXIS2_PLACEMENT_3D('',#53327,#31009,#31010);
#26220=AXIS2_PLACEMENT_3D('',#53330,#31012,#31013);
#26221=AXIS2_PLACEMENT_3D('',#53331,#31014,#31015);
#26222=AXIS2_PLACEMENT_3D('',#53333,#31016,#31017);
#26223=AXIS2_PLACEMENT_3D('',#53336,#31019,#31020);
#26224=AXIS2_PLACEMENT_3D('',#53337,#31021,#31022);
#26225=AXIS2_PLACEMENT_3D('',#53339,#31023,#31024);
#26226=AXIS2_PLACEMENT_3D('',#53342,#31026,#31027);
#26227=AXIS2_PLACEMENT_3D('',#53343,#31028,#31029);
#26228=AXIS2_PLACEMENT_3D('',#53345,#31030,#31031);
#26229=AXIS2_PLACEMENT_3D('',#53348,#31033,#31034);
#26230=AXIS2_PLACEMENT_3D('',#53349,#31035,#31036);
#26231=AXIS2_PLACEMENT_3D('',#53366,#31045,#31046);
#26232=AXIS2_PLACEMENT_3D('',#53375,#31051,#31052);
#26233=AXIS2_PLACEMENT_3D('',#53384,#31057,#31058);
#26234=AXIS2_PLACEMENT_3D('',#53393,#31063,#31064);
#26235=AXIS2_PLACEMENT_3D('',#53401,#31070,#31071);
#26236=AXIS2_PLACEMENT_3D('',#53402,#31072,#31073);
#26237=AXIS2_PLACEMENT_3D('',#53409,#31078,#31079);
#26238=AXIS2_PLACEMENT_3D('',#53411,#31081,#31082);
#26239=AXIS2_PLACEMENT_3D('',#53428,#31091,#31092);
#26240=AXIS2_PLACEMENT_3D('',#53431,#31095,#31096);
#26241=AXIS2_PLACEMENT_3D('',#53434,#31099,#31100);
#26242=AXIS2_PLACEMENT_3D('',#53437,#31103,#31104);
#26243=AXIS2_PLACEMENT_3D('',#53440,#31107,#31108);
#26244=AXIS2_PLACEMENT_3D('',#53441,#31109,#31110);
#26245=AXIS2_PLACEMENT_3D('',#53442,#31111,#31112);
#26246=AXIS2_PLACEMENT_3D('',#53443,#31113,#31114);
#26247=AXIS2_PLACEMENT_3D('',#53444,#31115,#31116);
#26248=AXIS2_PLACEMENT_3D('',#53445,#31117,#31118);
#26249=AXIS2_PLACEMENT_3D('',#53446,#31119,#31120);
#26250=AXIS2_PLACEMENT_3D('',#53447,#31121,#31122);
#26251=AXIS2_PLACEMENT_3D('',#53448,#31123,#31124);
#26252=AXIS2_PLACEMENT_3D('',#53449,#31125,#31126);
#26253=AXIS2_PLACEMENT_3D('',#53450,#31127,#31128);
#26254=AXIS2_PLACEMENT_3D('',#53451,#31129,#31130);
#26255=AXIS2_PLACEMENT_3D('',#53452,#31131,#31132);
#26256=AXIS2_PLACEMENT_3D('',#53453,#31133,#31134);
#26257=AXIS2_PLACEMENT_3D('',#53454,#31135,#31136);
#26258=AXIS2_PLACEMENT_3D('',#53455,#31137,#31138);
#26259=AXIS2_PLACEMENT_3D('',#53456,#31139,#31140);
#26260=AXIS2_PLACEMENT_3D('',#53457,#31141,#31142);
#26261=AXIS2_PLACEMENT_3D('',#53458,#31143,#31144);
#26262=AXIS2_PLACEMENT_3D('',#53459,#31145,#31146);
#26263=AXIS2_PLACEMENT_3D('',#53461,#31148,#31149);
#26264=AXIS2_PLACEMENT_3D('',#53463,#31151,#31152);
#26265=AXIS2_PLACEMENT_3D('',#53464,#31153,#31154);
#26266=AXIS2_PLACEMENT_3D('',#53465,#31155,#31156);
#26267=AXIS2_PLACEMENT_3D('',#53466,#31157,#31158);
#26268=AXIS2_PLACEMENT_3D('',#53467,#31159,#31160);
#26269=AXIS2_PLACEMENT_3D('',#53468,#31161,#31162);
#26270=AXIS2_PLACEMENT_3D('',#53469,#31163,#31164);
#26271=AXIS2_PLACEMENT_3D('',#53470,#31165,#31166);
#26272=AXIS2_PLACEMENT_3D('',#53472,#31167,#31168);
#26273=AXIS2_PLACEMENT_3D('',#53475,#31170,#31171);
#26274=AXIS2_PLACEMENT_3D('',#53476,#31172,#31173);
#26275=AXIS2_PLACEMENT_3D('',#53479,#31174,#31175);
#26276=AXIS2_PLACEMENT_3D('',#53481,#31176,#31177);
#26277=AXIS2_PLACEMENT_3D('',#53483,#31178,#31179);
#26278=AXIS2_PLACEMENT_3D('',#53485,#31180,#31181);
#26279=AXIS2_PLACEMENT_3D('',#53487,#31182,#31183);
#26280=AXIS2_PLACEMENT_3D('',#53490,#31185,#31186);
#26281=AXIS2_PLACEMENT_3D('',#53492,#31187,#31188);
#26282=AXIS2_PLACEMENT_3D('',#53494,#31189,#31190);
#26283=AXIS2_PLACEMENT_3D('',#53496,#31191,#31192);
#26284=AXIS2_PLACEMENT_3D('',#53497,#31193,#31194);
#26285=AXIS2_PLACEMENT_3D('',#53498,#31195,#31196);
#26286=AXIS2_PLACEMENT_3D('',#53500,#31197,#31198);
#26287=AXIS2_PLACEMENT_3D('',#53503,#31200,#31201);
#26288=AXIS2_PLACEMENT_3D('',#53504,#31202,#31203);
#26289=AXIS2_PLACEMENT_3D('',#53507,#31204,#31205);
#26290=AXIS2_PLACEMENT_3D('',#53509,#31206,#31207);
#26291=AXIS2_PLACEMENT_3D('',#53511,#31208,#31209);
#26292=AXIS2_PLACEMENT_3D('',#53513,#31210,#31211);
#26293=AXIS2_PLACEMENT_3D('',#53515,#31212,#31213);
#26294=AXIS2_PLACEMENT_3D('',#53518,#31215,#31216);
#26295=AXIS2_PLACEMENT_3D('',#53520,#31217,#31218);
#26296=AXIS2_PLACEMENT_3D('',#53522,#31219,#31220);
#26297=AXIS2_PLACEMENT_3D('',#53524,#31221,#31222);
#26298=AXIS2_PLACEMENT_3D('',#53525,#31223,#31224);
#26299=AXIS2_PLACEMENT_3D('',#53526,#31225,#31226);
#26300=AXIS2_PLACEMENT_3D('',#53528,#31227,#31228);
#26301=AXIS2_PLACEMENT_3D('',#53531,#31230,#31231);
#26302=AXIS2_PLACEMENT_3D('',#53532,#31232,#31233);
#26303=AXIS2_PLACEMENT_3D('',#53535,#31234,#31235);
#26304=AXIS2_PLACEMENT_3D('',#53537,#31236,#31237);
#26305=AXIS2_PLACEMENT_3D('',#53539,#31238,#31239);
#26306=AXIS2_PLACEMENT_3D('',#53541,#31240,#31241);
#26307=AXIS2_PLACEMENT_3D('',#53543,#31242,#31243);
#26308=AXIS2_PLACEMENT_3D('',#53546,#31245,#31246);
#26309=AXIS2_PLACEMENT_3D('',#53548,#31247,#31248);
#26310=AXIS2_PLACEMENT_3D('',#53550,#31249,#31250);
#26311=AXIS2_PLACEMENT_3D('',#53552,#31251,#31252);
#26312=AXIS2_PLACEMENT_3D('',#53553,#31253,#31254);
#26313=AXIS2_PLACEMENT_3D('',#53554,#31255,#31256);
#26314=AXIS2_PLACEMENT_3D('',#53556,#31257,#31258);
#26315=AXIS2_PLACEMENT_3D('',#53559,#31260,#31261);
#26316=AXIS2_PLACEMENT_3D('',#53560,#31262,#31263);
#26317=AXIS2_PLACEMENT_3D('',#53563,#31264,#31265);
#26318=AXIS2_PLACEMENT_3D('',#53565,#31266,#31267);
#26319=AXIS2_PLACEMENT_3D('',#53567,#31268,#31269);
#26320=AXIS2_PLACEMENT_3D('',#53569,#31270,#31271);
#26321=AXIS2_PLACEMENT_3D('',#53571,#31272,#31273);
#26322=AXIS2_PLACEMENT_3D('',#53574,#31275,#31276);
#26323=AXIS2_PLACEMENT_3D('',#53576,#31277,#31278);
#26324=AXIS2_PLACEMENT_3D('',#53578,#31279,#31280);
#26325=AXIS2_PLACEMENT_3D('',#53580,#31281,#31282);
#26326=AXIS2_PLACEMENT_3D('',#53581,#31283,#31284);
#26327=AXIS2_PLACEMENT_3D('',#53582,#31285,#31286);
#26328=AXIS2_PLACEMENT_3D('',#53584,#31287,#31288);
#26329=AXIS2_PLACEMENT_3D('',#53587,#31290,#31291);
#26330=AXIS2_PLACEMENT_3D('',#53588,#31292,#31293);
#26331=AXIS2_PLACEMENT_3D('',#53591,#31294,#31295);
#26332=AXIS2_PLACEMENT_3D('',#53593,#31296,#31297);
#26333=AXIS2_PLACEMENT_3D('',#53595,#31298,#31299);
#26334=AXIS2_PLACEMENT_3D('',#53597,#31300,#31301);
#26335=AXIS2_PLACEMENT_3D('',#53599,#31302,#31303);
#26336=AXIS2_PLACEMENT_3D('',#53602,#31305,#31306);
#26337=AXIS2_PLACEMENT_3D('',#53604,#31307,#31308);
#26338=AXIS2_PLACEMENT_3D('',#53606,#31309,#31310);
#26339=AXIS2_PLACEMENT_3D('',#53608,#31311,#31312);
#26340=AXIS2_PLACEMENT_3D('',#53609,#31313,#31314);
#26341=AXIS2_PLACEMENT_3D('',#53610,#31315,#31316);
#26342=AXIS2_PLACEMENT_3D('',#53612,#31317,#31318);
#26343=AXIS2_PLACEMENT_3D('',#53615,#31320,#31321);
#26344=AXIS2_PLACEMENT_3D('',#53616,#31322,#31323);
#26345=AXIS2_PLACEMENT_3D('',#53619,#31324,#31325);
#26346=AXIS2_PLACEMENT_3D('',#53621,#31326,#31327);
#26347=AXIS2_PLACEMENT_3D('',#53623,#31328,#31329);
#26348=AXIS2_PLACEMENT_3D('',#53625,#31330,#31331);
#26349=AXIS2_PLACEMENT_3D('',#53627,#31332,#31333);
#26350=AXIS2_PLACEMENT_3D('',#53630,#31335,#31336);
#26351=AXIS2_PLACEMENT_3D('',#53632,#31337,#31338);
#26352=AXIS2_PLACEMENT_3D('',#53634,#31339,#31340);
#26353=AXIS2_PLACEMENT_3D('',#53636,#31341,#31342);
#26354=AXIS2_PLACEMENT_3D('',#53637,#31343,#31344);
#26355=AXIS2_PLACEMENT_3D('',#53638,#31345,#31346);
#26356=AXIS2_PLACEMENT_3D('',#53640,#31347,#31348);
#26357=AXIS2_PLACEMENT_3D('',#53643,#31350,#31351);
#26358=AXIS2_PLACEMENT_3D('',#53644,#31352,#31353);
#26359=AXIS2_PLACEMENT_3D('',#53647,#31354,#31355);
#26360=AXIS2_PLACEMENT_3D('',#53649,#31356,#31357);
#26361=AXIS2_PLACEMENT_3D('',#53651,#31358,#31359);
#26362=AXIS2_PLACEMENT_3D('',#53653,#31360,#31361);
#26363=AXIS2_PLACEMENT_3D('',#53655,#31362,#31363);
#26364=AXIS2_PLACEMENT_3D('',#53658,#31365,#31366);
#26365=AXIS2_PLACEMENT_3D('',#53660,#31367,#31368);
#26366=AXIS2_PLACEMENT_3D('',#53662,#31369,#31370);
#26367=AXIS2_PLACEMENT_3D('',#53664,#31371,#31372);
#26368=AXIS2_PLACEMENT_3D('',#53665,#31373,#31374);
#26369=AXIS2_PLACEMENT_3D('',#53666,#31375,#31376);
#26370=AXIS2_PLACEMENT_3D('',#53668,#31377,#31378);
#26371=AXIS2_PLACEMENT_3D('',#53671,#31380,#31381);
#26372=AXIS2_PLACEMENT_3D('',#53672,#31382,#31383);
#26373=AXIS2_PLACEMENT_3D('',#53675,#31384,#31385);
#26374=AXIS2_PLACEMENT_3D('',#53677,#31386,#31387);
#26375=AXIS2_PLACEMENT_3D('',#53679,#31388,#31389);
#26376=AXIS2_PLACEMENT_3D('',#53681,#31390,#31391);
#26377=AXIS2_PLACEMENT_3D('',#53683,#31392,#31393);
#26378=AXIS2_PLACEMENT_3D('',#53686,#31395,#31396);
#26379=AXIS2_PLACEMENT_3D('',#53688,#31397,#31398);
#26380=AXIS2_PLACEMENT_3D('',#53690,#31399,#31400);
#26381=AXIS2_PLACEMENT_3D('',#53692,#31401,#31402);
#26382=AXIS2_PLACEMENT_3D('',#53693,#31403,#31404);
#26383=AXIS2_PLACEMENT_3D('',#53694,#31405,#31406);
#26384=AXIS2_PLACEMENT_3D('',#53700,#31410,#31411);
#26385=AXIS2_PLACEMENT_3D('',#53703,#31414,#31415);
#26386=AXIS2_PLACEMENT_3D('',#53705,#31417,#31418);
#26387=AXIS2_PLACEMENT_3D('',#53720,#31430,#31431);
#26388=AXIS2_PLACEMENT_3D('',#53736,#31443,#31444);
#26389=AXIS2_PLACEMENT_3D('',#53737,#31445,#31446);
#26390=AXIS2_PLACEMENT_3D('',#53740,#31449,#31450);
#26391=AXIS2_PLACEMENT_3D('',#53741,#31451,#31452);
#26392=AXIS2_PLACEMENT_3D('',#53742,#31453,#31454);
#26393=AXIS2_PLACEMENT_3D('',#53745,#31457,#31458);
#26394=AXIS2_PLACEMENT_3D('',#53746,#31459,#31460);
#26395=AXIS2_PLACEMENT_3D('',#53747,#31461,#31462);
#26396=AXIS2_PLACEMENT_3D('',#53749,#31464,#31465);
#26397=AXIS2_PLACEMENT_3D('',#53751,#31467,#31468);
#26398=AXIS2_PLACEMENT_3D('',#53752,#31469,#31470);
#26399=AXIS2_PLACEMENT_3D('',#53755,#31473,#31474);
#26400=AXIS2_PLACEMENT_3D('',#53756,#31475,#31476);
#26401=AXIS2_PLACEMENT_3D('',#53757,#31477,#31478);
#26402=AXIS2_PLACEMENT_3D('',#53760,#31481,#31482);
#26403=AXIS2_PLACEMENT_3D('',#53761,#31483,#31484);
#26404=AXIS2_PLACEMENT_3D('',#53762,#31485,#31486);
#26405=AXIS2_PLACEMENT_3D('',#53765,#31489,#31490);
#26406=AXIS2_PLACEMENT_3D('',#53766,#31491,#31492);
#26407=AXIS2_PLACEMENT_3D('',#53767,#31493,#31494);
#26408=AXIS2_PLACEMENT_3D('',#53773,#31498,#31499);
#26409=AXIS2_PLACEMENT_3D('',#53775,#31501,#31502);
#26410=AXIS2_PLACEMENT_3D('',#53781,#31505,#31506);
#26411=AXIS2_PLACEMENT_3D('',#53785,#31508,#31509);
#26412=AXIS2_PLACEMENT_3D('',#53789,#31511,#31512);
#26413=AXIS2_PLACEMENT_3D('',#53793,#31514,#31515);
#26414=AXIS2_PLACEMENT_3D('',#53795,#31516,#31517);
#26415=AXIS2_PLACEMENT_3D('',#53797,#31518,#31519);
#26416=AXIS2_PLACEMENT_3D('',#53801,#31521,#31522);
#26417=AXIS2_PLACEMENT_3D('',#53805,#31524,#31525);
#26418=AXIS2_PLACEMENT_3D('',#53809,#31527,#31528);
#26419=AXIS2_PLACEMENT_3D('',#53811,#31529,#31530);
#26420=AXIS2_PLACEMENT_3D('',#53813,#31531,#31532);
#26421=AXIS2_PLACEMENT_3D('',#53821,#31536,#31537);
#26422=AXIS2_PLACEMENT_3D('',#53823,#31538,#31539);
#26423=AXIS2_PLACEMENT_3D('',#53825,#31540,#31541);
#26424=AXIS2_PLACEMENT_3D('',#53829,#31543,#31544);
#26425=AXIS2_PLACEMENT_3D('',#53833,#31546,#31547);
#26426=AXIS2_PLACEMENT_3D('',#53837,#31549,#31550);
#26427=AXIS2_PLACEMENT_3D('',#53839,#31551,#31552);
#26428=AXIS2_PLACEMENT_3D('',#53841,#31553,#31554);
#26429=AXIS2_PLACEMENT_3D('',#53845,#31556,#31557);
#26430=AXIS2_PLACEMENT_3D('',#53849,#31559,#31560);
#26431=AXIS2_PLACEMENT_3D('',#53853,#31562,#31563);
#26432=AXIS2_PLACEMENT_3D('',#53860,#31568,#31569);
#26433=AXIS2_PLACEMENT_3D('',#53867,#31573,#31574);
#26434=AXIS2_PLACEMENT_3D('',#53871,#31576,#31577);
#26435=AXIS2_PLACEMENT_3D('',#53875,#31579,#31580);
#26436=AXIS2_PLACEMENT_3D('',#53879,#31582,#31583);
#26437=AXIS2_PLACEMENT_3D('',#53881,#31584,#31585);
#26438=AXIS2_PLACEMENT_3D('',#53883,#31586,#31587);
#26439=AXIS2_PLACEMENT_3D('',#53887,#31589,#31590);
#26440=AXIS2_PLACEMENT_3D('',#53891,#31592,#31593);
#26441=AXIS2_PLACEMENT_3D('',#53895,#31595,#31596);
#26442=AXIS2_PLACEMENT_3D('',#53897,#31597,#31598);
#26443=AXIS2_PLACEMENT_3D('',#53899,#31599,#31600);
#26444=AXIS2_PLACEMENT_3D('',#53907,#31604,#31605);
#26445=AXIS2_PLACEMENT_3D('',#53909,#31606,#31607);
#26446=AXIS2_PLACEMENT_3D('',#53911,#31608,#31609);
#26447=AXIS2_PLACEMENT_3D('',#53915,#31611,#31612);
#26448=AXIS2_PLACEMENT_3D('',#53919,#31614,#31615);
#26449=AXIS2_PLACEMENT_3D('',#53923,#31617,#31618);
#26450=AXIS2_PLACEMENT_3D('',#53925,#31619,#31620);
#26451=AXIS2_PLACEMENT_3D('',#53927,#31621,#31622);
#26452=AXIS2_PLACEMENT_3D('',#53931,#31624,#31625);
#26453=AXIS2_PLACEMENT_3D('',#53935,#31627,#31628);
#26454=AXIS2_PLACEMENT_3D('',#53939,#31630,#31631);
#26455=AXIS2_PLACEMENT_3D('',#53943,#31634,#31635);
#26456=AXIS2_PLACEMENT_3D('',#53946,#31638,#31639);
#26457=AXIS2_PLACEMENT_3D('',#53949,#31642,#31643);
#26458=AXIS2_PLACEMENT_3D('',#53952,#31646,#31647);
#26459=AXIS2_PLACEMENT_3D('',#53955,#31650,#31651);
#26460=AXIS2_PLACEMENT_3D('',#53958,#31654,#31655);
#26461=AXIS2_PLACEMENT_3D('',#53961,#31658,#31659);
#26462=AXIS2_PLACEMENT_3D('',#53963,#31661,#31662);
#26463=AXIS2_PLACEMENT_3D('',#53965,#31664,#31665);
#26464=AXIS2_PLACEMENT_3D('',#53967,#31667,#31668);
#26465=AXIS2_PLACEMENT_3D('',#53970,#31671,#31672);
#26466=AXIS2_PLACEMENT_3D('',#53973,#31675,#31676);
#26467=AXIS2_PLACEMENT_3D('',#53976,#31679,#31680);
#26468=AXIS2_PLACEMENT_3D('',#53979,#31683,#31684);
#26469=AXIS2_PLACEMENT_3D('',#53981,#31686,#31687);
#26470=AXIS2_PLACEMENT_3D('',#53984,#31690,#31691);
#26471=AXIS2_PLACEMENT_3D('',#53987,#31694,#31695);
#26472=AXIS2_PLACEMENT_3D('',#53988,#31696,#31697);
#26473=AXIS2_PLACEMENT_3D('',#53989,#31698,#31699);
#26474=AXIS2_PLACEMENT_3D('',#53990,#31700,#31701);
#26475=AXIS2_PLACEMENT_3D('',#53991,#31702,#31703);
#26476=AXIS2_PLACEMENT_3D('',#53992,#31704,#31705);
#26477=AXIS2_PLACEMENT_3D('',#53993,#31706,#31707);
#26478=AXIS2_PLACEMENT_3D('',#53994,#31708,#31709);
#26479=AXIS2_PLACEMENT_3D('',#53995,#31710,#31711);
#26480=AXIS2_PLACEMENT_3D('',#53996,#31712,#31713);
#26481=AXIS2_PLACEMENT_3D('',#53999,#31716,#31717);
#26482=AXIS2_PLACEMENT_3D('',#54002,#31720,#31721);
#26483=AXIS2_PLACEMENT_3D('',#54005,#31724,#31725);
#26484=AXIS2_PLACEMENT_3D('',#54008,#31728,#31729);
#26485=AXIS2_PLACEMENT_3D('',#54009,#31730,#31731);
#26486=AXIS2_PLACEMENT_3D('',#54012,#31734,#31735);
#26487=AXIS2_PLACEMENT_3D('',#54015,#31738,#31739);
#26488=AXIS2_PLACEMENT_3D('',#54016,#31740,#31741);
#26489=AXIS2_PLACEMENT_3D('',#54017,#31742,#31743);
#26490=AXIS2_PLACEMENT_3D('',#54018,#31744,#31745);
#26491=AXIS2_PLACEMENT_3D('',#54019,#31746,#31747);
#26492=AXIS2_PLACEMENT_3D('',#54020,#31748,#31749);
#26493=AXIS2_PLACEMENT_3D('',#54021,#31750,#31751);
#26494=AXIS2_PLACEMENT_3D('',#54022,#31752,#31753);
#26495=AXIS2_PLACEMENT_3D('',#54023,#31754,#31755);
#26496=AXIS2_PLACEMENT_3D('',#54024,#31756,#31757);
#26497=AXIS2_PLACEMENT_3D('',#54025,#31758,#31759);
#26498=AXIS2_PLACEMENT_3D('',#54027,#31761,#31762);
#26499=AXIS2_PLACEMENT_3D('',#54028,#31763,#31764);
#26500=AXIS2_PLACEMENT_3D('',#54029,#31765,#31766);
#26501=AXIS2_PLACEMENT_3D('',#54030,#31767,#31768);
#26502=AXIS2_PLACEMENT_3D('',#54031,#31769,#31770);
#26503=AXIS2_PLACEMENT_3D('',#54032,#31771,#31772);
#26504=AXIS2_PLACEMENT_3D('',#54033,#31773,#31774);
#26505=AXIS2_PLACEMENT_3D('',#54034,#31775,#31776);
#26506=AXIS2_PLACEMENT_3D('',#54035,#31777,#31778);
#26507=AXIS2_PLACEMENT_3D('',#54036,#31779,#31780);
#26508=AXIS2_PLACEMENT_3D('',#54037,#31781,#31782);
#26509=AXIS2_PLACEMENT_3D('',#54039,#31783,#31784);
#26510=AXIS2_PLACEMENT_3D('',#54042,#31786,#31787);
#26511=AXIS2_PLACEMENT_3D('',#54043,#31788,#31789);
#26512=AXIS2_PLACEMENT_3D('',#54045,#31790,#31791);
#26513=AXIS2_PLACEMENT_3D('',#54048,#31793,#31794);
#26514=AXIS2_PLACEMENT_3D('',#54049,#31795,#31796);
#26515=AXIS2_PLACEMENT_3D('',#54051,#31797,#31798);
#26516=AXIS2_PLACEMENT_3D('',#54054,#31800,#31801);
#26517=AXIS2_PLACEMENT_3D('',#54055,#31802,#31803);
#26518=AXIS2_PLACEMENT_3D('',#54058,#31805,#31806);
#26519=AXIS2_PLACEMENT_3D('',#54061,#31808,#31809);
#26520=AXIS2_PLACEMENT_3D('',#54063,#31810,#31811);
#26521=AXIS2_PLACEMENT_3D('',#54066,#31813,#31814);
#26522=AXIS2_PLACEMENT_3D('',#54067,#31815,#31816);
#26523=AXIS2_PLACEMENT_3D('',#54069,#31817,#31818);
#26524=AXIS2_PLACEMENT_3D('',#54072,#31820,#31821);
#26525=AXIS2_PLACEMENT_3D('',#54073,#31822,#31823);
#26526=AXIS2_PLACEMENT_3D('',#54075,#31824,#31825);
#26527=AXIS2_PLACEMENT_3D('',#54078,#31827,#31828);
#26528=AXIS2_PLACEMENT_3D('',#54079,#31829,#31830);
#26529=AXIS2_PLACEMENT_3D('',#54081,#31831,#31832);
#26530=AXIS2_PLACEMENT_3D('',#54084,#31834,#31835);
#26531=AXIS2_PLACEMENT_3D('',#54085,#31836,#31837);
#26532=AXIS2_PLACEMENT_3D('',#54087,#31838,#31839);
#26533=AXIS2_PLACEMENT_3D('',#54090,#31841,#31842);
#26534=AXIS2_PLACEMENT_3D('',#54091,#31843,#31844);
#26535=AXIS2_PLACEMENT_3D('',#54093,#31845,#31846);
#26536=AXIS2_PLACEMENT_3D('',#54096,#31848,#31849);
#26537=AXIS2_PLACEMENT_3D('',#54097,#31850,#31851);
#26538=AXIS2_PLACEMENT_3D('',#54099,#31852,#31853);
#26539=AXIS2_PLACEMENT_3D('',#54102,#31855,#31856);
#26540=AXIS2_PLACEMENT_3D('',#54103,#31857,#31858);
#26541=AXIS2_PLACEMENT_3D('',#54105,#31859,#31860);
#26542=AXIS2_PLACEMENT_3D('',#54109,#31862,#31863);
#26543=AXIS2_PLACEMENT_3D('',#54113,#31865,#31866);
#26544=AXIS2_PLACEMENT_3D('',#54115,#31868,#31869);
#26545=AXIS2_PLACEMENT_3D('',#54118,#31871,#31872);
#26546=AXIS2_PLACEMENT_3D('',#54121,#31874,#31875);
#26547=AXIS2_PLACEMENT_3D('',#54123,#31876,#31877);
#26548=AXIS2_PLACEMENT_3D('',#54129,#31880,#31881);
#26549=AXIS2_PLACEMENT_3D('',#54132,#31883,#31884);
#26550=AXIS2_PLACEMENT_3D('',#54199,#31885,#31886);
#26551=AXIS2_PLACEMENT_3D('',#54200,#31887,#31888);
#26552=AXIS2_PLACEMENT_3D('',#54233,#31889,#31890);
#26553=AXIS2_PLACEMENT_3D('',#54235,#31891,#31892);
#26554=AXIS2_PLACEMENT_3D('',#54237,#31894,#31895);
#26555=AXIS2_PLACEMENT_3D('',#54239,#31896,#31897);
#26556=AXIS2_PLACEMENT_3D('',#54242,#31899,#31900);
#26557=AXIS2_PLACEMENT_3D('',#54243,#31901,#31902);
#26558=AXIS2_PLACEMENT_3D('',#54246,#31903,#31904);
#26559=AXIS2_PLACEMENT_3D('',#54252,#31908,#31909);
#26560=AXIS2_PLACEMENT_3D('',#54254,#31910,#31911);
#26561=AXIS2_PLACEMENT_3D('',#54258,#31913,#31914);
#26562=AXIS2_PLACEMENT_3D('',#54260,#31916,#31917);
#26563=AXIS2_PLACEMENT_3D('',#54263,#31918,#31919);
#26564=AXIS2_PLACEMENT_3D('',#54267,#31921,#31922);
#26565=AXIS2_PLACEMENT_3D('',#54269,#31924,#31925);
#26566=AXIS2_PLACEMENT_3D('',#54271,#31926,#31927);
#26567=AXIS2_PLACEMENT_3D('',#54277,#31931,#31932);
#26568=AXIS2_PLACEMENT_3D('',#54286,#31937,#31938);
#26569=AXIS2_PLACEMENT_3D('',#54295,#31943,#31944);
#26570=AXIS2_PLACEMENT_3D('',#54304,#31949,#31950);
#26571=AXIS2_PLACEMENT_3D('',#54313,#31955,#31956);
#26572=AXIS2_PLACEMENT_3D('',#54322,#31961,#31962);
#26573=AXIS2_PLACEMENT_3D('',#54331,#31967,#31968);
#26574=AXIS2_PLACEMENT_3D('',#54340,#31973,#31974);
#26575=AXIS2_PLACEMENT_3D('',#54349,#31979,#31980);
#26576=AXIS2_PLACEMENT_3D('',#54358,#31985,#31986);
#26577=AXIS2_PLACEMENT_3D('',#54364,#31990,#31991);
#26578=AXIS2_PLACEMENT_3D('',#54373,#31996,#31997);
#26579=AXIS2_PLACEMENT_3D('',#54379,#32001,#32002);
#26580=AXIS2_PLACEMENT_3D('',#54388,#32007,#32008);
#26581=AXIS2_PLACEMENT_3D('',#54397,#32013,#32014);
#26582=AXIS2_PLACEMENT_3D('',#54406,#32019,#32020);
#26583=AXIS2_PLACEMENT_3D('',#54415,#32025,#32026);
#26584=AXIS2_PLACEMENT_3D('',#54418,#32029,#32030);
#26585=AXIS2_PLACEMENT_3D('',#54421,#32031,#32032);
#26586=AXIS2_PLACEMENT_3D('',#54425,#32034,#32035);
#26587=AXIS2_PLACEMENT_3D('',#54427,#32037,#32038);
#26588=AXIS2_PLACEMENT_3D('',#54430,#32039,#32040);
#26589=AXIS2_PLACEMENT_3D('',#54434,#32042,#32043);
#26590=AXIS2_PLACEMENT_3D('',#54436,#32045,#32046);
#26591=AXIS2_PLACEMENT_3D('',#54439,#32047,#32048);
#26592=AXIS2_PLACEMENT_3D('',#54443,#32050,#32051);
#26593=AXIS2_PLACEMENT_3D('',#54445,#32053,#32054);
#26594=AXIS2_PLACEMENT_3D('',#54448,#32055,#32056);
#26595=AXIS2_PLACEMENT_3D('',#54452,#32058,#32059);
#26596=AXIS2_PLACEMENT_3D('',#54454,#32061,#32062);
#26597=AXIS2_PLACEMENT_3D('',#54455,#32063,#32064);
#26598=AXIS2_PLACEMENT_3D('',#54456,#32065,#32066);
#26599=AXIS2_PLACEMENT_3D('',#54457,#32067,#32068);
#26600=AXIS2_PLACEMENT_3D('',#54458,#32069,#32070);
#26601=AXIS2_PLACEMENT_3D('',#54459,#32071,#32072);
#26602=AXIS2_PLACEMENT_3D('',#54460,#32073,#32074);
#26603=AXIS2_PLACEMENT_3D('',#54461,#32075,#32076);
#26604=AXIS2_PLACEMENT_3D('',#54462,#32077,#32078);
#26605=AXIS2_PLACEMENT_3D('',#54463,#32079,#32080);
#26606=AXIS2_PLACEMENT_3D('',#54464,#32081,#32082);
#26607=AXIS2_PLACEMENT_3D('',#54465,#32083,#32084);
#26608=AXIS2_PLACEMENT_3D('',#54466,#32085,#32086);
#26609=AXIS2_PLACEMENT_3D('',#54467,#32087,#32088);
#26610=AXIS2_PLACEMENT_3D('',#54468,#32089,#32090);
#26611=AXIS2_PLACEMENT_3D('',#54469,#32091,#32092);
#26612=AXIS2_PLACEMENT_3D('',#54470,#32093,#32094);
#26613=AXIS2_PLACEMENT_3D('',#54471,#32095,#32096);
#26614=AXIS2_PLACEMENT_3D('',#54472,#32097,#32098);
#26615=AXIS2_PLACEMENT_3D('',#54473,#32099,#32100);
#26616=AXIS2_PLACEMENT_3D('',#54474,#32101,#32102);
#26617=AXIS2_PLACEMENT_3D('',#54475,#32103,#32104);
#26618=AXIS2_PLACEMENT_3D('',#54476,#32105,#32106);
#26619=AXIS2_PLACEMENT_3D('',#54477,#32107,#32108);
#26620=AXIS2_PLACEMENT_3D('',#54478,#32109,#32110);
#26621=AXIS2_PLACEMENT_3D('',#54479,#32111,#32112);
#26622=AXIS2_PLACEMENT_3D('',#54480,#32113,#32114);
#26623=AXIS2_PLACEMENT_3D('',#54481,#32115,#32116);
#26624=AXIS2_PLACEMENT_3D('',#54482,#32117,#32118);
#26625=AXIS2_PLACEMENT_3D('',#54483,#32119,#32120);
#26626=AXIS2_PLACEMENT_3D('',#54484,#32121,#32122);
#26627=AXIS2_PLACEMENT_3D('',#54485,#32123,#32124);
#26628=AXIS2_PLACEMENT_3D('',#54486,#32125,#32126);
#26629=AXIS2_PLACEMENT_3D('',#54487,#32127,#32128);
#26630=AXIS2_PLACEMENT_3D('',#54488,#32129,#32130);
#26631=AXIS2_PLACEMENT_3D('',#54489,#32131,#32132);
#26632=AXIS2_PLACEMENT_3D('',#54490,#32133,#32134);
#26633=AXIS2_PLACEMENT_3D('',#54491,#32135,#32136);
#26634=AXIS2_PLACEMENT_3D('',#54492,#32137,#32138);
#26635=AXIS2_PLACEMENT_3D('',#54493,#32139,#32140);
#26636=AXIS2_PLACEMENT_3D('',#54494,#32141,#32142);
#26637=AXIS2_PLACEMENT_3D('',#54495,#32143,#32144);
#26638=AXIS2_PLACEMENT_3D('',#54496,#32145,#32146);
#26639=AXIS2_PLACEMENT_3D('',#54497,#32147,#32148);
#26640=AXIS2_PLACEMENT_3D('',#54498,#32149,#32150);
#26641=AXIS2_PLACEMENT_3D('',#54499,#32151,#32152);
#26642=AXIS2_PLACEMENT_3D('',#54500,#32153,#32154);
#26643=AXIS2_PLACEMENT_3D('',#54501,#32155,#32156);
#26644=AXIS2_PLACEMENT_3D('',#54502,#32157,#32158);
#26645=AXIS2_PLACEMENT_3D('',#54503,#32159,#32160);
#26646=AXIS2_PLACEMENT_3D('',#54512,#32165,#32166);
#26647=AXIS2_PLACEMENT_3D('',#54523,#32173,#32174);
#26648=AXIS2_PLACEMENT_3D('',#54527,#32177,#32178);
#26649=AXIS2_PLACEMENT_3D('',#54531,#32181,#32182);
#26650=AXIS2_PLACEMENT_3D('',#54533,#32184,#32185);
#26651=AXIS2_PLACEMENT_3D('',#54537,#32188,#32189);
#26652=AXIS2_PLACEMENT_3D('',#54541,#32192,#32193);
#26653=AXIS2_PLACEMENT_3D('',#54543,#32195,#32196);
#26654=AXIS2_PLACEMENT_3D('',#54549,#32200,#32201);
#26655=AXIS2_PLACEMENT_3D('',#54553,#32204,#32205);
#26656=AXIS2_PLACEMENT_3D('',#54557,#32208,#32209);
#26657=AXIS2_PLACEMENT_3D('',#54561,#32212,#32213);
#26658=AXIS2_PLACEMENT_3D('',#54565,#32216,#32217);
#26659=AXIS2_PLACEMENT_3D('',#54567,#32219,#32220);
#26660=AXIS2_PLACEMENT_3D('',#54568,#32221,#32222);
#26661=AXIS2_PLACEMENT_3D('',#54573,#32224,#32225);
#26662=AXIS2_PLACEMENT_3D('',#54577,#32227,#32228);
#26663=AXIS2_PLACEMENT_3D('',#54581,#32230,#32231);
#26664=AXIS2_PLACEMENT_3D('',#54583,#32232,#32233);
#26665=AXIS2_PLACEMENT_3D('',#54585,#32234,#32235);
#26666=AXIS2_PLACEMENT_3D('',#54589,#32237,#32238);
#26667=AXIS2_PLACEMENT_3D('',#54593,#32240,#32241);
#26668=AXIS2_PLACEMENT_3D('',#54597,#32243,#32244);
#26669=AXIS2_PLACEMENT_3D('',#54599,#32245,#32246);
#26670=AXIS2_PLACEMENT_3D('',#54601,#32247,#32248);
#26671=AXIS2_PLACEMENT_3D('',#54609,#32252,#32253);
#26672=AXIS2_PLACEMENT_3D('',#54611,#32254,#32255);
#26673=AXIS2_PLACEMENT_3D('',#54613,#32256,#32257);
#26674=AXIS2_PLACEMENT_3D('',#54617,#32259,#32260);
#26675=AXIS2_PLACEMENT_3D('',#54621,#32262,#32263);
#26676=AXIS2_PLACEMENT_3D('',#54625,#32265,#32266);
#26677=AXIS2_PLACEMENT_3D('',#54627,#32267,#32268);
#26678=AXIS2_PLACEMENT_3D('',#54629,#32269,#32270);
#26679=AXIS2_PLACEMENT_3D('',#54633,#32272,#32273);
#26680=AXIS2_PLACEMENT_3D('',#54637,#32275,#32276);
#26681=AXIS2_PLACEMENT_3D('',#54657,#32287,#32288);
#26682=AXIS2_PLACEMENT_3D('',#54663,#32292,#32293);
#26683=AXIS2_PLACEMENT_3D('',#54665,#32294,#32295);
#26684=AXIS2_PLACEMENT_3D('',#54667,#32297,#32298);
#26685=AXIS2_PLACEMENT_3D('',#54671,#32301,#32302);
#26686=AXIS2_PLACEMENT_3D('',#54673,#32303,#32304);
#26687=AXIS2_PLACEMENT_3D('',#54675,#32306,#32307);
#26688=AXIS2_PLACEMENT_3D('',#54679,#32310,#32311);
#26689=AXIS2_PLACEMENT_3D('',#54681,#32312,#32313);
#26690=AXIS2_PLACEMENT_3D('',#54683,#32315,#32316);
#26691=AXIS2_PLACEMENT_3D('',#54685,#32317,#32318);
#26692=AXIS2_PLACEMENT_3D('',#54687,#32320,#32321);
#26693=AXIS2_PLACEMENT_3D('',#54689,#32322,#32323);
#26694=AXIS2_PLACEMENT_3D('',#54691,#32325,#32326);
#26695=AXIS2_PLACEMENT_3D('',#54695,#32329,#32330);
#26696=AXIS2_PLACEMENT_3D('',#54697,#32331,#32332);
#26697=AXIS2_PLACEMENT_3D('',#54699,#32334,#32335);
#26698=AXIS2_PLACEMENT_3D('',#54703,#32338,#32339);
#26699=AXIS2_PLACEMENT_3D('',#54705,#32340,#32341);
#26700=AXIS2_PLACEMENT_3D('',#54707,#32343,#32344);
#26701=AXIS2_PLACEMENT_3D('',#54711,#32347,#32348);
#26702=AXIS2_PLACEMENT_3D('',#54713,#32349,#32350);
#26703=AXIS2_PLACEMENT_3D('',#54715,#32352,#32353);
#26704=AXIS2_PLACEMENT_3D('',#54717,#32354,#32355);
#26705=AXIS2_PLACEMENT_3D('',#54719,#32357,#32358);
#26706=AXIS2_PLACEMENT_3D('',#54721,#32359,#32360);
#26707=AXIS2_PLACEMENT_3D('',#54723,#32362,#32363);
#26708=AXIS2_PLACEMENT_3D('',#54727,#32366,#32367);
#26709=AXIS2_PLACEMENT_3D('',#54731,#32370,#32371);
#26710=AXIS2_PLACEMENT_3D('',#54735,#32374,#32375);
#26711=AXIS2_PLACEMENT_3D('',#54737,#32376,#32377);
#26712=AXIS2_PLACEMENT_3D('',#54739,#32379,#32380);
#26713=AXIS2_PLACEMENT_3D('',#54741,#32381,#32382);
#26714=AXIS2_PLACEMENT_3D('',#54743,#32384,#32385);
#26715=AXIS2_PLACEMENT_3D('',#54745,#32386,#32387);
#26716=AXIS2_PLACEMENT_3D('',#54747,#32389,#32390);
#26717=AXIS2_PLACEMENT_3D('',#54751,#32393,#32394);
#26718=AXIS2_PLACEMENT_3D('',#54753,#32395,#32396);
#26719=AXIS2_PLACEMENT_3D('',#54755,#32398,#32399);
#26720=AXIS2_PLACEMENT_3D('',#54759,#32402,#32403);
#26721=AXIS2_PLACEMENT_3D('',#54761,#32404,#32405);
#26722=AXIS2_PLACEMENT_3D('',#54763,#32407,#32408);
#26723=AXIS2_PLACEMENT_3D('',#54767,#32411,#32412);
#26724=AXIS2_PLACEMENT_3D('',#54769,#32413,#32414);
#26725=AXIS2_PLACEMENT_3D('',#54771,#32416,#32417);
#26726=AXIS2_PLACEMENT_3D('',#54773,#32418,#32419);
#26727=AXIS2_PLACEMENT_3D('',#54775,#32421,#32422);
#26728=AXIS2_PLACEMENT_3D('',#54777,#32423,#32424);
#26729=AXIS2_PLACEMENT_3D('',#54779,#32426,#32427);
#26730=AXIS2_PLACEMENT_3D('',#54783,#32430,#32431);
#26731=AXIS2_PLACEMENT_3D('',#54785,#32432,#32433);
#26732=AXIS2_PLACEMENT_3D('',#54787,#32435,#32436);
#26733=AXIS2_PLACEMENT_3D('',#54791,#32439,#32440);
#26734=AXIS2_PLACEMENT_3D('',#54793,#32441,#32442);
#26735=AXIS2_PLACEMENT_3D('',#54795,#32444,#32445);
#26736=AXIS2_PLACEMENT_3D('',#54799,#32448,#32449);
#26737=AXIS2_PLACEMENT_3D('',#54803,#32452,#32453);
#26738=AXIS2_PLACEMENT_3D('',#54807,#32456,#32457);
#26739=AXIS2_PLACEMENT_3D('',#54811,#32460,#32461);
#26740=AXIS2_PLACEMENT_3D('',#54815,#32464,#32465);
#26741=AXIS2_PLACEMENT_3D('',#54819,#32468,#32469);
#26742=AXIS2_PLACEMENT_3D('',#54823,#32472,#32473);
#26743=AXIS2_PLACEMENT_3D('',#54827,#32476,#32477);
#26744=AXIS2_PLACEMENT_3D('',#54831,#32480,#32481);
#26745=AXIS2_PLACEMENT_3D('',#54833,#32483,#32484);
#26746=AXIS2_PLACEMENT_3D('',#54834,#32485,#32486);
#26747=AXIS2_PLACEMENT_3D('',#54838,#32488,#32489);
#26748=AXIS2_PLACEMENT_3D('',#54840,#32491,#32492);
#26749=AXIS2_PLACEMENT_3D('',#54847,#32495,#32496);
#26750=AXIS2_PLACEMENT_3D('',#54863,#32504,#32505);
#26751=AXIS2_PLACEMENT_3D('',#54867,#32507,#32508);
#26752=AXIS2_PLACEMENT_3D('',#54871,#32510,#32511);
#26753=AXIS2_PLACEMENT_3D('',#54873,#32512,#32513);
#26754=AXIS2_PLACEMENT_3D('',#54875,#32514,#32515);
#26755=AXIS2_PLACEMENT_3D('',#54879,#32517,#32518);
#26756=AXIS2_PLACEMENT_3D('',#54883,#32520,#32521);
#26757=AXIS2_PLACEMENT_3D('',#54887,#32523,#32524);
#26758=AXIS2_PLACEMENT_3D('',#54889,#32525,#32526);
#26759=AXIS2_PLACEMENT_3D('',#54891,#32527,#32528);
#26760=AXIS2_PLACEMENT_3D('',#54899,#32532,#32533);
#26761=AXIS2_PLACEMENT_3D('',#54901,#32534,#32535);
#26762=AXIS2_PLACEMENT_3D('',#54903,#32536,#32537);
#26763=AXIS2_PLACEMENT_3D('',#54907,#32539,#32540);
#26764=AXIS2_PLACEMENT_3D('',#54911,#32542,#32543);
#26765=AXIS2_PLACEMENT_3D('',#54915,#32545,#32546);
#26766=AXIS2_PLACEMENT_3D('',#54917,#32547,#32548);
#26767=AXIS2_PLACEMENT_3D('',#54919,#32549,#32550);
#26768=AXIS2_PLACEMENT_3D('',#54923,#32552,#32553);
#26769=AXIS2_PLACEMENT_3D('',#54927,#32555,#32556);
#26770=AXIS2_PLACEMENT_3D('',#54937,#32562,#32563);
#26771=AXIS2_PLACEMENT_3D('',#54941,#32566,#32567);
#26772=AXIS2_PLACEMENT_3D('',#54945,#32570,#32571);
#26773=AXIS2_PLACEMENT_3D('',#54946,#32572,#32573);
#26774=AXIS2_PLACEMENT_3D('',#54947,#32574,#32575);
#26775=AXIS2_PLACEMENT_3D('',#54948,#32576,#32577);
#26776=AXIS2_PLACEMENT_3D('',#54952,#32579,#32580);
#26777=AXIS2_PLACEMENT_3D('',#54954,#32582,#32583);
#26778=AXIS2_PLACEMENT_3D('',#54960,#32587,#32588);
#26779=AXIS2_PLACEMENT_3D('',#54964,#32591,#32592);
#26780=AXIS2_PLACEMENT_3D('',#54968,#32595,#32596);
#26781=AXIS2_PLACEMENT_3D('',#54972,#32599,#32600);
#26782=AXIS2_PLACEMENT_3D('',#54981,#32606,#32607);
#26783=AXIS2_PLACEMENT_3D('',#54985,#32610,#32611);
#26784=AXIS2_PLACEMENT_3D('',#54989,#32614,#32615);
#26785=AXIS2_PLACEMENT_3D('',#54993,#32618,#32619);
#26786=AXIS2_PLACEMENT_3D('',#54997,#32622,#32623);
#26787=AXIS2_PLACEMENT_3D('',#55001,#32626,#32627);
#26788=AXIS2_PLACEMENT_3D('',#55003,#32628,#32629);
#26789=AXIS2_PLACEMENT_3D('',#55005,#32631,#32632);
#26790=AXIS2_PLACEMENT_3D('',#55009,#32635,#32636);
#26791=AXIS2_PLACEMENT_3D('',#55011,#32637,#32638);
#26792=AXIS2_PLACEMENT_3D('',#55013,#32640,#32641);
#26793=AXIS2_PLACEMENT_3D('',#55017,#32644,#32645);
#26794=AXIS2_PLACEMENT_3D('',#55019,#32646,#32647);
#26795=AXIS2_PLACEMENT_3D('',#55021,#32649,#32650);
#26796=AXIS2_PLACEMENT_3D('',#55023,#32651,#32652);
#26797=AXIS2_PLACEMENT_3D('',#55025,#32654,#32655);
#26798=AXIS2_PLACEMENT_3D('',#55027,#32656,#32657);
#26799=AXIS2_PLACEMENT_3D('',#55029,#32659,#32660);
#26800=AXIS2_PLACEMENT_3D('',#55033,#32663,#32664);
#26801=AXIS2_PLACEMENT_3D('',#55035,#32665,#32666);
#26802=AXIS2_PLACEMENT_3D('',#55037,#32668,#32669);
#26803=AXIS2_PLACEMENT_3D('',#55041,#32672,#32673);
#26804=AXIS2_PLACEMENT_3D('',#55043,#32674,#32675);
#26805=AXIS2_PLACEMENT_3D('',#55045,#32677,#32678);
#26806=AXIS2_PLACEMENT_3D('',#55049,#32681,#32682);
#26807=AXIS2_PLACEMENT_3D('',#55051,#32683,#32684);
#26808=AXIS2_PLACEMENT_3D('',#55053,#32686,#32687);
#26809=AXIS2_PLACEMENT_3D('',#55055,#32688,#32689);
#26810=AXIS2_PLACEMENT_3D('',#55057,#32691,#32692);
#26811=AXIS2_PLACEMENT_3D('',#55059,#32693,#32694);
#26812=AXIS2_PLACEMENT_3D('',#55061,#32696,#32697);
#26813=AXIS2_PLACEMENT_3D('',#55065,#32700,#32701);
#26814=AXIS2_PLACEMENT_3D('',#55069,#32704,#32705);
#26815=AXIS2_PLACEMENT_3D('',#55073,#32708,#32709);
#26816=AXIS2_PLACEMENT_3D('',#55075,#32710,#32711);
#26817=AXIS2_PLACEMENT_3D('',#55077,#32713,#32714);
#26818=AXIS2_PLACEMENT_3D('',#55079,#32715,#32716);
#26819=AXIS2_PLACEMENT_3D('',#55081,#32718,#32719);
#26820=AXIS2_PLACEMENT_3D('',#55083,#32720,#32721);
#26821=AXIS2_PLACEMENT_3D('',#55085,#32723,#32724);
#26822=AXIS2_PLACEMENT_3D('',#55089,#32727,#32728);
#26823=AXIS2_PLACEMENT_3D('',#55091,#32729,#32730);
#26824=AXIS2_PLACEMENT_3D('',#55093,#32732,#32733);
#26825=AXIS2_PLACEMENT_3D('',#55097,#32736,#32737);
#26826=AXIS2_PLACEMENT_3D('',#55099,#32738,#32739);
#26827=AXIS2_PLACEMENT_3D('',#55101,#32741,#32742);
#26828=AXIS2_PLACEMENT_3D('',#55105,#32745,#32746);
#26829=AXIS2_PLACEMENT_3D('',#55107,#32747,#32748);
#26830=AXIS2_PLACEMENT_3D('',#55109,#32750,#32751);
#26831=AXIS2_PLACEMENT_3D('',#55111,#32752,#32753);
#26832=AXIS2_PLACEMENT_3D('',#55113,#32755,#32756);
#26833=AXIS2_PLACEMENT_3D('',#55115,#32757,#32758);
#26834=AXIS2_PLACEMENT_3D('',#55117,#32760,#32761);
#26835=AXIS2_PLACEMENT_3D('',#55121,#32764,#32765);
#26836=AXIS2_PLACEMENT_3D('',#55123,#32766,#32767);
#26837=AXIS2_PLACEMENT_3D('',#55125,#32769,#32770);
#26838=AXIS2_PLACEMENT_3D('',#55129,#32773,#32774);
#26839=AXIS2_PLACEMENT_3D('',#55131,#32775,#32776);
#26840=AXIS2_PLACEMENT_3D('',#55133,#32778,#32779);
#26841=AXIS2_PLACEMENT_3D('',#55135,#32781,#32782);
#26842=AXIS2_PLACEMENT_3D('',#55136,#32783,#32784);
#26843=AXIS2_PLACEMENT_3D('',#55145,#32789,#32790);
#26844=AXIS2_PLACEMENT_3D('',#55154,#32795,#32796);
#26845=AXIS2_PLACEMENT_3D('',#55158,#32799,#32800);
#26846=AXIS2_PLACEMENT_3D('',#55162,#32803,#32804);
#26847=AXIS2_PLACEMENT_3D('',#55163,#32805,#32806);
#26848=AXIS2_PLACEMENT_3D('',#55164,#32807,#32808);
#26849=AXIS2_PLACEMENT_3D('',#55166,#32809,#32810);
#26850=AXIS2_PLACEMENT_3D('',#55168,#32811,#32812);
#26851=AXIS2_PLACEMENT_3D('',#55170,#32814,#32815);
#26852=AXIS2_PLACEMENT_3D('',#55178,#32820,#32821);
#26853=AXIS2_PLACEMENT_3D('',#55184,#32825,#32826);
#26854=AXIS2_PLACEMENT_3D('',#55193,#32831,#32832);
#26855=AXIS2_PLACEMENT_3D('',#55196,#32834,#32835);
#26856=AXIS2_PLACEMENT_3D('',#55200,#32838,#32839);
#26857=AXIS2_PLACEMENT_3D('',#55203,#32841,#32842);
#26858=AXIS2_PLACEMENT_3D('',#55204,#32843,#32844);
#26859=AXIS2_PLACEMENT_3D('',#55227,#32855,#32856);
#26860=AXIS2_PLACEMENT_3D('',#55231,#32858,#32859);
#26861=AXIS2_PLACEMENT_3D('',#55235,#32861,#32862);
#26862=AXIS2_PLACEMENT_3D('',#55237,#32863,#32864);
#26863=AXIS2_PLACEMENT_3D('',#55239,#32865,#32866);
#26864=AXIS2_PLACEMENT_3D('',#55243,#32868,#32869);
#26865=AXIS2_PLACEMENT_3D('',#55247,#32871,#32872);
#26866=AXIS2_PLACEMENT_3D('',#55251,#32874,#32875);
#26867=AXIS2_PLACEMENT_3D('',#55253,#32876,#32877);
#26868=AXIS2_PLACEMENT_3D('',#55255,#32878,#32879);
#26869=AXIS2_PLACEMENT_3D('',#55263,#32883,#32884);
#26870=AXIS2_PLACEMENT_3D('',#55265,#32885,#32886);
#26871=AXIS2_PLACEMENT_3D('',#55267,#32887,#32888);
#26872=AXIS2_PLACEMENT_3D('',#55271,#32890,#32891);
#26873=AXIS2_PLACEMENT_3D('',#55275,#32893,#32894);
#26874=AXIS2_PLACEMENT_3D('',#55279,#32896,#32897);
#26875=AXIS2_PLACEMENT_3D('',#55281,#32898,#32899);
#26876=AXIS2_PLACEMENT_3D('',#55283,#32900,#32901);
#26877=AXIS2_PLACEMENT_3D('',#55287,#32903,#32904);
#26878=AXIS2_PLACEMENT_3D('',#55291,#32906,#32907);
#26879=AXIS2_PLACEMENT_3D('',#55293,#32909,#32910);
#26880=AXIS2_PLACEMENT_3D('',#55297,#32913,#32914);
#26881=AXIS2_PLACEMENT_3D('',#55301,#32917,#32918);
#26882=AXIS2_PLACEMENT_3D('',#55307,#32922,#32923);
#26883=AXIS2_PLACEMENT_3D('',#55313,#32927,#32928);
#26884=AXIS2_PLACEMENT_3D('',#55319,#32932,#32933);
#26885=AXIS2_PLACEMENT_3D('',#55325,#32937,#32938);
#26886=AXIS2_PLACEMENT_3D('',#55326,#32939,#32940);
#26887=AXIS2_PLACEMENT_3D('',#55327,#32941,#32942);
#26888=AXIS2_PLACEMENT_3D('',#55328,#32943,#32944);
#26889=AXIS2_PLACEMENT_3D('',#55329,#32945,#32946);
#26890=AXIS2_PLACEMENT_3D('',#55331,#32947,#32948);
#26891=AXIS2_PLACEMENT_3D('',#55337,#32952,#32953);
#26892=AXIS2_PLACEMENT_3D('',#55343,#32957,#32958);
#26893=AXIS2_PLACEMENT_3D('',#55345,#32959,#32960);
#26894=AXIS2_PLACEMENT_3D('',#55349,#32963,#32964);
#26895=AXIS2_PLACEMENT_3D('',#55355,#32968,#32969);
#26896=AXIS2_PLACEMENT_3D('',#55359,#32972,#32973);
#26897=AXIS2_PLACEMENT_3D('',#55360,#32974,#32975);
#26898=AXIS2_PLACEMENT_3D('',#55362,#32976,#32977);
#26899=AXIS2_PLACEMENT_3D('',#55366,#32980,#32981);
#26900=AXIS2_PLACEMENT_3D('',#55367,#32982,#32983);
#26901=AXIS2_PLACEMENT_3D('',#55368,#32984,#32985);
#26902=AXIS2_PLACEMENT_3D('',#55369,#32986,#32987);
#26903=AXIS2_PLACEMENT_3D('',#55375,#32991,#32992);
#26904=AXIS2_PLACEMENT_3D('',#55379,#32995,#32996);
#26905=AXIS2_PLACEMENT_3D('',#55383,#32999,#33000);
#26906=AXIS2_PLACEMENT_3D('',#55387,#33003,#33004);
#26907=AXIS2_PLACEMENT_3D('',#55391,#33007,#33008);
#26908=AXIS2_PLACEMENT_3D('',#55395,#33011,#33012);
#26909=AXIS2_PLACEMENT_3D('',#55399,#33015,#33016);
#26910=AXIS2_PLACEMENT_3D('',#55403,#33019,#33020);
#26911=AXIS2_PLACEMENT_3D('',#55407,#33023,#33024);
#26912=AXIS2_PLACEMENT_3D('',#55411,#33027,#33028);
#26913=AXIS2_PLACEMENT_3D('',#55413,#33029,#33030);
#26914=AXIS2_PLACEMENT_3D('',#55415,#33032,#33033);
#26915=AXIS2_PLACEMENT_3D('',#55419,#33036,#33037);
#26916=AXIS2_PLACEMENT_3D('',#55421,#33038,#33039);
#26917=AXIS2_PLACEMENT_3D('',#55423,#33041,#33042);
#26918=AXIS2_PLACEMENT_3D('',#55427,#33045,#33046);
#26919=AXIS2_PLACEMENT_3D('',#55429,#33047,#33048);
#26920=AXIS2_PLACEMENT_3D('',#55431,#33050,#33051);
#26921=AXIS2_PLACEMENT_3D('',#55433,#33052,#33053);
#26922=AXIS2_PLACEMENT_3D('',#55435,#33055,#33056);
#26923=AXIS2_PLACEMENT_3D('',#55437,#33057,#33058);
#26924=AXIS2_PLACEMENT_3D('',#55439,#33060,#33061);
#26925=AXIS2_PLACEMENT_3D('',#55443,#33064,#33065);
#26926=AXIS2_PLACEMENT_3D('',#55445,#33066,#33067);
#26927=AXIS2_PLACEMENT_3D('',#55447,#33069,#33070);
#26928=AXIS2_PLACEMENT_3D('',#55451,#33073,#33074);
#26929=AXIS2_PLACEMENT_3D('',#55453,#33075,#33076);
#26930=AXIS2_PLACEMENT_3D('',#55455,#33078,#33079);
#26931=AXIS2_PLACEMENT_3D('',#55459,#33082,#33083);
#26932=AXIS2_PLACEMENT_3D('',#55461,#33084,#33085);
#26933=AXIS2_PLACEMENT_3D('',#55463,#33087,#33088);
#26934=AXIS2_PLACEMENT_3D('',#55465,#33089,#33090);
#26935=AXIS2_PLACEMENT_3D('',#55467,#33092,#33093);
#26936=AXIS2_PLACEMENT_3D('',#55469,#33094,#33095);
#26937=AXIS2_PLACEMENT_3D('',#55471,#33097,#33098);
#26938=AXIS2_PLACEMENT_3D('',#55475,#33101,#33102);
#26939=AXIS2_PLACEMENT_3D('',#55479,#33105,#33106);
#26940=AXIS2_PLACEMENT_3D('',#55483,#33109,#33110);
#26941=AXIS2_PLACEMENT_3D('',#55485,#33111,#33112);
#26942=AXIS2_PLACEMENT_3D('',#55487,#33114,#33115);
#26943=AXIS2_PLACEMENT_3D('',#55489,#33116,#33117);
#26944=AXIS2_PLACEMENT_3D('',#55491,#33119,#33120);
#26945=AXIS2_PLACEMENT_3D('',#55493,#33121,#33122);
#26946=AXIS2_PLACEMENT_3D('',#55495,#33124,#33125);
#26947=AXIS2_PLACEMENT_3D('',#55499,#33128,#33129);
#26948=AXIS2_PLACEMENT_3D('',#55501,#33130,#33131);
#26949=AXIS2_PLACEMENT_3D('',#55503,#33133,#33134);
#26950=AXIS2_PLACEMENT_3D('',#55507,#33137,#33138);
#26951=AXIS2_PLACEMENT_3D('',#55509,#33139,#33140);
#26952=AXIS2_PLACEMENT_3D('',#55511,#33142,#33143);
#26953=AXIS2_PLACEMENT_3D('',#55515,#33146,#33147);
#26954=AXIS2_PLACEMENT_3D('',#55517,#33148,#33149);
#26955=AXIS2_PLACEMENT_3D('',#55519,#33151,#33152);
#26956=AXIS2_PLACEMENT_3D('',#55521,#33153,#33154);
#26957=AXIS2_PLACEMENT_3D('',#55523,#33156,#33157);
#26958=AXIS2_PLACEMENT_3D('',#55525,#33158,#33159);
#26959=AXIS2_PLACEMENT_3D('',#55527,#33161,#33162);
#26960=AXIS2_PLACEMENT_3D('',#55531,#33165,#33166);
#26961=AXIS2_PLACEMENT_3D('',#55533,#33167,#33168);
#26962=AXIS2_PLACEMENT_3D('',#55535,#33170,#33171);
#26963=AXIS2_PLACEMENT_3D('',#55539,#33174,#33175);
#26964=AXIS2_PLACEMENT_3D('',#55541,#33176,#33177);
#26965=AXIS2_PLACEMENT_3D('',#55543,#33179,#33180);
#26966=AXIS2_PLACEMENT_3D('',#55545,#33182,#33183);
#26967=AXIS2_PLACEMENT_3D('',#55554,#33188,#33189);
#26968=AXIS2_PLACEMENT_3D('',#55560,#33193,#33194);
#26969=AXIS2_PLACEMENT_3D('',#55566,#33198,#33199);
#26970=AXIS2_PLACEMENT_3D('',#55572,#33203,#33204);
#26971=AXIS2_PLACEMENT_3D('',#55578,#33208,#33209);
#26972=AXIS2_PLACEMENT_3D('',#55587,#33214,#33215);
#26973=AXIS2_PLACEMENT_3D('',#55593,#33219,#33220);
#26974=AXIS2_PLACEMENT_3D('',#55599,#33224,#33225);
#26975=AXIS2_PLACEMENT_3D('',#55602,#33228,#33229);
#26976=AXIS2_PLACEMENT_3D('',#55610,#33234,#33235);
#26977=AXIS2_PLACEMENT_3D('',#55616,#33239,#33240);
#26978=AXIS2_PLACEMENT_3D('',#55622,#33244,#33245);
#26979=AXIS2_PLACEMENT_3D('',#55628,#33249,#33250);
#26980=AXIS2_PLACEMENT_3D('',#55634,#33254,#33255);
#26981=AXIS2_PLACEMENT_3D('',#55640,#33259,#33260);
#26982=AXIS2_PLACEMENT_3D('',#55646,#33264,#33265);
#26983=AXIS2_PLACEMENT_3D('',#55652,#33269,#33270);
#26984=AXIS2_PLACEMENT_3D('',#55658,#33274,#33275);
#26985=AXIS2_PLACEMENT_3D('',#55664,#33279,#33280);
#26986=AXIS2_PLACEMENT_3D('',#55670,#33284,#33285);
#26987=AXIS2_PLACEMENT_3D('',#55676,#33289,#33290);
#26988=AXIS2_PLACEMENT_3D('',#55682,#33294,#33295);
#26989=AXIS2_PLACEMENT_3D('',#55688,#33299,#33300);
#26990=AXIS2_PLACEMENT_3D('',#55693,#33304,#33305);
#26991=AXIS2_PLACEMENT_3D('',#55695,#33306,#33307);
#26992=AXIS2_PLACEMENT_3D('',#55699,#33310,#33311);
#26993=AXIS2_PLACEMENT_3D('',#55705,#33315,#33316);
#26994=AXIS2_PLACEMENT_3D('',#55707,#33317,#33318);
#26995=AXIS2_PLACEMENT_3D('',#55711,#33321,#33322);
#26996=AXIS2_PLACEMENT_3D('',#55713,#33323,#33324);
#26997=AXIS2_PLACEMENT_3D('',#55717,#33327,#33328);
#26998=AXIS2_PLACEMENT_3D('',#55723,#33332,#33333);
#26999=AXIS2_PLACEMENT_3D('',#55725,#33335,#33336);
#27000=AXIS2_PLACEMENT_3D('',#55726,#33337,#33338);
#27001=AXIS2_PLACEMENT_3D('',#55727,#33339,#33340);
#27002=AXIS2_PLACEMENT_3D('',#55731,#33343,#33344);
#27003=AXIS2_PLACEMENT_3D('',#55737,#33348,#33349);
#27004=AXIS2_PLACEMENT_3D('',#55743,#33353,#33354);
#27005=AXIS2_PLACEMENT_3D('',#55748,#33358,#33359);
#27006=AXIS2_PLACEMENT_3D('',#55749,#33360,#33361);
#27007=AXIS2_PLACEMENT_3D('',#55751,#33363,#33364);
#27008=AXIS2_PLACEMENT_3D('',#55757,#33367,#33368);
#27009=AXIS2_PLACEMENT_3D('',#55761,#33370,#33371);
#27010=AXIS2_PLACEMENT_3D('',#55765,#33373,#33374);
#27011=AXIS2_PLACEMENT_3D('',#55767,#33375,#33376);
#27012=AXIS2_PLACEMENT_3D('',#55769,#33377,#33378);
#27013=AXIS2_PLACEMENT_3D('',#55773,#33380,#33381);
#27014=AXIS2_PLACEMENT_3D('',#55777,#33383,#33384);
#27015=AXIS2_PLACEMENT_3D('',#55781,#33386,#33387);
#27016=AXIS2_PLACEMENT_3D('',#55783,#33388,#33389);
#27017=AXIS2_PLACEMENT_3D('',#55785,#33390,#33391);
#27018=AXIS2_PLACEMENT_3D('',#55793,#33395,#33396);
#27019=AXIS2_PLACEMENT_3D('',#55795,#33397,#33398);
#27020=AXIS2_PLACEMENT_3D('',#55797,#33399,#33400);
#27021=AXIS2_PLACEMENT_3D('',#55801,#33402,#33403);
#27022=AXIS2_PLACEMENT_3D('',#55805,#33405,#33406);
#27023=AXIS2_PLACEMENT_3D('',#55809,#33408,#33409);
#27024=AXIS2_PLACEMENT_3D('',#55811,#33410,#33411);
#27025=AXIS2_PLACEMENT_3D('',#55813,#33412,#33413);
#27026=AXIS2_PLACEMENT_3D('',#55817,#33415,#33416);
#27027=AXIS2_PLACEMENT_3D('',#55821,#33418,#33419);
#27028=AXIS2_PLACEMENT_3D('',#55825,#33422,#33423);
#27029=AXIS2_PLACEMENT_3D('',#55851,#33437,#33438);
#27030=AXIS2_PLACEMENT_3D('',#55857,#33442,#33443);
#27031=AXIS2_PLACEMENT_3D('',#55863,#33447,#33448);
#27032=AXIS2_PLACEMENT_3D('',#55867,#33451,#33452);
#27033=AXIS2_PLACEMENT_3D('',#55871,#33455,#33456);
#27034=AXIS2_PLACEMENT_3D('',#55875,#33459,#33460);
#27035=AXIS2_PLACEMENT_3D('',#55879,#33462,#33463);
#27036=AXIS2_PLACEMENT_3D('',#55881,#33465,#33466);
#27037=AXIS2_PLACEMENT_3D('',#55885,#33468,#33469);
#27038=AXIS2_PLACEMENT_3D('',#55887,#33471,#33472);
#27039=AXIS2_PLACEMENT_3D('',#55889,#33474,#33475);
#27040=AXIS2_PLACEMENT_3D('',#55893,#33478,#33479);
#27041=AXIS2_PLACEMENT_3D('',#55895,#33481,#33482);
#27042=AXIS2_PLACEMENT_3D('',#55898,#33483,#33484);
#27043=AXIS2_PLACEMENT_3D('',#55901,#33487,#33488);
#27044=AXIS2_PLACEMENT_3D('',#55904,#33489,#33490);
#27045=AXIS2_PLACEMENT_3D('',#55907,#33493,#33494);
#27046=AXIS2_PLACEMENT_3D('',#55908,#33495,#33496);
#27047=AXIS2_PLACEMENT_3D('',#55909,#33497,#33498);
#27048=AXIS2_PLACEMENT_3D('',#55912,#33499,#33500);
#27049=AXIS2_PLACEMENT_3D('',#55915,#33503,#33504);
#27050=AXIS2_PLACEMENT_3D('',#55918,#33505,#33506);
#27051=AXIS2_PLACEMENT_3D('',#55921,#33509,#33510);
#27052=AXIS2_PLACEMENT_3D('',#55923,#33512,#33513);
#27053=AXIS2_PLACEMENT_3D('',#55925,#33515,#33516);
#27054=AXIS2_PLACEMENT_3D('',#55928,#33517,#33518);
#27055=AXIS2_PLACEMENT_3D('',#55931,#33521,#33522);
#27056=AXIS2_PLACEMENT_3D('',#55934,#33523,#33524);
#27057=AXIS2_PLACEMENT_3D('',#55937,#33527,#33528);
#27058=AXIS2_PLACEMENT_3D('',#55938,#33529,#33530);
#27059=AXIS2_PLACEMENT_3D('',#55939,#33531,#33532);
#27060=AXIS2_PLACEMENT_3D('',#55945,#33536,#33537);
#27061=AXIS2_PLACEMENT_3D('',#55947,#33539,#33540);
#27062=AXIS2_PLACEMENT_3D('',#55950,#33541,#33542);
#27063=AXIS2_PLACEMENT_3D('',#55953,#33545,#33546);
#27064=AXIS2_PLACEMENT_3D('',#55956,#33547,#33548);
#27065=AXIS2_PLACEMENT_3D('',#55959,#33551,#33552);
#27066=AXIS2_PLACEMENT_3D('',#55960,#33553,#33554);
#27067=AXIS2_PLACEMENT_3D('',#55961,#33555,#33556);
#27068=AXIS2_PLACEMENT_3D('',#55964,#33557,#33558);
#27069=AXIS2_PLACEMENT_3D('',#55967,#33561,#33562);
#27070=AXIS2_PLACEMENT_3D('',#55970,#33563,#33564);
#27071=AXIS2_PLACEMENT_3D('',#55973,#33567,#33568);
#27072=AXIS2_PLACEMENT_3D('',#55975,#33570,#33571);
#27073=AXIS2_PLACEMENT_3D('',#55977,#33573,#33574);
#27074=AXIS2_PLACEMENT_3D('',#55979,#33576,#33577);
#27075=AXIS2_PLACEMENT_3D('',#55982,#33578,#33579);
#27076=AXIS2_PLACEMENT_3D('',#55985,#33582,#33583);
#27077=AXIS2_PLACEMENT_3D('',#55988,#33584,#33585);
#27078=AXIS2_PLACEMENT_3D('',#55991,#33588,#33589);
#27079=AXIS2_PLACEMENT_3D('',#55992,#33590,#33591);
#27080=AXIS2_PLACEMENT_3D('',#55993,#33592,#33593);
#27081=AXIS2_PLACEMENT_3D('',#55997,#33595,#33596);
#27082=AXIS2_PLACEMENT_3D('',#55999,#33598,#33599);
#27083=AXIS2_PLACEMENT_3D('',#56003,#33601,#33602);
#27084=AXIS2_PLACEMENT_3D('',#56005,#33604,#33605);
#27085=AXIS2_PLACEMENT_3D('',#56011,#33609,#33610);
#27086=AXIS2_PLACEMENT_3D('',#56015,#33613,#33614);
#27087=AXIS2_PLACEMENT_3D('',#56019,#33617,#33618);
#27088=AXIS2_PLACEMENT_3D('',#56021,#33620,#33621);
#27089=AXIS2_PLACEMENT_3D('',#56025,#33624,#33625);
#27090=AXIS2_PLACEMENT_3D('',#56027,#33627,#33628);
#27091=AXIS2_PLACEMENT_3D('',#56029,#33630,#33631);
#27092=AXIS2_PLACEMENT_3D('',#56031,#33633,#33634);
#27093=AXIS2_PLACEMENT_3D('',#56033,#33636,#33637);
#27094=AXIS2_PLACEMENT_3D('',#56035,#33639,#33640);
#27095=AXIS2_PLACEMENT_3D('',#56037,#33642,#33643);
#27096=AXIS2_PLACEMENT_3D('',#56041,#33646,#33647);
#27097=AXIS2_PLACEMENT_3D('',#56043,#33649,#33650);
#27098=AXIS2_PLACEMENT_3D('',#56044,#33651,#33652);
#27099=AXIS2_PLACEMENT_3D('',#56048,#33655,#33656);
#27100=AXIS2_PLACEMENT_3D('',#56050,#33657,#33658);
#27101=AXIS2_PLACEMENT_3D('',#56052,#33660,#33661);
#27102=AXIS2_PLACEMENT_3D('',#56054,#33663,#33664);
#27103=AXIS2_PLACEMENT_3D('',#56055,#33665,#33666);
#27104=AXIS2_PLACEMENT_3D('',#56056,#33667,#33668);
#27105=AXIS2_PLACEMENT_3D('',#56057,#33669,#33670);
#27106=AXIS2_PLACEMENT_3D('',#56058,#33671,#33672);
#27107=AXIS2_PLACEMENT_3D('',#56059,#33673,#33674);
#27108=AXIS2_PLACEMENT_3D('',#56060,#33675,#33676);
#27109=AXIS2_PLACEMENT_3D('',#56062,#33677,#33678);
#27110=AXIS2_PLACEMENT_3D('',#56064,#33679,#33680);
#27111=AXIS2_PLACEMENT_3D('',#56065,#33681,#33682);
#27112=AXIS2_PLACEMENT_3D('',#56094,#33683,#33684);
#27113=AXIS2_PLACEMENT_3D('',#56095,#33685,#33686);
#27114=AXIS2_PLACEMENT_3D('',#56096,#33687,#33688);
#27115=AXIS2_PLACEMENT_3D('',#56099,#33690,#33691);
#27116=AXIS2_PLACEMENT_3D('',#56100,#33692,#33693);
#27117=AXIS2_PLACEMENT_3D('',#56102,#33694,#33695);
#27118=AXIS2_PLACEMENT_3D('',#56103,#33696,#33697);
#27119=AXIS2_PLACEMENT_3D('',#56106,#33698,#33699);
#27120=AXIS2_PLACEMENT_3D('',#56114,#33700,#33701);
#27121=AXIS2_PLACEMENT_3D('',#56117,#33702,#33703);
#27122=AXIS2_PLACEMENT_3D('',#56125,#33704,#33705);
#27123=AXIS2_PLACEMENT_3D('',#56128,#33706,#33707);
#27124=AXIS2_PLACEMENT_3D('',#56142,#33709,#33710);
#27125=AXIS2_PLACEMENT_3D('',#56153,#33711,#33712);
#27126=AXIS2_PLACEMENT_3D('',#56155,#33713,#33714);
#27127=AXIS2_PLACEMENT_3D('',#56157,#33715,#33716);
#27128=AXIS2_PLACEMENT_3D('',#56158,#33717,#33718);
#27129=AXIS2_PLACEMENT_3D('',#56162,#33720,#33721);
#27130=AXIS2_PLACEMENT_3D('',#56164,#33722,#33723);
#27131=AXIS2_PLACEMENT_3D('',#56166,#33724,#33725);
#27132=AXIS2_PLACEMENT_3D('',#56168,#33726,#33727);
#27133=AXIS2_PLACEMENT_3D('',#56170,#33728,#33729);
#27134=AXIS2_PLACEMENT_3D('',#56171,#33730,#33731);
#27135=AXIS2_PLACEMENT_3D('',#56172,#33732,#33733);
#27136=AXIS2_PLACEMENT_3D('',#56174,#33734,#33735);
#27137=AXIS2_PLACEMENT_3D('',#56175,#33736,#33737);
#27138=AXIS2_PLACEMENT_3D('',#56177,#33738,#33739);
#27139=AXIS2_PLACEMENT_3D('',#56179,#33740,#33741);
#27140=AXIS2_PLACEMENT_3D('',#56181,#33742,#33743);
#27141=AXIS2_PLACEMENT_3D('',#56183,#33744,#33745);
#27142=AXIS2_PLACEMENT_3D('',#56184,#33746,#33747);
#27143=AXIS2_PLACEMENT_3D('',#56185,#33748,#33749);
#27144=AXIS2_PLACEMENT_3D('',#56187,#33750,#33751);
#27145=AXIS2_PLACEMENT_3D('',#56189,#33752,#33753);
#27146=AXIS2_PLACEMENT_3D('',#56191,#33754,#33755);
#27147=AXIS2_PLACEMENT_3D('',#56193,#33756,#33757);
#27148=AXIS2_PLACEMENT_3D('',#56194,#33758,#33759);
#27149=AXIS2_PLACEMENT_3D('',#56195,#33760,#33761);
#27150=AXIS2_PLACEMENT_3D('',#56199,#33764,#33765);
#27151=AXIS2_PLACEMENT_3D('',#56203,#33768,#33769);
#27152=AXIS2_PLACEMENT_3D('',#56207,#33772,#33773);
#27153=AXIS2_PLACEMENT_3D('',#56211,#33776,#33777);
#27154=AXIS2_PLACEMENT_3D('',#56215,#33780,#33781);
#27155=AXIS2_PLACEMENT_3D('',#56219,#33784,#33785);
#27156=AXIS2_PLACEMENT_3D('',#56225,#33789,#33790);
#27157=AXIS2_PLACEMENT_3D('',#56229,#33793,#33794);
#27158=AXIS2_PLACEMENT_3D('',#56233,#33797,#33798);
#27159=AXIS2_PLACEMENT_3D('',#56237,#33801,#33802);
#27160=AXIS2_PLACEMENT_3D('',#56241,#33805,#33806);
#27161=AXIS2_PLACEMENT_3D('',#56243,#33808,#33809);
#27162=AXIS2_PLACEMENT_3D('',#56244,#33810,#33811);
#27163=AXIS2_PLACEMENT_3D('',#56252,#33812,#33813);
#27164=AXIS2_PLACEMENT_3D('',#56260,#33814,#33815);
#27165=AXIS2_PLACEMENT_3D('',#56268,#33816,#33817);
#27166=AXIS2_PLACEMENT_3D('',#56276,#33818,#33819);
#27167=AXIS2_PLACEMENT_3D('',#56284,#33820,#33821);
#27168=AXIS2_PLACEMENT_3D('',#56292,#33822,#33823);
#27169=AXIS2_PLACEMENT_3D('',#56300,#33824,#33825);
#27170=AXIS2_PLACEMENT_3D('',#56308,#33826,#33827);
#27171=AXIS2_PLACEMENT_3D('',#56316,#33828,#33829);
#27172=AXIS2_PLACEMENT_3D('',#56324,#33830,#33831);
#27173=AXIS2_PLACEMENT_3D('',#56327,#33834,#33835);
#27174=AXIS2_PLACEMENT_3D('',#56329,#33837,#33838);
#27175=AXIS2_PLACEMENT_3D('',#56331,#33840,#33841);
#27176=AXIS2_PLACEMENT_3D('',#56333,#33843,#33844);
#27177=AXIS2_PLACEMENT_3D('',#56335,#33846,#33847);
#27178=AXIS2_PLACEMENT_3D('',#56336,#33848,#33849);
#27179=AXIS2_PLACEMENT_3D('',#56337,#33850,#33851);
#27180=AXIS2_PLACEMENT_3D('',#56338,#33852,#33853);
#27181=AXIS2_PLACEMENT_3D('',#56339,#33854,#33855);
#27182=AXIS2_PLACEMENT_3D('',#56340,#33856,#33857);
#27183=AXIS2_PLACEMENT_3D('',#56341,#33858,#33859);
#27184=AXIS2_PLACEMENT_3D('',#56342,#33860,#33861);
#27185=AXIS2_PLACEMENT_3D('',#56343,#33862,#33863);
#27186=AXIS2_PLACEMENT_3D('',#56344,#33864,#33865);
#27187=AXIS2_PLACEMENT_3D('',#56345,#33866,#33867);
#27188=AXIS2_PLACEMENT_3D('',#56346,#33868,#33869);
#27189=AXIS2_PLACEMENT_3D('',#56347,#33870,#33871);
#27190=AXIS2_PLACEMENT_3D('',#56348,#33872,#33873);
#27191=AXIS2_PLACEMENT_3D('',#56350,#33874,#33875);
#27192=AXIS2_PLACEMENT_3D('',#56353,#33877,#33878);
#27193=AXIS2_PLACEMENT_3D('',#56354,#33879,#33880);
#27194=AXIS2_PLACEMENT_3D('',#56357,#33882,#33883);
#27195=AXIS2_PLACEMENT_3D('',#56359,#33884,#33885);
#27196=AXIS2_PLACEMENT_3D('',#56362,#33887,#33888);
#27197=AXIS2_PLACEMENT_3D('',#56363,#33889,#33890);
#27198=AXIS2_PLACEMENT_3D('',#56366,#33892,#33893);
#27199=AXIS2_PLACEMENT_3D('',#56368,#33894,#33895);
#27200=AXIS2_PLACEMENT_3D('',#56371,#33897,#33898);
#27201=AXIS2_PLACEMENT_3D('',#56372,#33899,#33900);
#27202=AXIS2_PLACEMENT_3D('',#56375,#33902,#33903);
#27203=AXIS2_PLACEMENT_3D('',#56377,#33904,#33905);
#27204=AXIS2_PLACEMENT_3D('',#56380,#33907,#33908);
#27205=AXIS2_PLACEMENT_3D('',#56381,#33909,#33910);
#27206=AXIS2_PLACEMENT_3D('',#56384,#33912,#33913);
#27207=AXIS2_PLACEMENT_3D('',#56386,#33914,#33915);
#27208=AXIS2_PLACEMENT_3D('',#56389,#33917,#33918);
#27209=AXIS2_PLACEMENT_3D('',#56390,#33919,#33920);
#27210=AXIS2_PLACEMENT_3D('',#56393,#33922,#33923);
#27211=AXIS2_PLACEMENT_3D('',#56395,#33924,#33925);
#27212=AXIS2_PLACEMENT_3D('',#56398,#33927,#33928);
#27213=AXIS2_PLACEMENT_3D('',#56399,#33929,#33930);
#27214=AXIS2_PLACEMENT_3D('',#56402,#33932,#33933);
#27215=AXIS2_PLACEMENT_3D('',#56404,#33934,#33935);
#27216=AXIS2_PLACEMENT_3D('',#56407,#33937,#33938);
#27217=AXIS2_PLACEMENT_3D('',#56408,#33939,#33940);
#27218=AXIS2_PLACEMENT_3D('',#56411,#33942,#33943);
#27219=AXIS2_PLACEMENT_3D('',#56413,#33944,#33945);
#27220=AXIS2_PLACEMENT_3D('',#56416,#33947,#33948);
#27221=AXIS2_PLACEMENT_3D('',#56417,#33949,#33950);
#27222=AXIS2_PLACEMENT_3D('',#56420,#33952,#33953);
#27223=AXIS2_PLACEMENT_3D('',#56429,#33958,#33959);
#27224=AXIS2_PLACEMENT_3D('',#56433,#33961,#33962);
#27225=AXIS2_PLACEMENT_3D('',#56437,#33964,#33965);
#27226=AXIS2_PLACEMENT_3D('',#56447,#33971,#33972);
#27227=AXIS2_PLACEMENT_3D('',#56453,#33976,#33977);
#27228=AXIS2_PLACEMENT_3D('',#56458,#33979,#33980);
#27229=AXIS2_PLACEMENT_3D('',#56462,#33982,#33983);
#27230=AXIS2_PLACEMENT_3D('',#56468,#33988,#33989);
#27231=AXIS2_PLACEMENT_3D('',#56471,#33992,#33993);
#27232=AXIS2_PLACEMENT_3D('',#56472,#33994,#33995);
#27233=AXIS2_PLACEMENT_3D('',#56473,#33996,#33997);
#27234=AXIS2_PLACEMENT_3D('',#56475,#33999,#34000);
#27235=AXIS2_PLACEMENT_3D('',#56478,#34003,#34004);
#27236=AXIS2_PLACEMENT_3D('',#56480,#34006,#34007);
#27237=AXIS2_PLACEMENT_3D('',#56481,#34008,#34009);
#27238=AXIS2_PLACEMENT_3D('',#56482,#34010,#34011);
#27239=AXIS2_PLACEMENT_3D('',#56483,#34012,#34013);
#27240=AXIS2_PLACEMENT_3D('',#56486,#34014,#34015);
#27241=AXIS2_PLACEMENT_3D('',#56487,#34016,#34017);
#27242=AXIS2_PLACEMENT_3D('',#56490,#34019,#34020);
#27243=AXIS2_PLACEMENT_3D('',#56491,#34021,#34022);
#27244=AXIS2_PLACEMENT_3D('',#56496,#34024,#34025);
#27245=AXIS2_PLACEMENT_3D('',#56498,#34026,#34027);
#27246=AXIS2_PLACEMENT_3D('',#56500,#34028,#34029);
#27247=AXIS2_PLACEMENT_3D('',#56502,#34030,#34031);
#27248=AXIS2_PLACEMENT_3D('',#56504,#34032,#34033);
#27249=AXIS2_PLACEMENT_3D('',#56506,#34034,#34035);
#27250=AXIS2_PLACEMENT_3D('',#56507,#34036,#34037);
#27251=AXIS2_PLACEMENT_3D('',#56508,#34038,#34039);
#27252=AXIS2_PLACEMENT_3D('',#56511,#34041,#34042);
#27253=AXIS2_PLACEMENT_3D('',#56512,#34043,#34044);
#27254=AXIS2_PLACEMENT_3D('',#56514,#34045,#34046);
#27255=AXIS2_PLACEMENT_3D('',#56517,#34048,#34049);
#27256=AXIS2_PLACEMENT_3D('',#56518,#34050,#34051);
#27257=AXIS2_PLACEMENT_3D('',#56520,#34052,#34053);
#27258=AXIS2_PLACEMENT_3D('',#56523,#34055,#34056);
#27259=AXIS2_PLACEMENT_3D('',#56524,#34057,#34058);
#27260=AXIS2_PLACEMENT_3D('',#56537,#34065,#34066);
#27261=AXIS2_PLACEMENT_3D('',#56538,#34067,#34068);
#27262=AXIS2_PLACEMENT_3D('',#56539,#34069,#34070);
#27263=AXIS2_PLACEMENT_3D('',#56540,#34071,#34072);
#27264=AXIS2_PLACEMENT_3D('',#56547,#34077,#34078);
#27265=AXIS2_PLACEMENT_3D('',#56552,#34082,#34083);
#27266=AXIS2_PLACEMENT_3D('',#56557,#34087,#34088);
#27267=AXIS2_PLACEMENT_3D('',#56562,#34092,#34093);
#27268=AXIS2_PLACEMENT_3D('',#56567,#34097,#34098);
#27269=AXIS2_PLACEMENT_3D('',#56570,#34101,#34102);
#27270=AXIS2_PLACEMENT_3D('',#56571,#34103,#34104);
#27271=AXIS2_PLACEMENT_3D('',#56572,#34105,#34106);
#27272=AXIS2_PLACEMENT_3D('',#56573,#34107,#34108);
#27273=AXIS2_PLACEMENT_3D('',#56574,#34109,#34110);
#27274=AXIS2_PLACEMENT_3D('',#56575,#34111,#34112);
#27275=AXIS2_PLACEMENT_3D('',#56576,#34113,#34114);
#27276=AXIS2_PLACEMENT_3D('',#56578,#34115,#34116);
#27277=AXIS2_PLACEMENT_3D('',#56581,#34118,#34119);
#27278=AXIS2_PLACEMENT_3D('',#56582,#34120,#34121);
#27279=AXIS2_PLACEMENT_3D('',#56584,#34122,#34123);
#27280=AXIS2_PLACEMENT_3D('',#56587,#34125,#34126);
#27281=AXIS2_PLACEMENT_3D('',#56588,#34127,#34128);
#27282=AXIS2_PLACEMENT_3D('',#56589,#34129,#34130);
#27283=AXIS2_PLACEMENT_3D('',#56590,#34131,#34132);
#27284=AXIS2_PLACEMENT_3D('',#56593,#34133,#34134);
#27285=AXIS2_PLACEMENT_3D('',#56597,#34136,#34137);
#27286=AXIS2_PLACEMENT_3D('',#56599,#34139,#34140);
#27287=AXIS2_PLACEMENT_3D('',#56602,#34141,#34142);
#27288=AXIS2_PLACEMENT_3D('',#56606,#34144,#34145);
#27289=AXIS2_PLACEMENT_3D('',#56608,#34147,#34148);
#27290=AXIS2_PLACEMENT_3D('',#56611,#34151,#34152);
#27291=AXIS2_PLACEMENT_3D('',#56614,#34155,#34156);
#27292=AXIS2_PLACEMENT_3D('',#56615,#34157,#34158);
#27293=AXIS2_PLACEMENT_3D('',#56616,#34159,#34160);
#27294=AXIS2_PLACEMENT_3D('',#56617,#34161,#34162);
#27295=AXIS2_PLACEMENT_3D('',#56619,#34163,#34164);
#27296=AXIS2_PLACEMENT_3D('',#56622,#34166,#34167);
#27297=AXIS2_PLACEMENT_3D('',#56623,#34168,#34169);
#27298=AXIS2_PLACEMENT_3D('',#56626,#34171,#34172);
#27299=AXIS2_PLACEMENT_3D('',#56627,#34173,#34174);
#27300=AXIS2_PLACEMENT_3D('',#56630,#34175,#34176);
#27301=AXIS2_PLACEMENT_3D('',#56633,#34178,#34179);
#27302=AXIS2_PLACEMENT_3D('',#56634,#34180,#34181);
#27303=AXIS2_PLACEMENT_3D('',#56635,#34182,#34183);
#27304=AXIS2_PLACEMENT_3D('',#56638,#34185,#34186);
#27305=AXIS2_PLACEMENT_3D('',#56639,#34187,#34188);
#27306=AXIS2_PLACEMENT_3D('',#56640,#34189,#34190);
#27307=AXIS2_PLACEMENT_3D('',#56653,#34197,#34198);
#27308=AXIS2_PLACEMENT_3D('',#56654,#34199,#34200);
#27309=AXIS2_PLACEMENT_3D('',#56660,#34204,#34205);
#27310=AXIS2_PLACEMENT_3D('',#56664,#34208,#34209);
#27311=AXIS2_PLACEMENT_3D('',#56668,#34212,#34213);
#27312=AXIS2_PLACEMENT_3D('',#56672,#34216,#34217);
#27313=AXIS2_PLACEMENT_3D('',#56676,#34220,#34221);
#27314=AXIS2_PLACEMENT_3D('',#56678,#34223,#34224);
#27315=AXIS2_PLACEMENT_3D('',#56679,#34225,#34226);
#27316=AXIS2_PLACEMENT_3D('',#56680,#34227,#34228);
#27317=AXIS2_PLACEMENT_3D('',#56683,#34229,#34230);
#27318=AXIS2_PLACEMENT_3D('',#56684,#34231,#34232);
#27319=AXIS2_PLACEMENT_3D('',#56687,#34234,#34235);
#27320=AXIS2_PLACEMENT_3D('',#56688,#34236,#34237);
#27321=AXIS2_PLACEMENT_3D('',#56693,#34239,#34240);
#27322=AXIS2_PLACEMENT_3D('',#56695,#34241,#34242);
#27323=AXIS2_PLACEMENT_3D('',#56697,#34243,#34244);
#27324=AXIS2_PLACEMENT_3D('',#56699,#34245,#34246);
#27325=AXIS2_PLACEMENT_3D('',#56701,#34247,#34248);
#27326=AXIS2_PLACEMENT_3D('',#56703,#34249,#34250);
#27327=AXIS2_PLACEMENT_3D('',#56704,#34251,#34252);
#27328=AXIS2_PLACEMENT_3D('',#56705,#34253,#34254);
#27329=AXIS2_PLACEMENT_3D('',#56708,#34256,#34257);
#27330=AXIS2_PLACEMENT_3D('',#56709,#34258,#34259);
#27331=AXIS2_PLACEMENT_3D('',#56711,#34260,#34261);
#27332=AXIS2_PLACEMENT_3D('',#56714,#34263,#34264);
#27333=AXIS2_PLACEMENT_3D('',#56715,#34265,#34266);
#27334=AXIS2_PLACEMENT_3D('',#56717,#34267,#34268);
#27335=AXIS2_PLACEMENT_3D('',#56720,#34270,#34271);
#27336=AXIS2_PLACEMENT_3D('',#56721,#34272,#34273);
#27337=AXIS2_PLACEMENT_3D('',#56734,#34280,#34281);
#27338=AXIS2_PLACEMENT_3D('',#56735,#34282,#34283);
#27339=AXIS2_PLACEMENT_3D('',#56736,#34284,#34285);
#27340=AXIS2_PLACEMENT_3D('',#56737,#34286,#34287);
#27341=AXIS2_PLACEMENT_3D('',#56744,#34292,#34293);
#27342=AXIS2_PLACEMENT_3D('',#56749,#34297,#34298);
#27343=AXIS2_PLACEMENT_3D('',#56754,#34302,#34303);
#27344=AXIS2_PLACEMENT_3D('',#56759,#34307,#34308);
#27345=AXIS2_PLACEMENT_3D('',#56764,#34312,#34313);
#27346=AXIS2_PLACEMENT_3D('',#56767,#34316,#34317);
#27347=AXIS2_PLACEMENT_3D('',#56768,#34318,#34319);
#27348=AXIS2_PLACEMENT_3D('',#56769,#34320,#34321);
#27349=AXIS2_PLACEMENT_3D('',#56770,#34322,#34323);
#27350=AXIS2_PLACEMENT_3D('',#56771,#34324,#34325);
#27351=AXIS2_PLACEMENT_3D('',#56772,#34326,#34327);
#27352=AXIS2_PLACEMENT_3D('',#56773,#34328,#34329);
#27353=AXIS2_PLACEMENT_3D('',#56775,#34330,#34331);
#27354=AXIS2_PLACEMENT_3D('',#56778,#34333,#34334);
#27355=AXIS2_PLACEMENT_3D('',#56779,#34335,#34336);
#27356=AXIS2_PLACEMENT_3D('',#56781,#34337,#34338);
#27357=AXIS2_PLACEMENT_3D('',#56784,#34340,#34341);
#27358=AXIS2_PLACEMENT_3D('',#56785,#34342,#34343);
#27359=AXIS2_PLACEMENT_3D('',#56786,#34344,#34345);
#27360=AXIS2_PLACEMENT_3D('',#56787,#34346,#34347);
#27361=AXIS2_PLACEMENT_3D('',#56790,#34348,#34349);
#27362=AXIS2_PLACEMENT_3D('',#56794,#34351,#34352);
#27363=AXIS2_PLACEMENT_3D('',#56796,#34354,#34355);
#27364=AXIS2_PLACEMENT_3D('',#56799,#34356,#34357);
#27365=AXIS2_PLACEMENT_3D('',#56803,#34359,#34360);
#27366=AXIS2_PLACEMENT_3D('',#56805,#34362,#34363);
#27367=AXIS2_PLACEMENT_3D('',#56808,#34366,#34367);
#27368=AXIS2_PLACEMENT_3D('',#56811,#34370,#34371);
#27369=AXIS2_PLACEMENT_3D('',#56812,#34372,#34373);
#27370=AXIS2_PLACEMENT_3D('',#56813,#34374,#34375);
#27371=AXIS2_PLACEMENT_3D('',#56814,#34376,#34377);
#27372=AXIS2_PLACEMENT_3D('',#56816,#34378,#34379);
#27373=AXIS2_PLACEMENT_3D('',#56819,#34381,#34382);
#27374=AXIS2_PLACEMENT_3D('',#56820,#34383,#34384);
#27375=AXIS2_PLACEMENT_3D('',#56823,#34386,#34387);
#27376=AXIS2_PLACEMENT_3D('',#56824,#34388,#34389);
#27377=AXIS2_PLACEMENT_3D('',#56827,#34390,#34391);
#27378=AXIS2_PLACEMENT_3D('',#56830,#34393,#34394);
#27379=AXIS2_PLACEMENT_3D('',#56831,#34395,#34396);
#27380=AXIS2_PLACEMENT_3D('',#56832,#34397,#34398);
#27381=AXIS2_PLACEMENT_3D('',#56835,#34400,#34401);
#27382=AXIS2_PLACEMENT_3D('',#56836,#34402,#34403);
#27383=AXIS2_PLACEMENT_3D('',#56837,#34404,#34405);
#27384=AXIS2_PLACEMENT_3D('',#56850,#34412,#34413);
#27385=AXIS2_PLACEMENT_3D('',#56851,#34414,#34415);
#27386=AXIS2_PLACEMENT_3D('',#56857,#34419,#34420);
#27387=AXIS2_PLACEMENT_3D('',#56861,#34423,#34424);
#27388=AXIS2_PLACEMENT_3D('',#56865,#34427,#34428);
#27389=AXIS2_PLACEMENT_3D('',#56869,#34431,#34432);
#27390=AXIS2_PLACEMENT_3D('',#56873,#34435,#34436);
#27391=AXIS2_PLACEMENT_3D('',#56875,#34438,#34439);
#27392=AXIS2_PLACEMENT_3D('',#56876,#34440,#34441);
#27393=AXIS2_PLACEMENT_3D('',#56877,#34442,#34443);
#27394=AXIS2_PLACEMENT_3D('',#56879,#34444,#34445);
#27395=AXIS2_PLACEMENT_3D('',#56882,#34447,#34448);
#27396=AXIS2_PLACEMENT_3D('',#56883,#34449,#34450);
#27397=AXIS2_PLACEMENT_3D('',#56886,#34452,#34453);
#27398=AXIS2_PLACEMENT_3D('',#56887,#34454,#34455);
#27399=AXIS2_PLACEMENT_3D('',#56890,#34456,#34457);
#27400=AXIS2_PLACEMENT_3D('',#56893,#34459,#34460);
#27401=AXIS2_PLACEMENT_3D('',#56894,#34461,#34462);
#27402=AXIS2_PLACEMENT_3D('',#56895,#34463,#34464);
#27403=AXIS2_PLACEMENT_3D('',#56898,#34466,#34467);
#27404=AXIS2_PLACEMENT_3D('',#56899,#34468,#34469);
#27405=AXIS2_PLACEMENT_3D('',#56900,#34470,#34471);
#27406=AXIS2_PLACEMENT_3D('',#56913,#34478,#34479);
#27407=AXIS2_PLACEMENT_3D('',#56914,#34480,#34481);
#27408=AXIS2_PLACEMENT_3D('',#56920,#34485,#34486);
#27409=AXIS2_PLACEMENT_3D('',#56924,#34489,#34490);
#27410=AXIS2_PLACEMENT_3D('',#56928,#34493,#34494);
#27411=AXIS2_PLACEMENT_3D('',#56932,#34497,#34498);
#27412=AXIS2_PLACEMENT_3D('',#56936,#34501,#34502);
#27413=AXIS2_PLACEMENT_3D('',#56938,#34504,#34505);
#27414=AXIS2_PLACEMENT_3D('',#56939,#34506,#34507);
#27415=AXIS2_PLACEMENT_3D('',#56940,#34508,#34509);
#27416=AXIS2_PLACEMENT_3D('',#56941,#34510,#34511);
#27417=AXIS2_PLACEMENT_3D('',#56942,#34512,#34513);
#27418=AXIS2_PLACEMENT_3D('',#56943,#34514,#34515);
#27419=AXIS2_PLACEMENT_3D('',#56944,#34516,#34517);
#27420=AXIS2_PLACEMENT_3D('',#56945,#34518,#34519);
#27421=AXIS2_PLACEMENT_3D('',#56946,#34520,#34521);
#27422=AXIS2_PLACEMENT_3D('',#56947,#34522,#34523);
#27423=AXIS2_PLACEMENT_3D('',#56948,#34524,#34525);
#27424=AXIS2_PLACEMENT_3D('',#56949,#34526,#34527);
#27425=AXIS2_PLACEMENT_3D('',#56950,#34528,#34529);
#27426=AXIS2_PLACEMENT_3D('',#56951,#34530,#34531);
#27427=AXIS2_PLACEMENT_3D('',#56952,#34532,#34533);
#27428=AXIS2_PLACEMENT_3D('',#56953,#34534,#34535);
#27429=AXIS2_PLACEMENT_3D('',#56954,#34536,#34537);
#27430=AXIS2_PLACEMENT_3D('',#56955,#34538,#34539);
#27431=AXIS2_PLACEMENT_3D('',#56956,#34540,#34541);
#27432=AXIS2_PLACEMENT_3D('',#56957,#34542,#34543);
#27433=AXIS2_PLACEMENT_3D('',#56958,#34544,#34545);
#27434=AXIS2_PLACEMENT_3D('',#56959,#34546,#34547);
#27435=AXIS2_PLACEMENT_3D('',#56960,#34548,#34549);
#27436=AXIS2_PLACEMENT_3D('',#56961,#34550,#34551);
#27437=AXIS2_PLACEMENT_3D('',#56962,#34552,#34553);
#27438=AXIS2_PLACEMENT_3D('',#56963,#34554,#34555);
#27439=AXIS2_PLACEMENT_3D('',#56964,#34556,#34557);
#27440=AXIS2_PLACEMENT_3D('',#56965,#34558,#34559);
#27441=AXIS2_PLACEMENT_3D('',#56966,#34560,#34561);
#27442=AXIS2_PLACEMENT_3D('',#56967,#34562,#34563);
#27443=AXIS2_PLACEMENT_3D('',#56968,#34564,#34565);
#27444=AXIS2_PLACEMENT_3D('',#56969,#34566,#34567);
#27445=AXIS2_PLACEMENT_3D('',#56970,#34568,#34569);
#27446=AXIS2_PLACEMENT_3D('',#56971,#34570,#34571);
#27447=AXIS2_PLACEMENT_3D('',#56972,#34572,#34573);
#27448=AXIS2_PLACEMENT_3D('',#56973,#34574,#34575);
#27449=AXIS2_PLACEMENT_3D('',#56974,#34576,#34577);
#27450=AXIS2_PLACEMENT_3D('',#56975,#34578,#34579);
#27451=AXIS2_PLACEMENT_3D('',#56976,#34580,#34581);
#27452=AXIS2_PLACEMENT_3D('',#56977,#34582,#34583);
#27453=AXIS2_PLACEMENT_3D('',#56978,#34584,#34585);
#27454=AXIS2_PLACEMENT_3D('',#56979,#34586,#34587);
#27455=AXIS2_PLACEMENT_3D('',#56980,#34588,#34589);
#27456=AXIS2_PLACEMENT_3D('',#56981,#34590,#34591);
#27457=AXIS2_PLACEMENT_3D('',#56982,#34592,#34593);
#27458=AXIS2_PLACEMENT_3D('',#56983,#34594,#34595);
#27459=AXIS2_PLACEMENT_3D('',#56984,#34596,#34597);
#27460=AXIS2_PLACEMENT_3D('',#56985,#34598,#34599);
#27461=AXIS2_PLACEMENT_3D('',#56986,#34600,#34601);
#27462=AXIS2_PLACEMENT_3D('',#56987,#34602,#34603);
#27463=AXIS2_PLACEMENT_3D('',#56988,#34604,#34605);
#27464=AXIS2_PLACEMENT_3D('',#56989,#34606,#34607);
#27465=AXIS2_PLACEMENT_3D('',#56990,#34608,#34609);
#27466=AXIS2_PLACEMENT_3D('',#56991,#34610,#34611);
#27467=AXIS2_PLACEMENT_3D('',#56992,#34612,#34613);
#27468=AXIS2_PLACEMENT_3D('',#56993,#34614,#34615);
#27469=AXIS2_PLACEMENT_3D('',#56994,#34616,#34617);
#27470=AXIS2_PLACEMENT_3D('',#56995,#34618,#34619);
#27471=AXIS2_PLACEMENT_3D('',#56996,#34620,#34621);
#27472=AXIS2_PLACEMENT_3D('',#56997,#34622,#34623);
#27473=AXIS2_PLACEMENT_3D('',#56998,#34624,#34625);
#27474=AXIS2_PLACEMENT_3D('',#56999,#34626,#34627);
#27475=AXIS2_PLACEMENT_3D('',#57000,#34628,#34629);
#27476=AXIS2_PLACEMENT_3D('',#57001,#34630,#34631);
#27477=DIRECTION('axis',(0.,0.,1.));
#27478=DIRECTION('refdir',(1.,0.,0.));
#27479=DIRECTION('axis',(0.,0.,1.));
#27480=DIRECTION('refdir',(1.,0.,0.));
#27481=DIRECTION('center_axis',(0.,0.,1.));
#27482=DIRECTION('ref_axis',(1.,0.,0.));
#27483=DIRECTION('center_axis',(0.,0.,1.));
#27484=DIRECTION('ref_axis',(1.,0.,0.));
#27485=DIRECTION('',(0.,0.,1.));
#27486=DIRECTION('center_axis',(0.,0.,1.));
#27487=DIRECTION('ref_axis',(1.,0.,0.));
#27488=DIRECTION('center_axis',(0.,0.,1.));
#27489=DIRECTION('ref_axis',(1.,0.,0.));
#27490=DIRECTION('center_axis',(0.,0.,1.));
#27491=DIRECTION('ref_axis',(1.,0.,0.));
#27492=DIRECTION('',(0.,0.,1.));
#27493=DIRECTION('center_axis',(0.,0.,1.));
#27494=DIRECTION('ref_axis',(1.,0.,0.));
#27495=DIRECTION('center_axis',(0.,0.,1.));
#27496=DIRECTION('ref_axis',(1.,0.,0.));
#27497=DIRECTION('center_axis',(0.,0.,1.));
#27498=DIRECTION('ref_axis',(1.,0.,0.));
#27499=DIRECTION('',(0.,0.,1.));
#27500=DIRECTION('center_axis',(0.,0.,1.));
#27501=DIRECTION('ref_axis',(1.,0.,0.));
#27502=DIRECTION('center_axis',(0.,0.,1.));
#27503=DIRECTION('ref_axis',(1.,0.,0.));
#27504=DIRECTION('center_axis',(0.,0.,1.));
#27505=DIRECTION('ref_axis',(1.,0.,0.));
#27506=DIRECTION('',(0.,0.,1.));
#27507=DIRECTION('center_axis',(0.,0.,1.));
#27508=DIRECTION('ref_axis',(1.,0.,0.));
#27509=DIRECTION('center_axis',(0.,0.,1.));
#27510=DIRECTION('ref_axis',(1.,0.,0.));
#27511=DIRECTION('center_axis',(0.,0.,1.));
#27512=DIRECTION('ref_axis',(1.,0.,0.));
#27513=DIRECTION('',(0.,0.,1.));
#27514=DIRECTION('center_axis',(0.,0.,1.));
#27515=DIRECTION('ref_axis',(1.,0.,0.));
#27516=DIRECTION('center_axis',(0.,0.,1.));
#27517=DIRECTION('ref_axis',(1.,0.,0.));
#27518=DIRECTION('center_axis',(0.,0.,1.));
#27519=DIRECTION('ref_axis',(1.,0.,0.));
#27520=DIRECTION('',(0.,0.,1.));
#27521=DIRECTION('center_axis',(0.,0.,1.));
#27522=DIRECTION('ref_axis',(1.,0.,0.));
#27523=DIRECTION('center_axis',(0.,0.,1.));
#27524=DIRECTION('ref_axis',(1.,0.,0.));
#27525=DIRECTION('center_axis',(0.,0.,1.));
#27526=DIRECTION('ref_axis',(1.,0.,0.));
#27527=DIRECTION('',(0.,0.,1.));
#27528=DIRECTION('center_axis',(0.,0.,1.));
#27529=DIRECTION('ref_axis',(1.,0.,0.));
#27530=DIRECTION('center_axis',(0.,0.,1.));
#27531=DIRECTION('ref_axis',(1.,0.,0.));
#27532=DIRECTION('center_axis',(0.,0.,1.));
#27533=DIRECTION('ref_axis',(1.,0.,0.));
#27534=DIRECTION('',(0.,0.,1.));
#27535=DIRECTION('center_axis',(0.,0.,1.));
#27536=DIRECTION('ref_axis',(1.,0.,0.));
#27537=DIRECTION('center_axis',(0.,1.,0.));
#27538=DIRECTION('ref_axis',(0.,0.,1.));
#27539=DIRECTION('center_axis',(0.,1.,0.));
#27540=DIRECTION('ref_axis',(0.,0.,1.));
#27541=DIRECTION('',(0.,1.,0.));
#27542=DIRECTION('center_axis',(0.,1.,0.));
#27543=DIRECTION('ref_axis',(0.,0.,1.));
#27544=DIRECTION('center_axis',(0.,1.,0.));
#27545=DIRECTION('ref_axis',(0.,0.,1.));
#27546=DIRECTION('',(-1.04972719113862E-16,0.515038074910055,-0.857167300702112));
#27547=DIRECTION('center_axis',(0.,1.,0.));
#27548=DIRECTION('ref_axis',(0.,0.,1.));
#27549=DIRECTION('center_axis',(0.,1.,0.));
#27550=DIRECTION('ref_axis',(0.,0.,1.));
#27551=DIRECTION('',(0.,1.,0.));
#27552=DIRECTION('center_axis',(0.,1.,0.));
#27553=DIRECTION('ref_axis',(0.,0.,1.));
#27554=DIRECTION('center_axis',(0.,1.,0.));
#27555=DIRECTION('ref_axis',(0.,0.,1.));
#27556=DIRECTION('',(-1.04972719113862E-16,0.515038074910055,-0.857167300702112));
#27557=DIRECTION('center_axis',(0.,1.,0.));
#27558=DIRECTION('ref_axis',(0.,0.,1.));
#27559=DIRECTION('center_axis',(0.,1.,0.));
#27560=DIRECTION('ref_axis',(0.,0.,1.));
#27561=DIRECTION('',(0.,1.,0.));
#27562=DIRECTION('center_axis',(0.,1.,0.));
#27563=DIRECTION('ref_axis',(0.,0.,1.));
#27564=DIRECTION('center_axis',(0.,1.,0.));
#27565=DIRECTION('ref_axis',(0.,0.,1.));
#27566=DIRECTION('',(-1.04972719113862E-16,0.515038074910053,-0.857167300702113));
#27567=DIRECTION('center_axis',(0.,1.,0.));
#27568=DIRECTION('ref_axis',(0.,0.,1.));
#27569=DIRECTION('center_axis',(0.,1.,0.));
#27570=DIRECTION('ref_axis',(0.,0.,1.));
#27571=DIRECTION('',(0.,1.,0.));
#27572=DIRECTION('center_axis',(0.,1.,0.));
#27573=DIRECTION('ref_axis',(0.,0.,1.));
#27574=DIRECTION('center_axis',(0.,1.,0.));
#27575=DIRECTION('ref_axis',(0.,0.,1.));
#27576=DIRECTION('',(-1.04972719113862E-16,0.515038074910053,-0.857167300702113));
#27577=DIRECTION('center_axis',(0.,1.,0.));
#27578=DIRECTION('ref_axis',(0.,0.,1.));
#27579=DIRECTION('',(1.,0.,0.));
#27580=DIRECTION('',(0.,0.,1.));
#27581=DIRECTION('',(1.,0.,0.));
#27582=DIRECTION('',(0.,0.,-1.));
#27583=DIRECTION('center_axis',(-1.,0.,0.));
#27584=DIRECTION('ref_axis',(0.,0.,1.));
#27585=DIRECTION('',(0.,1.,0.));
#27586=DIRECTION('',(0.,0.,-1.));
#27587=DIRECTION('',(0.,1.,0.));
#27588=DIRECTION('',(0.,0.,-1.));
#27589=DIRECTION('center_axis',(0.,-1.,0.));
#27590=DIRECTION('ref_axis',(0.,0.,-1.));
#27591=DIRECTION('',(-1.,0.,0.));
#27592=DIRECTION('',(0.,0.,-1.));
#27593=DIRECTION('',(-1.,0.,0.));
#27594=DIRECTION('center_axis',(1.,0.,0.));
#27595=DIRECTION('ref_axis',(0.,0.,-1.));
#27596=DIRECTION('',(0.,-1.,0.));
#27597=DIRECTION('',(0.,-1.,0.));
#27598=DIRECTION('center_axis',(0.,1.,0.));
#27599=DIRECTION('ref_axis',(0.,0.,1.));
#27600=DIRECTION('',(1.,0.,0.));
#27601=DIRECTION('',(0.,0.,1.));
#27602=DIRECTION('',(1.,0.,0.));
#27603=DIRECTION('center_axis',(0.,0.,-1.));
#27604=DIRECTION('ref_axis',(-1.,0.,0.));
#27605=DIRECTION('',(0.,-1.,0.));
#27606=DIRECTION('',(-1.,0.,0.));
#27607=DIRECTION('',(0.,1.,0.));
#27608=DIRECTION('center_axis',(0.,0.,-1.));
#27609=DIRECTION('ref_axis',(-1.,0.,0.));
#27610=DIRECTION('',(0.,-1.,0.));
#27611=DIRECTION('',(0.,1.,0.));
#27612=DIRECTION('',(-1.,0.,0.));
#27613=DIRECTION('center_axis',(-1.,0.,0.));
#27614=DIRECTION('ref_axis',(0.,0.,1.));
#27615=DIRECTION('',(0.,0.,1.));
#27616=DIRECTION('center_axis',(0.,1.,0.));
#27617=DIRECTION('ref_axis',(0.,0.,1.));
#27618=DIRECTION('',(0.,0.,1.));
#27619=DIRECTION('center_axis',(1.,0.,0.));
#27620=DIRECTION('ref_axis',(0.,0.,-1.));
#27621=DIRECTION('axis',(0.,0.,1.));
#27622=DIRECTION('refdir',(1.,0.,0.));
#27623=DIRECTION('axis',(0.,0.,1.));
#27624=DIRECTION('refdir',(1.,0.,0.));
#27625=DIRECTION('axis',(0.,0.,1.));
#27626=DIRECTION('refdir',(1.,0.,0.));
#27627=DIRECTION('center_axis',(-1.,0.,0.));
#27628=DIRECTION('ref_axis',(0.,0.,1.));
#27629=DIRECTION('center_axis',(-1.,0.,0.));
#27630=DIRECTION('ref_axis',(0.,0.,1.));
#27631=DIRECTION('',(1.,0.,0.));
#27632=DIRECTION('center_axis',(-1.,0.,0.));
#27633=DIRECTION('ref_axis',(0.,0.,1.));
#27634=DIRECTION('',(-1.,0.,0.));
#27635=DIRECTION('',(1.,0.,0.));
#27636=DIRECTION('center_axis',(-1.,0.,0.));
#27637=DIRECTION('ref_axis',(0.,0.,1.));
#27638=DIRECTION('center_axis',(-1.,0.,0.));
#27639=DIRECTION('ref_axis',(0.,0.,1.));
#27640=DIRECTION('center_axis',(-1.,0.,0.));
#27641=DIRECTION('ref_axis',(0.,0.,1.));
#27642=DIRECTION('center_axis',(0.,1.,-1.22464679914735E-16));
#27643=DIRECTION('ref_axis',(0.,-1.22464679914735E-16,-1.));
#27644=DIRECTION('center_axis',(-1.,0.,0.));
#27645=DIRECTION('ref_axis',(0.,0.,1.));
#27646=DIRECTION('center_axis',(-1.,0.,0.));
#27647=DIRECTION('ref_axis',(0.,0.,1.));
#27648=DIRECTION('',(0.707106781186492,8.65956056235561E-17,0.707106781186603));
#27649=DIRECTION('center_axis',(-1.,0.,0.));
#27650=DIRECTION('ref_axis',(0.,0.,1.));
#27651=DIRECTION('center_axis',(-1.,0.,0.));
#27652=DIRECTION('ref_axis',(0.,0.,1.));
#27653=DIRECTION('center_axis',(-1.,0.,0.));
#27654=DIRECTION('ref_axis',(0.,0.,1.));
#27655=DIRECTION('',(1.,0.,0.));
#27656=DIRECTION('center_axis',(-1.,0.,0.));
#27657=DIRECTION('ref_axis',(0.,0.,1.));
#27658=DIRECTION('center_axis',(-1.,0.,0.));
#27659=DIRECTION('ref_axis',(0.,0.,1.));
#27660=DIRECTION('center_axis',(0.,1.,-1.22464679914735E-16));
#27661=DIRECTION('ref_axis',(0.,-1.22464679914735E-16,-1.));
#27662=DIRECTION('center_axis',(-1.,0.,0.));
#27663=DIRECTION('ref_axis',(0.,0.,1.));
#27664=DIRECTION('center_axis',(-1.,0.,0.));
#27665=DIRECTION('ref_axis',(0.,0.,1.));
#27666=DIRECTION('',(0.707106781186486,8.65956056235568E-17,0.707106781186609));
#27667=DIRECTION('center_axis',(-1.,0.,0.));
#27668=DIRECTION('ref_axis',(0.,0.,1.));
#27669=DIRECTION('center_axis',(-1.,0.,0.));
#27670=DIRECTION('ref_axis',(0.,0.,1.));
#27671=DIRECTION('center_axis',(-1.,0.,0.));
#27672=DIRECTION('ref_axis',(0.,0.,1.));
#27673=DIRECTION('center_axis',(-1.,0.,0.));
#27674=DIRECTION('ref_axis',(0.,0.,1.));
#27675=DIRECTION('',(1.,0.,0.));
#27676=DIRECTION('center_axis',(1.,0.,0.));
#27677=DIRECTION('ref_axis',(0.,0.,-1.));
#27678=DIRECTION('',(-0.707106781186569,8.65956056235467E-17,-0.707106781186526));
#27679=DIRECTION('center_axis',(-1.,0.,0.));
#27680=DIRECTION('ref_axis',(0.,0.,1.));
#27681=DIRECTION('center_axis',(-1.,0.,0.));
#27682=DIRECTION('ref_axis',(0.,0.,1.));
#27683=DIRECTION('center_axis',(-1.,0.,0.));
#27684=DIRECTION('ref_axis',(0.,0.,1.));
#27685=DIRECTION('center_axis',(0.,1.,-1.22464679914735E-16));
#27686=DIRECTION('ref_axis',(0.,-1.22464679914735E-16,-1.));
#27687=DIRECTION('center_axis',(-1.,0.,0.));
#27688=DIRECTION('ref_axis',(0.,0.,1.));
#27689=DIRECTION('center_axis',(-1.,0.,0.));
#27690=DIRECTION('ref_axis',(0.,0.,1.));
#27691=DIRECTION('center_axis',(-1.,0.,0.));
#27692=DIRECTION('ref_axis',(0.,0.,1.));
#27693=DIRECTION('',(1.,0.,0.));
#27694=DIRECTION('center_axis',(-1.,0.,0.));
#27695=DIRECTION('ref_axis',(0.,0.,1.));
#27696=DIRECTION('center_axis',(-1.,0.,0.));
#27697=DIRECTION('ref_axis',(0.,0.,1.));
#27698=DIRECTION('',(1.,0.,0.));
#27699=DIRECTION('center_axis',(-1.,0.,0.));
#27700=DIRECTION('ref_axis',(0.,0.,1.));
#27701=DIRECTION('center_axis',(-1.,0.,0.));
#27702=DIRECTION('ref_axis',(0.,0.,1.));
#27703=DIRECTION('center_axis',(-1.,0.,0.));
#27704=DIRECTION('ref_axis',(0.,0.,1.));
#27705=DIRECTION('center_axis',(-1.,0.,0.));
#27706=DIRECTION('ref_axis',(0.,0.,1.));
#27707=DIRECTION('',(1.,0.,0.));
#27708=DIRECTION('center_axis',(-1.,0.,0.));
#27709=DIRECTION('ref_axis',(0.,0.,1.));
#27710=DIRECTION('center_axis',(1.,0.,0.));
#27711=DIRECTION('ref_axis',(0.,0.,-1.));
#27712=DIRECTION('',(-0.70710678118657,8.65956056235465E-17,-0.707106781186525));
#27713=DIRECTION('center_axis',(-1.,0.,0.));
#27714=DIRECTION('ref_axis',(0.,0.,1.));
#27715=DIRECTION('center_axis',(-1.,0.,0.));
#27716=DIRECTION('ref_axis',(0.,0.,1.));
#27717=DIRECTION('center_axis',(1.,0.,0.));
#27718=DIRECTION('ref_axis',(0.,0.,-1.));
#27719=DIRECTION('center_axis',(1.,0.,0.));
#27720=DIRECTION('ref_axis',(0.,0.,-1.));
#27721=DIRECTION('center_axis',(-1.,0.,0.));
#27722=DIRECTION('ref_axis',(0.,0.,1.));
#27723=DIRECTION('center_axis',(-1.,0.,0.));
#27724=DIRECTION('ref_axis',(0.,0.,1.));
#27725=DIRECTION('center_axis',(-1.,0.,0.));
#27726=DIRECTION('ref_axis',(0.,5.66553889764798E-16,-1.));
#27727=DIRECTION('center_axis',(-1.,0.,0.));
#27728=DIRECTION('ref_axis',(0.,0.,1.));
#27729=DIRECTION('center_axis',(-1.,0.,0.));
#27730=DIRECTION('ref_axis',(0.,0.,1.));
#27731=DIRECTION('',(0.,0.,1.));
#27732=DIRECTION('',(0.,1.,1.44560289664734E-16));
#27733=DIRECTION('',(0.,-2.4093381610789E-16,1.));
#27734=DIRECTION('center_axis',(1.,0.,0.));
#27735=DIRECTION('ref_axis',(0.,0.,-1.));
#27736=DIRECTION('center_axis',(0.,1.,0.));
#27737=DIRECTION('ref_axis',(0.,0.,1.));
#27738=DIRECTION('',(0.,0.,-1.));
#27739=DIRECTION('',(1.,0.,0.));
#27740=DIRECTION('center_axis',(0.,-1.,-2.4093381610789E-16));
#27741=DIRECTION('ref_axis',(0.,2.4093381610789E-16,-1.));
#27742=DIRECTION('',(1.,0.,0.));
#27743=DIRECTION('',(0.,-2.4093381610789E-16,1.));
#27744=DIRECTION('center_axis',(0.,1.44560289664734E-16,-1.));
#27745=DIRECTION('ref_axis',(0.,1.,1.44560289664734E-16));
#27746=DIRECTION('center_axis',(0.,-1.44560289664734E-16,1.));
#27747=DIRECTION('ref_axis',(0.,1.,1.44560289664734E-16));
#27748=DIRECTION('center_axis',(0.,0.,1.));
#27749=DIRECTION('ref_axis',(-1.,1.22464679914735E-16,0.));
#27750=DIRECTION('axis',(0.,0.,1.));
#27751=DIRECTION('refdir',(1.,0.,0.));
#27752=DIRECTION('center_axis',(0.,0.923879532511287,0.382683432365091));
#27753=DIRECTION('ref_axis',(0.,-0.382683432365091,0.923879532511286));
#27754=DIRECTION('',(0.,0.923879532511286,0.382683432365091));
#27755=DIRECTION('center_axis',(1.,0.,0.));
#27756=DIRECTION('ref_axis',(0.,0.,-1.));
#27757=DIRECTION('center_axis',(1.,0.,0.));
#27758=DIRECTION('ref_axis',(0.,0.,-1.));
#27759=DIRECTION('',(1.,0.,0.));
#27760=DIRECTION('center_axis',(1.,0.,0.));
#27761=DIRECTION('ref_axis',(0.,0.,-1.));
#27762=DIRECTION('center_axis',(1.,0.,0.));
#27763=DIRECTION('ref_axis',(0.,0.,-1.));
#27764=DIRECTION('center_axis',(1.,0.,0.));
#27765=DIRECTION('ref_axis',(0.,0.,-1.));
#27766=DIRECTION('',(1.,0.,0.));
#27767=DIRECTION('center_axis',(1.,0.,0.));
#27768=DIRECTION('ref_axis',(0.,0.,-1.));
#27769=DIRECTION('center_axis',(1.,0.,0.));
#27770=DIRECTION('ref_axis',(0.,0.,-1.));
#27771=DIRECTION('center_axis',(1.,0.,0.));
#27772=DIRECTION('ref_axis',(0.,0.,-1.));
#27773=DIRECTION('',(1.,0.,0.));
#27774=DIRECTION('center_axis',(1.,0.,0.));
#27775=DIRECTION('ref_axis',(0.,0.,-1.));
#27776=DIRECTION('center_axis',(1.,0.,0.));
#27777=DIRECTION('ref_axis',(0.,0.,-1.));
#27778=DIRECTION('center_axis',(1.,0.,0.));
#27779=DIRECTION('ref_axis',(0.,0.,-1.));
#27780=DIRECTION('',(1.,0.,0.));
#27781=DIRECTION('center_axis',(1.,0.,0.));
#27782=DIRECTION('ref_axis',(0.,0.,-1.));
#27783=DIRECTION('center_axis',(1.,0.,0.));
#27784=DIRECTION('ref_axis',(0.,0.,-1.));
#27785=DIRECTION('center_axis',(1.,0.,0.));
#27786=DIRECTION('ref_axis',(0.,0.,-1.));
#27787=DIRECTION('',(1.,0.,0.));
#27788=DIRECTION('center_axis',(1.,0.,0.));
#27789=DIRECTION('ref_axis',(0.,0.,-1.));
#27790=DIRECTION('center_axis',(1.,0.,0.));
#27791=DIRECTION('ref_axis',(0.,0.,-1.));
#27792=DIRECTION('center_axis',(1.,0.,0.));
#27793=DIRECTION('ref_axis',(0.,0.,-1.));
#27794=DIRECTION('',(1.,0.,0.));
#27795=DIRECTION('center_axis',(1.,0.,0.));
#27796=DIRECTION('ref_axis',(0.,0.,-1.));
#27797=DIRECTION('center_axis',(-1.,0.,0.));
#27798=DIRECTION('ref_axis',(0.,0.,1.));
#27799=DIRECTION('center_axis',(-1.,0.,0.));
#27800=DIRECTION('ref_axis',(0.,0.,1.));
#27801=DIRECTION('',(1.,0.,0.));
#27802=DIRECTION('center_axis',(-1.,0.,0.));
#27803=DIRECTION('ref_axis',(0.,0.,1.));
#27804=DIRECTION('center_axis',(-1.,0.,0.));
#27805=DIRECTION('ref_axis',(0.,0.,1.));
#27806=DIRECTION('center_axis',(-1.,0.,0.));
#27807=DIRECTION('ref_axis',(0.,0.,1.));
#27808=DIRECTION('',(-1.,0.,0.));
#27809=DIRECTION('center_axis',(-1.,0.,0.));
#27810=DIRECTION('ref_axis',(0.,0.,1.));
#27811=DIRECTION('center_axis',(-1.,0.,0.));
#27812=DIRECTION('ref_axis',(0.,0.,1.));
#27813=DIRECTION('center_axis',(-1.,0.,0.));
#27814=DIRECTION('ref_axis',(0.,0.,1.));
#27815=DIRECTION('',(1.,0.,0.));
#27816=DIRECTION('center_axis',(-1.,0.,0.));
#27817=DIRECTION('ref_axis',(0.,0.,1.));
#27818=DIRECTION('center_axis',(-1.,0.,0.));
#27819=DIRECTION('ref_axis',(0.,0.,1.));
#27820=DIRECTION('center_axis',(-1.,0.,0.));
#27821=DIRECTION('ref_axis',(0.,0.,1.));
#27822=DIRECTION('',(-1.,0.,0.));
#27823=DIRECTION('center_axis',(-1.,0.,0.));
#27824=DIRECTION('ref_axis',(0.,0.,1.));
#27825=DIRECTION('center_axis',(-1.,0.,0.));
#27826=DIRECTION('ref_axis',(0.,0.,1.));
#27827=DIRECTION('center_axis',(-1.,0.,0.));
#27828=DIRECTION('ref_axis',(0.,0.,1.));
#27829=DIRECTION('',(1.,0.,0.));
#27830=DIRECTION('center_axis',(-1.,0.,0.));
#27831=DIRECTION('ref_axis',(0.,0.,1.));
#27832=DIRECTION('center_axis',(-1.,0.,0.));
#27833=DIRECTION('ref_axis',(0.,0.,1.));
#27834=DIRECTION('center_axis',(-1.,0.,0.));
#27835=DIRECTION('ref_axis',(0.,0.,1.));
#27836=DIRECTION('',(-1.,0.,0.));
#27837=DIRECTION('center_axis',(-1.,0.,0.));
#27838=DIRECTION('ref_axis',(0.,0.,1.));
#27839=DIRECTION('center_axis',(-1.,0.,0.));
#27840=DIRECTION('ref_axis',(0.,0.,1.));
#27841=DIRECTION('center_axis',(-1.,0.,0.));
#27842=DIRECTION('ref_axis',(0.,0.,1.));
#27843=DIRECTION('center_axis',(0.,-1.,1.22464679914735E-16));
#27844=DIRECTION('ref_axis',(0.,-1.22464679914735E-16,-1.));
#27845=DIRECTION('center_axis',(-1.,0.,0.));
#27846=DIRECTION('ref_axis',(0.,0.,1.));
#27847=DIRECTION('',(0.,-1.,1.44560289664734E-16));
#27848=DIRECTION('center_axis',(-1.,0.,0.));
#27849=DIRECTION('ref_axis',(0.,0.,1.));
#27850=DIRECTION('',(0.,1.,1.44560289664734E-16));
#27851=DIRECTION('center_axis',(-1.,0.,0.));
#27852=DIRECTION('ref_axis',(0.,0.,1.));
#27853=DIRECTION('center_axis',(-1.,0.,0.));
#27854=DIRECTION('ref_axis',(0.,0.,1.));
#27855=DIRECTION('center_axis',(-1.,0.,0.));
#27856=DIRECTION('ref_axis',(0.,0.,1.));
#27857=DIRECTION('center_axis',(-1.,0.,0.));
#27858=DIRECTION('ref_axis',(0.,0.,1.));
#27859=DIRECTION('center_axis',(-1.,0.,0.));
#27860=DIRECTION('ref_axis',(0.,0.,1.));
#27861=DIRECTION('center_axis',(-1.,0.,0.));
#27862=DIRECTION('ref_axis',(0.,0.,1.));
#27863=DIRECTION('',(1.,0.,0.));
#27864=DIRECTION('center_axis',(-1.,0.,0.));
#27865=DIRECTION('ref_axis',(0.,0.,1.));
#27866=DIRECTION('',(-1.,0.,0.));
#27867=DIRECTION('center_axis',(-1.,0.,0.));
#27868=DIRECTION('ref_axis',(0.,0.,1.));
#27869=DIRECTION('',(-1.,0.,0.));
#27870=DIRECTION('',(1.,0.,0.));
#27871=DIRECTION('center_axis',(-1.,0.,0.));
#27872=DIRECTION('ref_axis',(0.,0.,1.));
#27873=DIRECTION('center_axis',(-1.,0.,0.));
#27874=DIRECTION('ref_axis',(0.,0.,1.));
#27875=DIRECTION('center_axis',(-1.,0.,0.));
#27876=DIRECTION('ref_axis',(0.,0.,1.));
#27877=DIRECTION('center_axis',(-1.,0.,0.));
#27878=DIRECTION('ref_axis',(0.,0.,1.));
#27879=DIRECTION('center_axis',(-1.,0.,0.));
#27880=DIRECTION('ref_axis',(0.,0.,1.));
#27881=DIRECTION('center_axis',(1.,0.,0.));
#27882=DIRECTION('ref_axis',(0.,0.,-1.));
#27883=DIRECTION('',(0.,-1.,1.44560289664734E-16));
#27884=DIRECTION('',(0.,1.,1.44560289664734E-16));
#27885=DIRECTION('center_axis',(1.,0.,0.));
#27886=DIRECTION('ref_axis',(0.,0.,-1.));
#27887=DIRECTION('center_axis',(1.,0.,0.));
#27888=DIRECTION('ref_axis',(0.,0.,-1.));
#27889=DIRECTION('center_axis',(1.,0.,0.));
#27890=DIRECTION('ref_axis',(0.,0.,-1.));
#27891=DIRECTION('center_axis',(-1.,0.,0.));
#27892=DIRECTION('ref_axis',(0.,0.,1.));
#27893=DIRECTION('center_axis',(-1.,0.,0.));
#27894=DIRECTION('ref_axis',(0.,0.,1.));
#27895=DIRECTION('center_axis',(0.,1.44560289664734E-16,-1.));
#27896=DIRECTION('ref_axis',(0.,1.,1.44560289664734E-16));
#27897=DIRECTION('center_axis',(0.,1.44560289664734E-16,1.));
#27898=DIRECTION('ref_axis',(0.,-1.,1.44560289664734E-16));
#27899=DIRECTION('',(0.,3.78946479905599E-31,1.));
#27900=DIRECTION('',(1.,1.23259516440783E-32,-4.67087598701011E-63));
#27901=DIRECTION('',(0.,3.78946479905599E-31,1.));
#27902=DIRECTION('',(1.,1.23259516440783E-32,-4.67087598701011E-63));
#27903=DIRECTION('axis',(0.,0.,1.));
#27904=DIRECTION('refdir',(1.,0.,0.));
#27905=DIRECTION('axis',(0.,0.,1.));
#27906=DIRECTION('refdir',(1.,0.,0.));
#27907=DIRECTION('center_axis',(0.,1.,3.01691039300315E-16));
#27908=DIRECTION('ref_axis',(0.,-3.01691039300315E-16,1.));
#27909=DIRECTION('center_axis',(0.,1.,3.01691039300315E-16));
#27910=DIRECTION('ref_axis',(0.,-3.01691039300315E-16,1.));
#27911=DIRECTION('',(0.,1.,3.01691039300315E-16));
#27912=DIRECTION('center_axis',(0.,1.,3.01691039300315E-16));
#27913=DIRECTION('ref_axis',(0.,-3.01691039300315E-16,1.));
#27914=DIRECTION('center_axis',(0.,1.,3.01691039300315E-16));
#27915=DIRECTION('ref_axis',(0.,-3.01691039300315E-16,1.));
#27916=DIRECTION('center_axis',(0.,1.,3.01691039300315E-16));
#27917=DIRECTION('ref_axis',(0.,-3.01691039300315E-16,1.));
#27918=DIRECTION('',(0.,1.,3.01691039300315E-16));
#27919=DIRECTION('center_axis',(0.,1.,3.01691039300315E-16));
#27920=DIRECTION('ref_axis',(0.,-3.01691039300315E-16,1.));
#27921=DIRECTION('center_axis',(1.,0.,0.));
#27922=DIRECTION('ref_axis',(0.,0.,-1.));
#27923=DIRECTION('center_axis',(1.,0.,0.));
#27924=DIRECTION('ref_axis',(0.,0.,-1.));
#27925=DIRECTION('',(1.,0.,0.));
#27926=DIRECTION('center_axis',(1.,0.,0.));
#27927=DIRECTION('ref_axis',(0.,0.,-1.));
#27928=DIRECTION('center_axis',(1.,0.,0.));
#27929=DIRECTION('ref_axis',(0.,0.,-1.));
#27930=DIRECTION('center_axis',(1.,0.,0.));
#27931=DIRECTION('ref_axis',(0.,0.,-1.));
#27932=DIRECTION('',(1.,0.,0.));
#27933=DIRECTION('center_axis',(1.,0.,0.));
#27934=DIRECTION('ref_axis',(0.,0.,-1.));
#27935=DIRECTION('center_axis',(1.,0.,0.));
#27936=DIRECTION('ref_axis',(0.,0.,-1.));
#27937=DIRECTION('center_axis',(1.,0.,0.));
#27938=DIRECTION('ref_axis',(0.,0.,-1.));
#27939=DIRECTION('',(1.,0.,0.));
#27940=DIRECTION('center_axis',(1.,0.,0.));
#27941=DIRECTION('ref_axis',(0.,0.,-1.));
#27942=DIRECTION('center_axis',(1.,0.,0.));
#27943=DIRECTION('ref_axis',(0.,0.,-1.));
#27944=DIRECTION('center_axis',(1.,0.,0.));
#27945=DIRECTION('ref_axis',(0.,0.,-1.));
#27946=DIRECTION('',(1.,0.,0.));
#27947=DIRECTION('center_axis',(1.,0.,0.));
#27948=DIRECTION('ref_axis',(0.,0.,-1.));
#27949=DIRECTION('center_axis',(1.,0.,0.));
#27950=DIRECTION('ref_axis',(0.,0.,-1.));
#27951=DIRECTION('center_axis',(1.,0.,0.));
#27952=DIRECTION('ref_axis',(0.,0.,-1.));
#27953=DIRECTION('',(1.,0.,0.));
#27954=DIRECTION('center_axis',(1.,0.,0.));
#27955=DIRECTION('ref_axis',(0.,0.,-1.));
#27956=DIRECTION('center_axis',(1.,0.,0.));
#27957=DIRECTION('ref_axis',(0.,0.,-1.));
#27958=DIRECTION('',(0.515038074910055,-1.04972719113862E-16,0.857167300702111));
#27959=DIRECTION('center_axis',(1.,0.,0.));
#27960=DIRECTION('ref_axis',(0.,0.,-1.));
#27961=DIRECTION('center_axis',(1.,0.,0.));
#27962=DIRECTION('ref_axis',(0.,0.,-1.));
#27963=DIRECTION('center_axis',(1.,0.,0.));
#27964=DIRECTION('ref_axis',(0.,0.,-1.));
#27965=DIRECTION('center_axis',(1.,0.,0.));
#27966=DIRECTION('ref_axis',(0.,0.,-1.));
#27967=DIRECTION('center_axis',(1.,0.,0.));
#27968=DIRECTION('ref_axis',(0.,0.,-1.));
#27969=DIRECTION('center_axis',(1.,0.,0.));
#27970=DIRECTION('ref_axis',(0.,0.,-1.));
#27971=DIRECTION('center_axis',(1.,0.,0.));
#27972=DIRECTION('ref_axis',(0.,0.,-1.));
#27973=DIRECTION('',(0.515038074910055,-1.04972719113862E-16,0.857167300702111));
#27974=DIRECTION('center_axis',(1.,0.,0.));
#27975=DIRECTION('ref_axis',(0.,0.,-1.));
#27976=DIRECTION('center_axis',(1.,0.,0.));
#27977=DIRECTION('ref_axis',(0.,0.,-1.));
#27978=DIRECTION('center_axis',(1.,0.,0.));
#27979=DIRECTION('ref_axis',(0.,0.,-1.));
#27980=DIRECTION('center_axis',(1.,0.,0.));
#27981=DIRECTION('ref_axis',(0.,0.,-1.));
#27982=DIRECTION('center_axis',(1.,0.,0.));
#27983=DIRECTION('ref_axis',(0.,0.,-1.));
#27984=DIRECTION('center_axis',(1.,0.,0.));
#27985=DIRECTION('ref_axis',(0.,0.,-1.));
#27986=DIRECTION('center_axis',(1.,0.,0.));
#27987=DIRECTION('ref_axis',(0.,0.,-1.));
#27988=DIRECTION('',(0.515038074910055,-1.04972719113862E-16,0.857167300702112));
#27989=DIRECTION('center_axis',(1.,0.,0.));
#27990=DIRECTION('ref_axis',(0.,0.,-1.));
#27991=DIRECTION('center_axis',(1.,0.,0.));
#27992=DIRECTION('ref_axis',(0.,0.,-1.));
#27993=DIRECTION('center_axis',(1.,0.,0.));
#27994=DIRECTION('ref_axis',(0.,0.,-1.));
#27995=DIRECTION('center_axis',(1.,0.,0.));
#27996=DIRECTION('ref_axis',(0.,0.,-1.));
#27997=DIRECTION('center_axis',(1.,0.,0.));
#27998=DIRECTION('ref_axis',(0.,0.,-1.));
#27999=DIRECTION('center_axis',(1.,0.,0.));
#28000=DIRECTION('ref_axis',(0.,0.,-1.));
#28001=DIRECTION('center_axis',(1.,0.,0.));
#28002=DIRECTION('ref_axis',(0.,0.,-1.));
#28003=DIRECTION('',(0.515038074910055,-1.04972719113862E-16,0.857167300702112));
#28004=DIRECTION('center_axis',(1.,0.,0.));
#28005=DIRECTION('ref_axis',(0.,0.,-1.));
#28006=DIRECTION('center_axis',(1.,0.,0.));
#28007=DIRECTION('ref_axis',(0.,0.,-1.));
#28008=DIRECTION('center_axis',(1.,0.,0.));
#28009=DIRECTION('ref_axis',(0.,0.,-1.));
#28010=DIRECTION('center_axis',(1.,0.,0.));
#28011=DIRECTION('ref_axis',(0.,0.,-1.));
#28012=DIRECTION('center_axis',(1.,0.,0.));
#28013=DIRECTION('ref_axis',(0.,0.,-1.));
#28014=DIRECTION('center_axis',(1.,0.,0.));
#28015=DIRECTION('ref_axis',(0.,0.,-1.));
#28016=DIRECTION('center_axis',(-1.,0.,0.));
#28017=DIRECTION('ref_axis',(0.,0.,1.));
#28018=DIRECTION('center_axis',(1.,0.,0.));
#28019=DIRECTION('ref_axis',(0.,0.,-1.));
#28020=DIRECTION('',(1.,0.,0.));
#28021=DIRECTION('center_axis',(1.,0.,0.));
#28022=DIRECTION('ref_axis',(0.,0.,-1.));
#28023=DIRECTION('center_axis',(-1.,0.,0.));
#28024=DIRECTION('ref_axis',(0.,0.,1.));
#28025=DIRECTION('center_axis',(1.,0.,0.));
#28026=DIRECTION('ref_axis',(0.,0.,-1.));
#28027=DIRECTION('',(1.,0.,0.));
#28028=DIRECTION('center_axis',(1.,0.,0.));
#28029=DIRECTION('ref_axis',(0.,0.,-1.));
#28030=DIRECTION('center_axis',(-1.,0.,0.));
#28031=DIRECTION('ref_axis',(0.,0.,1.));
#28032=DIRECTION('center_axis',(1.,0.,0.));
#28033=DIRECTION('ref_axis',(0.,0.,-1.));
#28034=DIRECTION('',(1.,0.,0.));
#28035=DIRECTION('center_axis',(1.,0.,0.));
#28036=DIRECTION('ref_axis',(0.,0.,-1.));
#28037=DIRECTION('center_axis',(-1.,0.,0.));
#28038=DIRECTION('ref_axis',(0.,0.,1.));
#28039=DIRECTION('center_axis',(1.,0.,0.));
#28040=DIRECTION('ref_axis',(0.,0.,-1.));
#28041=DIRECTION('',(1.,0.,0.));
#28042=DIRECTION('center_axis',(1.,0.,0.));
#28043=DIRECTION('ref_axis',(0.,0.,-1.));
#28044=DIRECTION('center_axis',(-1.,0.,0.));
#28045=DIRECTION('ref_axis',(0.,0.,1.));
#28046=DIRECTION('center_axis',(1.,0.,0.));
#28047=DIRECTION('ref_axis',(0.,0.,-1.));
#28048=DIRECTION('',(-1.,0.,0.));
#28049=DIRECTION('center_axis',(-1.,0.,0.));
#28050=DIRECTION('ref_axis',(0.,0.,-1.));
#28051=DIRECTION('center_axis',(-1.,0.,0.));
#28052=DIRECTION('ref_axis',(0.,0.,1.));
#28053=DIRECTION('center_axis',(1.,0.,0.));
#28054=DIRECTION('ref_axis',(0.,0.,-1.));
#28055=DIRECTION('',(-1.,0.,0.));
#28056=DIRECTION('center_axis',(-1.,0.,0.));
#28057=DIRECTION('ref_axis',(0.,0.,-1.));
#28058=DIRECTION('center_axis',(-1.,0.,0.));
#28059=DIRECTION('ref_axis',(0.,0.,1.));
#28060=DIRECTION('center_axis',(1.,0.,0.));
#28061=DIRECTION('ref_axis',(0.,0.,-1.));
#28062=DIRECTION('',(-1.,0.,0.));
#28063=DIRECTION('center_axis',(-1.,0.,0.));
#28064=DIRECTION('ref_axis',(0.,0.,-1.));
#28065=DIRECTION('center_axis',(-1.,0.,0.));
#28066=DIRECTION('ref_axis',(0.,0.,1.));
#28067=DIRECTION('center_axis',(1.,0.,0.));
#28068=DIRECTION('ref_axis',(0.,0.,-1.));
#28069=DIRECTION('',(-1.,0.,0.));
#28070=DIRECTION('center_axis',(-1.,0.,0.));
#28071=DIRECTION('ref_axis',(0.,0.,-1.));
#28072=DIRECTION('center_axis',(1.,0.,0.));
#28073=DIRECTION('ref_axis',(0.,0.,-1.));
#28074=DIRECTION('center_axis',(1.,0.,0.));
#28075=DIRECTION('ref_axis',(0.,0.,-1.));
#28076=DIRECTION('center_axis',(1.,0.,0.));
#28077=DIRECTION('ref_axis',(0.,0.,-1.));
#28078=DIRECTION('center_axis',(1.,0.,0.));
#28079=DIRECTION('ref_axis',(0.,0.,-1.));
#28080=DIRECTION('center_axis',(1.,0.,0.));
#28081=DIRECTION('ref_axis',(0.,0.,-1.));
#28082=DIRECTION('',(0.,-2.10269512239613E-16,1.));
#28083=DIRECTION('',(0.,-0.707106781186582,0.707106781186513));
#28084=DIRECTION('',(0.,-1.,-2.95272081017329E-16));
#28085=DIRECTION('',(0.,2.55331806268467E-16,-1.));
#28086=DIRECTION('',(0.,1.,5.90544162034659E-16));
#28087=DIRECTION('',(0.,0.707106781186562,0.707106781186533));
#28088=DIRECTION('',(0.,2.10269512239613E-16,1.));
#28089=DIRECTION('',(0.,1.,1.87537673078574E-16));
#28090=DIRECTION('',(0.,0.70710678118655,0.707106781186545));
#28091=DIRECTION('',(0.,0.,1.));
#28092=DIRECTION('',(0.,-0.707106781186543,0.707106781186552));
#28093=DIRECTION('',(0.,-1.,-7.50150692314296E-16));
#28094=DIRECTION('',(0.,-0.707106781186548,0.707106781186547));
#28095=DIRECTION('',(0.,0.,1.));
#28096=DIRECTION('',(0.,0.707106781186546,0.707106781186549));
#28097=DIRECTION('',(0.,1.,0.));
#28098=DIRECTION('',(0.,0.707106781186549,-0.707106781186546));
#28099=DIRECTION('',(0.,0.,-1.));
#28100=DIRECTION('',(0.,-0.707106781186546,-0.707106781186549));
#28101=DIRECTION('',(0.,-1.,0.));
#28102=DIRECTION('center_axis',(0.,-1.,-2.10269512239613E-16));
#28103=DIRECTION('ref_axis',(0.,2.10269512239613E-16,-1.));
#28104=DIRECTION('',(0.,-2.10269512239613E-16,1.));
#28105=DIRECTION('',(-1.,0.,0.));
#28106=DIRECTION('',(-1.,0.,0.));
#28107=DIRECTION('center_axis',(0.,-0.707106781186513,-0.707106781186582));
#28108=DIRECTION('ref_axis',(0.,0.707106781186582,-0.707106781186513));
#28109=DIRECTION('',(0.,-0.707106781186582,0.707106781186513));
#28110=DIRECTION('',(-1.,0.,0.));
#28111=DIRECTION('center_axis',(0.,2.95272081017329E-16,-1.));
#28112=DIRECTION('ref_axis',(0.,1.,2.95272081017329E-16));
#28113=DIRECTION('',(0.,-1.,-2.95272081017329E-16));
#28114=DIRECTION('',(-1.,0.,0.));
#28115=DIRECTION('center_axis',(0.,1.,2.55331806268467E-16));
#28116=DIRECTION('ref_axis',(0.,-2.55331806268467E-16,1.));
#28117=DIRECTION('',(0.,2.55331806268467E-16,-1.));
#28118=DIRECTION('',(-1.,0.,0.));
#28119=DIRECTION('center_axis',(0.,-5.90544162034659E-16,1.));
#28120=DIRECTION('ref_axis',(0.,-1.,-5.90544162034659E-16));
#28121=DIRECTION('',(0.,1.,5.90544162034659E-16));
#28122=DIRECTION('',(-1.,0.,0.));
#28123=DIRECTION('center_axis',(0.,-0.707106781186533,0.707106781186562));
#28124=DIRECTION('ref_axis',(0.,-0.707106781186562,-0.707106781186533));
#28125=DIRECTION('',(0.,0.707106781186562,0.707106781186533));
#28126=DIRECTION('',(-1.,0.,0.));
#28127=DIRECTION('center_axis',(0.,-1.,2.10269512239613E-16));
#28128=DIRECTION('ref_axis',(0.,-2.10269512239613E-16,-1.));
#28129=DIRECTION('',(0.,2.10269512239613E-16,1.));
#28130=DIRECTION('',(-1.,0.,0.));
#28131=DIRECTION('center_axis',(0.,-1.87537673078574E-16,1.));
#28132=DIRECTION('ref_axis',(0.,-1.,-1.87537673078574E-16));
#28133=DIRECTION('',(0.,1.,1.87537673078574E-16));
#28134=DIRECTION('',(-1.,0.,0.));
#28135=DIRECTION('center_axis',(0.,-0.707106781186545,0.70710678118655));
#28136=DIRECTION('ref_axis',(0.,-0.70710678118655,-0.707106781186545));
#28137=DIRECTION('',(0.,0.70710678118655,0.707106781186545));
#28138=DIRECTION('',(-1.,0.,0.));
#28139=DIRECTION('center_axis',(0.,-1.,0.));
#28140=DIRECTION('ref_axis',(0.,0.,-1.));
#28141=DIRECTION('',(0.,0.,1.));
#28142=DIRECTION('',(-1.,0.,0.));
#28143=DIRECTION('center_axis',(0.,-0.707106781186552,-0.707106781186543));
#28144=DIRECTION('ref_axis',(0.,0.707106781186543,-0.707106781186553));
#28145=DIRECTION('',(0.,-0.707106781186543,0.707106781186552));
#28146=DIRECTION('',(-1.,0.,0.));
#28147=DIRECTION('center_axis',(0.,7.50150692314296E-16,-1.));
#28148=DIRECTION('ref_axis',(0.,1.,7.50150692314296E-16));
#28149=DIRECTION('',(0.,-1.,-7.50150692314296E-16));
#28150=DIRECTION('center_axis',(1.,0.,0.));
#28151=DIRECTION('ref_axis',(0.,0.,-1.));
#28152=DIRECTION('center_axis',(-1.,0.,0.));
#28153=DIRECTION('ref_axis',(0.,0.,1.));
#28154=DIRECTION('',(0.,0.,1.));
#28155=DIRECTION('',(0.,-0.707106781186548,0.707106781186547));
#28156=DIRECTION('',(0.,-1.,0.));
#28157=DIRECTION('',(0.,-0.707106781186546,-0.707106781186549));
#28158=DIRECTION('',(0.,0.,-1.));
#28159=DIRECTION('',(0.,0.707106781186549,-0.707106781186546));
#28160=DIRECTION('',(0.,1.,0.));
#28161=DIRECTION('',(0.,0.707106781186546,0.707106781186549));
#28162=DIRECTION('center_axis',(0.,-1.,0.));
#28163=DIRECTION('ref_axis',(0.,0.,-1.));
#28164=DIRECTION('',(-1.,0.,0.));
#28165=DIRECTION('',(-1.,0.,0.));
#28166=DIRECTION('center_axis',(0.,-0.707106781186547,-0.707106781186548));
#28167=DIRECTION('ref_axis',(0.,0.707106781186548,-0.707106781186547));
#28168=DIRECTION('',(-1.,0.,0.));
#28169=DIRECTION('center_axis',(0.,0.,-1.));
#28170=DIRECTION('ref_axis',(-1.,0.,0.));
#28171=DIRECTION('',(-1.,0.,0.));
#28172=DIRECTION('center_axis',(0.,0.707106781186549,-0.707106781186546));
#28173=DIRECTION('ref_axis',(0.,0.707106781186546,0.707106781186549));
#28174=DIRECTION('',(-1.,0.,0.));
#28175=DIRECTION('center_axis',(0.,1.,0.));
#28176=DIRECTION('ref_axis',(0.,0.,1.));
#28177=DIRECTION('',(-1.,0.,0.));
#28178=DIRECTION('center_axis',(0.,0.707106781186546,0.707106781186549));
#28179=DIRECTION('ref_axis',(0.,-0.707106781186549,0.707106781186546));
#28180=DIRECTION('',(-1.,0.,0.));
#28181=DIRECTION('center_axis',(0.,0.,1.));
#28182=DIRECTION('ref_axis',(1.,0.,0.));
#28183=DIRECTION('',(-1.,0.,0.));
#28184=DIRECTION('center_axis',(0.,-0.707106781186549,0.707106781186546));
#28185=DIRECTION('ref_axis',(0.,-0.707106781186546,-0.707106781186549));
#28186=DIRECTION('center_axis',(1.,0.,0.));
#28187=DIRECTION('ref_axis',(0.,0.,-1.));
#28188=DIRECTION('',(0.,-0.499999999999999,0.866025403784439));
#28189=DIRECTION('',(0.,0.5,0.866025403784439));
#28190=DIRECTION('',(0.,1.,0.));
#28191=DIRECTION('',(0.,0.499999999999999,-0.866025403784439));
#28192=DIRECTION('',(0.,-0.5,-0.866025403784438));
#28193=DIRECTION('',(0.,-1.,0.));
#28194=DIRECTION('center_axis',(1.,0.,0.));
#28195=DIRECTION('ref_axis',(0.,0.,-1.));
#28196=DIRECTION('',(0.,-1.,-3.00462919747432E-15));
#28197=DIRECTION('',(0.,-0.500000000000008,0.866025403784434));
#28198=DIRECTION('',(0.,0.499999999999998,0.86602540378444));
#28199=DIRECTION('',(0.,1.,3.00462919747432E-15));
#28200=DIRECTION('',(0.,0.500000000000002,-0.866025403784437));
#28201=DIRECTION('',(0.,-0.499999999999997,-0.866025403784441));
#28202=DIRECTION('center_axis',(1.,0.,0.));
#28203=DIRECTION('ref_axis',(0.,0.,-1.));
#28204=DIRECTION('',(0.,-1.,1.00154306582477E-15));
#28205=DIRECTION('',(0.,-0.499999999999999,0.866025403784439));
#28206=DIRECTION('',(0.,0.5,0.866025403784438));
#28207=DIRECTION('',(0.,1.,-1.00154306582477E-15));
#28208=DIRECTION('',(0.,0.5,-0.866025403784439));
#28209=DIRECTION('',(0.,-0.500000000000002,-0.866025403784438));
#28210=DIRECTION('center_axis',(1.,0.,0.));
#28211=DIRECTION('ref_axis',(0.,0.,-1.));
#28212=DIRECTION('',(0.,-1.,1.00154306582478E-15));
#28213=DIRECTION('',(0.,-0.499999999999999,0.866025403784439));
#28214=DIRECTION('',(0.,0.500000000000002,0.866025403784438));
#28215=DIRECTION('',(0.,1.,-1.00154306582478E-15));
#28216=DIRECTION('',(0.,0.499999999999999,-0.866025403784439));
#28217=DIRECTION('',(0.,-0.500000000000002,-0.866025403784438));
#28218=DIRECTION('center_axis',(0.,-0.866025403784438,0.5));
#28219=DIRECTION('ref_axis',(0.,-0.5,-0.866025403784438));
#28220=DIRECTION('',(1.,0.,0.));
#28221=DIRECTION('',(0.,-0.5,-0.866025403784438));
#28222=DIRECTION('',(0.,-0.5,-0.866025403784438));
#28223=DIRECTION('',(1.,0.,0.));
#28224=DIRECTION('center_axis',(0.,0.,1.));
#28225=DIRECTION('ref_axis',(1.,0.,0.));
#28226=DIRECTION('',(0.,-1.,0.));
#28227=DIRECTION('',(0.,-1.,0.));
#28228=DIRECTION('',(1.,0.,0.));
#28229=DIRECTION('center_axis',(0.,0.866025403784439,0.499999999999999));
#28230=DIRECTION('ref_axis',(0.,-0.499999999999999,0.866025403784439));
#28231=DIRECTION('',(0.,-0.499999999999999,0.866025403784439));
#28232=DIRECTION('',(0.,-0.499999999999999,0.866025403784439));
#28233=DIRECTION('',(1.,0.,0.));
#28234=DIRECTION('center_axis',(0.,0.866025403784439,-0.5));
#28235=DIRECTION('ref_axis',(0.,0.5,0.866025403784439));
#28236=DIRECTION('',(0.,0.5,0.866025403784439));
#28237=DIRECTION('',(0.,0.5,0.866025403784439));
#28238=DIRECTION('',(1.,0.,0.));
#28239=DIRECTION('center_axis',(0.,0.,-1.));
#28240=DIRECTION('ref_axis',(-1.,0.,0.));
#28241=DIRECTION('',(0.,1.,0.));
#28242=DIRECTION('',(0.,1.,0.));
#28243=DIRECTION('',(1.,0.,0.));
#28244=DIRECTION('center_axis',(0.,-0.866025403784439,-0.499999999999999));
#28245=DIRECTION('ref_axis',(0.,0.499999999999999,-0.866025403784439));
#28246=DIRECTION('',(0.,0.499999999999999,-0.866025403784439));
#28247=DIRECTION('',(0.,0.499999999999999,-0.866025403784439));
#28248=DIRECTION('center_axis',(1.,0.,0.));
#28249=DIRECTION('ref_axis',(0.,0.,-1.));
#28250=DIRECTION('center_axis',(1.,0.,0.));
#28251=DIRECTION('ref_axis',(0.,0.,-1.));
#28252=DIRECTION('center_axis',(1.,0.,0.));
#28253=DIRECTION('ref_axis',(0.,0.,-1.));
#28254=DIRECTION('center_axis',(1.,0.,0.));
#28255=DIRECTION('ref_axis',(0.,0.,-1.));
#28256=DIRECTION('center_axis',(1.,0.,0.));
#28257=DIRECTION('ref_axis',(0.,0.,-1.));
#28258=DIRECTION('center_axis',(1.,0.,0.));
#28259=DIRECTION('ref_axis',(0.,0.,-1.));
#28260=DIRECTION('center_axis',(0.,-0.866025403784437,-0.500000000000002));
#28261=DIRECTION('ref_axis',(0.,0.500000000000002,-0.866025403784437));
#28262=DIRECTION('',(1.,0.,0.));
#28263=DIRECTION('',(0.,0.500000000000002,-0.866025403784437));
#28264=DIRECTION('',(0.,0.500000000000002,-0.866025403784437));
#28265=DIRECTION('',(1.,0.,0.));
#28266=DIRECTION('center_axis',(0.,-0.866025403784441,0.499999999999997));
#28267=DIRECTION('ref_axis',(0.,-0.499999999999997,-0.866025403784441));
#28268=DIRECTION('',(0.,-0.499999999999997,-0.866025403784441));
#28269=DIRECTION('',(0.,-0.499999999999997,-0.866025403784441));
#28270=DIRECTION('',(1.,0.,0.));
#28271=DIRECTION('center_axis',(0.,-3.00462919747432E-15,1.));
#28272=DIRECTION('ref_axis',(0.,-1.,-3.00462919747432E-15));
#28273=DIRECTION('',(0.,-1.,-3.00462919747432E-15));
#28274=DIRECTION('',(0.,-1.,-3.00462919747432E-15));
#28275=DIRECTION('',(1.,0.,0.));
#28276=DIRECTION('center_axis',(0.,0.866025403784434,0.500000000000008));
#28277=DIRECTION('ref_axis',(0.,-0.500000000000007,0.866025403784434));
#28278=DIRECTION('',(0.,-0.500000000000008,0.866025403784434));
#28279=DIRECTION('',(0.,-0.500000000000008,0.866025403784434));
#28280=DIRECTION('',(1.,0.,0.));
#28281=DIRECTION('center_axis',(0.,0.86602540378444,-0.499999999999998));
#28282=DIRECTION('ref_axis',(0.,0.499999999999998,0.86602540378444));
#28283=DIRECTION('',(0.,0.499999999999998,0.86602540378444));
#28284=DIRECTION('',(0.,0.499999999999998,0.86602540378444));
#28285=DIRECTION('',(1.,0.,0.));
#28286=DIRECTION('center_axis',(0.,3.00462919747432E-15,-1.));
#28287=DIRECTION('ref_axis',(0.,1.,3.00462919747432E-15));
#28288=DIRECTION('',(0.,1.,3.00462919747432E-15));
#28289=DIRECTION('',(0.,1.,3.00462919747432E-15));
#28290=DIRECTION('center_axis',(1.,0.,0.));
#28291=DIRECTION('ref_axis',(0.,0.,-1.));
#28292=DIRECTION('center_axis',(1.,0.,0.));
#28293=DIRECTION('ref_axis',(0.,0.,-1.));
#28294=DIRECTION('center_axis',(1.,0.,0.));
#28295=DIRECTION('ref_axis',(0.,0.,-1.));
#28296=DIRECTION('center_axis',(1.,0.,0.));
#28297=DIRECTION('ref_axis',(0.,0.,-1.));
#28298=DIRECTION('center_axis',(1.,0.,0.));
#28299=DIRECTION('ref_axis',(0.,0.,-1.));
#28300=DIRECTION('center_axis',(1.,0.,0.));
#28301=DIRECTION('ref_axis',(0.,0.,-1.));
#28302=DIRECTION('center_axis',(0.,-0.866025403784439,-0.499999999999999));
#28303=DIRECTION('ref_axis',(0.,0.499999999999999,-0.866025403784439));
#28304=DIRECTION('',(1.,0.,0.));
#28305=DIRECTION('',(0.,0.499999999999999,-0.866025403784439));
#28306=DIRECTION('',(0.,0.499999999999999,-0.866025403784439));
#28307=DIRECTION('',(1.,0.,0.));
#28308=DIRECTION('center_axis',(0.,-0.866025403784438,0.500000000000002));
#28309=DIRECTION('ref_axis',(0.,-0.500000000000002,-0.866025403784438));
#28310=DIRECTION('',(0.,-0.500000000000002,-0.866025403784438));
#28311=DIRECTION('',(0.,-0.500000000000002,-0.866025403784438));
#28312=DIRECTION('',(1.,0.,0.));
#28313=DIRECTION('center_axis',(0.,1.00154306582478E-15,1.));
#28314=DIRECTION('ref_axis',(0.,-1.,1.00154306582478E-15));
#28315=DIRECTION('',(0.,-1.,1.00154306582478E-15));
#28316=DIRECTION('',(0.,-1.,1.00154306582478E-15));
#28317=DIRECTION('',(1.,0.,0.));
#28318=DIRECTION('center_axis',(0.,0.866025403784439,0.499999999999999));
#28319=DIRECTION('ref_axis',(0.,-0.499999999999999,0.866025403784439));
#28320=DIRECTION('',(0.,-0.499999999999999,0.866025403784439));
#28321=DIRECTION('',(0.,-0.499999999999999,0.866025403784439));
#28322=DIRECTION('',(1.,0.,0.));
#28323=DIRECTION('center_axis',(0.,0.866025403784438,-0.500000000000002));
#28324=DIRECTION('ref_axis',(0.,0.500000000000002,0.866025403784438));
#28325=DIRECTION('',(0.,0.500000000000002,0.866025403784438));
#28326=DIRECTION('',(0.,0.500000000000002,0.866025403784438));
#28327=DIRECTION('',(1.,0.,0.));
#28328=DIRECTION('center_axis',(0.,-1.00154306582478E-15,-1.));
#28329=DIRECTION('ref_axis',(0.,1.,-1.00154306582478E-15));
#28330=DIRECTION('',(0.,1.,-1.00154306582478E-15));
#28331=DIRECTION('',(0.,1.,-1.00154306582478E-15));
#28332=DIRECTION('center_axis',(1.,0.,0.));
#28333=DIRECTION('ref_axis',(0.,0.,-1.));
#28334=DIRECTION('center_axis',(1.,0.,0.));
#28335=DIRECTION('ref_axis',(0.,0.,-1.));
#28336=DIRECTION('center_axis',(1.,0.,0.));
#28337=DIRECTION('ref_axis',(0.,0.,-1.));
#28338=DIRECTION('center_axis',(1.,0.,0.));
#28339=DIRECTION('ref_axis',(0.,0.,-1.));
#28340=DIRECTION('center_axis',(1.,0.,0.));
#28341=DIRECTION('ref_axis',(0.,0.,-1.));
#28342=DIRECTION('center_axis',(1.,0.,0.));
#28343=DIRECTION('ref_axis',(0.,0.,-1.));
#28344=DIRECTION('center_axis',(0.,-0.866025403784439,-0.5));
#28345=DIRECTION('ref_axis',(0.,0.5,-0.866025403784439));
#28346=DIRECTION('',(1.,0.,0.));
#28347=DIRECTION('',(0.,0.5,-0.866025403784439));
#28348=DIRECTION('',(0.,0.5,-0.866025403784439));
#28349=DIRECTION('',(1.,0.,0.));
#28350=DIRECTION('center_axis',(0.,-0.866025403784438,0.500000000000002));
#28351=DIRECTION('ref_axis',(0.,-0.500000000000002,-0.866025403784438));
#28352=DIRECTION('',(0.,-0.500000000000002,-0.866025403784438));
#28353=DIRECTION('',(0.,-0.500000000000002,-0.866025403784438));
#28354=DIRECTION('',(1.,0.,0.));
#28355=DIRECTION('center_axis',(0.,1.00154306582477E-15,1.));
#28356=DIRECTION('ref_axis',(0.,-1.,1.00154306582477E-15));
#28357=DIRECTION('',(0.,-1.,1.00154306582477E-15));
#28358=DIRECTION('',(0.,-1.,1.00154306582477E-15));
#28359=DIRECTION('',(1.,0.,0.));
#28360=DIRECTION('center_axis',(0.,0.866025403784439,0.499999999999999));
#28361=DIRECTION('ref_axis',(0.,-0.499999999999999,0.866025403784439));
#28362=DIRECTION('',(0.,-0.499999999999999,0.866025403784439));
#28363=DIRECTION('',(0.,-0.499999999999999,0.866025403784439));
#28364=DIRECTION('',(1.,0.,0.));
#28365=DIRECTION('center_axis',(0.,0.866025403784438,-0.5));
#28366=DIRECTION('ref_axis',(0.,0.5,0.866025403784438));
#28367=DIRECTION('',(0.,0.5,0.866025403784438));
#28368=DIRECTION('',(0.,0.5,0.866025403784438));
#28369=DIRECTION('',(1.,0.,0.));
#28370=DIRECTION('center_axis',(0.,-1.00154306582477E-15,-1.));
#28371=DIRECTION('ref_axis',(0.,1.,-1.00154306582477E-15));
#28372=DIRECTION('',(0.,1.,-1.00154306582477E-15));
#28373=DIRECTION('',(0.,1.,-1.00154306582477E-15));
#28374=DIRECTION('center_axis',(1.,0.,0.));
#28375=DIRECTION('ref_axis',(0.,0.,-1.));
#28376=DIRECTION('center_axis',(1.,0.,0.));
#28377=DIRECTION('ref_axis',(0.,0.,-1.));
#28378=DIRECTION('center_axis',(1.,0.,0.));
#28379=DIRECTION('ref_axis',(0.,0.,-1.));
#28380=DIRECTION('center_axis',(1.,0.,0.));
#28381=DIRECTION('ref_axis',(0.,0.,-1.));
#28382=DIRECTION('center_axis',(1.,0.,0.));
#28383=DIRECTION('ref_axis',(0.,0.,-1.));
#28384=DIRECTION('center_axis',(1.,0.,0.));
#28385=DIRECTION('ref_axis',(0.,0.,-1.));
#28386=DIRECTION('center_axis',(1.,0.,0.));
#28387=DIRECTION('ref_axis',(0.,0.,-1.));
#28388=DIRECTION('center_axis',(1.,0.,0.));
#28389=DIRECTION('ref_axis',(0.,0.,-1.));
#28390=DIRECTION('center_axis',(-1.,0.,0.));
#28391=DIRECTION('ref_axis',(0.,0.,1.));
#28392=DIRECTION('center_axis',(-1.,0.,0.));
#28393=DIRECTION('ref_axis',(0.,0.,1.));
#28394=DIRECTION('axis',(0.,0.,1.));
#28395=DIRECTION('refdir',(1.,0.,0.));
#28396=DIRECTION('center_axis',(0.,1.,0.));
#28397=DIRECTION('ref_axis',(0.,0.,1.));
#28398=DIRECTION('',(0.,1.,0.));
#28399=DIRECTION('center_axis',(1.,0.,0.));
#28400=DIRECTION('ref_axis',(0.,0.,-1.));
#28401=DIRECTION('center_axis',(-1.,0.,0.));
#28402=DIRECTION('ref_axis',(0.,0.,1.));
#28403=DIRECTION('',(0.707106781186548,-8.65956056235493E-17,0.707106781186547));
#28404=DIRECTION('center_axis',(-1.,0.,0.));
#28405=DIRECTION('ref_axis',(0.,0.,1.));
#28406=DIRECTION('center_axis',(-1.,0.,0.));
#28407=DIRECTION('ref_axis',(0.,0.,1.));
#28408=DIRECTION('center_axis',(-1.,0.,0.));
#28409=DIRECTION('ref_axis',(0.,0.,1.));
#28410=DIRECTION('center_axis',(-1.,0.,0.));
#28411=DIRECTION('ref_axis',(0.,0.,1.));
#28412=DIRECTION('',(-0.707106781186547,-8.65956056235494E-17,-0.707106781186548));
#28413=DIRECTION('center_axis',(-1.,0.,0.));
#28414=DIRECTION('ref_axis',(0.,0.,1.));
#28415=DIRECTION('center_axis',(-1.,0.,0.));
#28416=DIRECTION('ref_axis',(0.,0.,1.));
#28417=DIRECTION('',(-1.,0.,0.));
#28418=DIRECTION('center_axis',(-1.,0.,0.));
#28419=DIRECTION('ref_axis',(0.,0.,1.));
#28420=DIRECTION('center_axis',(-1.,0.,0.));
#28421=DIRECTION('ref_axis',(0.,0.,1.));
#28422=DIRECTION('',(-1.,0.,0.));
#28423=DIRECTION('center_axis',(-1.,0.,0.));
#28424=DIRECTION('ref_axis',(0.,0.,1.));
#28425=DIRECTION('',(1.,0.,0.));
#28426=DIRECTION('center_axis',(-1.,0.,0.));
#28427=DIRECTION('ref_axis',(0.,0.,1.));
#28428=DIRECTION('center_axis',(-1.,0.,0.));
#28429=DIRECTION('ref_axis',(0.,0.,1.));
#28430=DIRECTION('',(1.,0.,0.));
#28431=DIRECTION('center_axis',(-1.,0.,0.));
#28432=DIRECTION('ref_axis',(0.,0.,1.));
#28433=DIRECTION('center_axis',(-1.,0.,0.));
#28434=DIRECTION('ref_axis',(0.,0.,1.));
#28435=DIRECTION('center_axis',(-1.,0.,0.));
#28436=DIRECTION('ref_axis',(0.,0.,1.));
#28437=DIRECTION('',(-1.,0.,0.));
#28438=DIRECTION('center_axis',(-1.,0.,0.));
#28439=DIRECTION('ref_axis',(0.,0.,1.));
#28440=DIRECTION('',(1.,0.,0.));
#28441=DIRECTION('center_axis',(-1.,0.,0.));
#28442=DIRECTION('ref_axis',(0.,1.22464679914735E-16,-1.));
#28443=DIRECTION('center_axis',(-1.,0.,0.));
#28444=DIRECTION('ref_axis',(0.,0.,1.));
#28445=DIRECTION('',(-1.,0.,0.));
#28446=DIRECTION('center_axis',(-1.,0.,0.));
#28447=DIRECTION('ref_axis',(0.,0.,1.));
#28448=DIRECTION('',(1.,0.,0.));
#28449=DIRECTION('center_axis',(-1.,0.,0.));
#28450=DIRECTION('ref_axis',(0.,0.,1.));
#28451=DIRECTION('center_axis',(-1.,0.,0.));
#28452=DIRECTION('ref_axis',(0.,0.,1.));
#28453=DIRECTION('',(-1.,0.,0.));
#28454=DIRECTION('center_axis',(-1.,0.,0.));
#28455=DIRECTION('ref_axis',(0.,0.,1.));
#28456=DIRECTION('',(1.,0.,0.));
#28457=DIRECTION('center_axis',(1.,0.,0.));
#28458=DIRECTION('ref_axis',(0.,0.,-1.));
#28459=DIRECTION('center_axis',(1.,0.,0.));
#28460=DIRECTION('ref_axis',(0.,0.,-1.));
#28461=DIRECTION('',(0.,0.707106781186548,0.707106781186548));
#28462=DIRECTION('',(0.,0.707106781186547,-0.707106781186547));
#28463=DIRECTION('',(0.,-0.707106781186547,-0.707106781186547));
#28464=DIRECTION('',(0.,-0.707106781186548,0.707106781186548));
#28465=DIRECTION('center_axis',(-1.,0.,0.));
#28466=DIRECTION('ref_axis',(0.,0.,1.));
#28467=DIRECTION('',(0.,-0.707106781186548,-0.707106781186548));
#28468=DIRECTION('',(0.,0.707106781186548,-0.707106781186548));
#28469=DIRECTION('',(0.,0.707106781186547,0.707106781186547));
#28470=DIRECTION('',(0.,-0.707106781186547,0.707106781186547));
#28471=DIRECTION('center_axis',(0.,-0.707106781186548,-0.707106781186548));
#28472=DIRECTION('ref_axis',(0.,0.707106781186548,-0.707106781186548));
#28473=DIRECTION('center_axis',(0.,-0.707106781186548,0.707106781186548));
#28474=DIRECTION('ref_axis',(0.,-0.707106781186548,-0.707106781186548));
#28475=DIRECTION('center_axis',(0.,0.707106781186547,0.707106781186548));
#28476=DIRECTION('ref_axis',(0.,-0.707106781186548,0.707106781186547));
#28477=DIRECTION('center_axis',(0.,0.707106781186548,-0.707106781186547));
#28478=DIRECTION('ref_axis',(0.,0.707106781186547,0.707106781186548));
#28479=DIRECTION('center_axis',(0.,-1.,0.));
#28480=DIRECTION('ref_axis',(0.,0.,-1.));
#28481=DIRECTION('center_axis',(0.,-1.,0.));
#28482=DIRECTION('ref_axis',(0.,0.,1.));
#28483=DIRECTION('',(8.65956056235491E-17,0.70710678118655,-0.707106781186545));
#28484=DIRECTION('center_axis',(0.,1.,0.));
#28485=DIRECTION('ref_axis',(0.,0.,1.));
#28486=DIRECTION('center_axis',(0.,1.,0.));
#28487=DIRECTION('ref_axis',(0.,0.,1.));
#28488=DIRECTION('center_axis',(0.,-1.,0.));
#28489=DIRECTION('ref_axis',(0.,0.,-1.));
#28490=DIRECTION('',(8.65956056235495E-17,-0.707106781186546,0.707106781186549));
#28491=DIRECTION('center_axis',(0.,-1.,0.));
#28492=DIRECTION('ref_axis',(0.,0.,-1.));
#28493=DIRECTION('center_axis',(0.,-1.,0.));
#28494=DIRECTION('ref_axis',(0.,0.,-1.));
#28495=DIRECTION('center_axis',(0.,-1.,0.));
#28496=DIRECTION('ref_axis',(0.,0.,-1.));
#28497=DIRECTION('',(0.,1.,0.));
#28498=DIRECTION('center_axis',(0.,-1.,0.));
#28499=DIRECTION('ref_axis',(0.,0.,-1.));
#28500=DIRECTION('center_axis',(0.,1.,0.));
#28501=DIRECTION('ref_axis',(0.,0.,1.));
#28502=DIRECTION('',(-0.866025403784439,0.,-0.5));
#28503=DIRECTION('',(0.,0.,-1.));
#28504=DIRECTION('',(0.866025403784439,0.,-0.5));
#28505=DIRECTION('',(0.866025403784439,0.,0.5));
#28506=DIRECTION('',(7.5115729936858E-16,0.,1.));
#28507=DIRECTION('',(-0.866025403784439,0.,0.5));
#28508=DIRECTION('center_axis',(0.5,0.,-0.866025403784439));
#28509=DIRECTION('ref_axis',(-0.866025403784439,0.,-0.5));
#28510=DIRECTION('',(0.,1.,0.));
#28511=DIRECTION('',(-0.866025403784439,0.,-0.5));
#28512=DIRECTION('',(0.,1.,0.));
#28513=DIRECTION('center_axis',(1.,0.,0.));
#28514=DIRECTION('ref_axis',(0.,0.,-1.));
#28515=DIRECTION('',(0.,0.,-1.));
#28516=DIRECTION('',(0.,1.,0.));
#28517=DIRECTION('center_axis',(0.5,0.,0.866025403784439));
#28518=DIRECTION('ref_axis',(0.866025403784439,0.,-0.5));
#28519=DIRECTION('',(0.866025403784439,0.,-0.5));
#28520=DIRECTION('',(0.,1.,0.));
#28521=DIRECTION('center_axis',(-0.5,0.,0.866025403784439));
#28522=DIRECTION('ref_axis',(0.866025403784439,0.,0.5));
#28523=DIRECTION('',(0.866025403784439,0.,0.5));
#28524=DIRECTION('',(0.,1.,0.));
#28525=DIRECTION('center_axis',(-1.,0.,7.5115729936858E-16));
#28526=DIRECTION('ref_axis',(7.5115729936858E-16,0.,1.));
#28527=DIRECTION('',(7.5115729936858E-16,0.,1.));
#28528=DIRECTION('',(0.,1.,0.));
#28529=DIRECTION('center_axis',(-0.5,0.,-0.866025403784439));
#28530=DIRECTION('ref_axis',(-0.866025403784439,0.,0.5));
#28531=DIRECTION('',(-0.866025403784439,0.,0.5));
#28532=DIRECTION('center_axis',(0.,1.,0.));
#28533=DIRECTION('ref_axis',(0.,0.,1.));
#28534=DIRECTION('axis',(0.,0.,1.));
#28535=DIRECTION('refdir',(1.,0.,0.));
#28536=DIRECTION('center_axis',(-1.,0.,0.));
#28537=DIRECTION('ref_axis',(0.,0.,1.));
#28538=DIRECTION('center_axis',(-1.,0.,0.));
#28539=DIRECTION('ref_axis',(0.,0.,1.));
#28540=DIRECTION('',(1.,0.,0.));
#28541=DIRECTION('center_axis',(-1.,0.,0.));
#28542=DIRECTION('ref_axis',(0.,0.,1.));
#28543=DIRECTION('center_axis',(-1.,0.,0.));
#28544=DIRECTION('ref_axis',(0.,0.,1.));
#28545=DIRECTION('center_axis',(-1.,0.,0.));
#28546=DIRECTION('ref_axis',(0.,0.,1.));
#28547=DIRECTION('',(-1.,0.,0.));
#28548=DIRECTION('center_axis',(-1.,0.,0.));
#28549=DIRECTION('ref_axis',(0.,0.,1.));
#28550=DIRECTION('center_axis',(1.,0.,0.));
#28551=DIRECTION('ref_axis',(0.,0.,-1.));
#28552=DIRECTION('center_axis',(-1.,0.,0.));
#28553=DIRECTION('ref_axis',(0.,0.,1.));
#28554=DIRECTION('',(4.93038065763132E-32,-9.65818659854845E-31,1.));
#28555=DIRECTION('',(1.,-1.4791141972894E-31,-4.93038065763132E-32));
#28556=DIRECTION('',(-1.43585651792049E-16,5.55111512312588E-17,-1.));
#28557=DIRECTION('',(-1.,2.24963064604522E-16,1.43585651792049E-16));
#28558=DIRECTION('',(4.93038065763132E-32,-9.65818659854845E-31,1.));
#28559=DIRECTION('',(1.,-1.4791141972894E-31,-4.93038065763132E-32));
#28560=DIRECTION('',(4.93038065763132E-32,-9.65818659854845E-31,1.));
#28561=DIRECTION('',(1.,-1.4791141972894E-31,-4.93038065763132E-32));
#28562=DIRECTION('axis',(0.,0.,1.));
#28563=DIRECTION('refdir',(1.,0.,0.));
#28564=DIRECTION('axis',(0.,0.,1.));
#28565=DIRECTION('refdir',(1.,0.,0.));
#28566=DIRECTION('center_axis',(0.,1.,3.01691039300315E-16));
#28567=DIRECTION('ref_axis',(0.,-3.01691039300315E-16,1.));
#28568=DIRECTION('center_axis',(0.,1.,3.01691039300315E-16));
#28569=DIRECTION('ref_axis',(0.,-3.01691039300315E-16,1.));
#28570=DIRECTION('',(0.,1.,3.01691039300315E-16));
#28571=DIRECTION('center_axis',(0.,1.,3.01691039300315E-16));
#28572=DIRECTION('ref_axis',(0.,-3.01691039300315E-16,1.));
#28573=DIRECTION('center_axis',(0.,1.,3.01691039300315E-16));
#28574=DIRECTION('ref_axis',(0.,-3.01691039300315E-16,1.));
#28575=DIRECTION('center_axis',(0.,1.,3.01691039300315E-16));
#28576=DIRECTION('ref_axis',(0.,-3.01691039300315E-16,1.));
#28577=DIRECTION('',(0.,1.,3.01691039300315E-16));
#28578=DIRECTION('center_axis',(0.,1.,3.01691039300315E-16));
#28579=DIRECTION('ref_axis',(0.,-3.01691039300315E-16,1.));
#28580=DIRECTION('center_axis',(-1.,0.,0.));
#28581=DIRECTION('ref_axis',(0.,0.,1.));
#28582=DIRECTION('center_axis',(1.,0.,0.));
#28583=DIRECTION('ref_axis',(0.,0.,-1.));
#28584=DIRECTION('',(-1.,0.,0.));
#28585=DIRECTION('center_axis',(1.,0.,0.));
#28586=DIRECTION('ref_axis',(0.,0.,-1.));
#28587=DIRECTION('center_axis',(1.,0.,0.));
#28588=DIRECTION('ref_axis',(0.,0.,-1.));
#28589=DIRECTION('',(0.,-2.10269512239613E-16,1.));
#28590=DIRECTION('',(0.,-0.707106781186582,0.707106781186513));
#28591=DIRECTION('',(0.,-1.,-2.95272081017329E-16));
#28592=DIRECTION('',(0.,2.55331806268467E-16,-1.));
#28593=DIRECTION('',(0.,1.,5.90544162034659E-16));
#28594=DIRECTION('',(0.,0.707106781186562,0.707106781186533));
#28595=DIRECTION('',(0.,2.10269512239613E-16,1.));
#28596=DIRECTION('',(0.,1.,1.87537673078574E-16));
#28597=DIRECTION('',(0.,0.70710678118655,0.707106781186545));
#28598=DIRECTION('',(0.,0.,1.));
#28599=DIRECTION('',(0.,-0.707106781186543,0.707106781186552));
#28600=DIRECTION('',(0.,-1.,-7.50150692314296E-16));
#28601=DIRECTION('center_axis',(1.,0.,0.));
#28602=DIRECTION('ref_axis',(0.,0.,-1.));
#28603=DIRECTION('',(0.,-2.10269512239613E-16,1.));
#28604=DIRECTION('',(0.,-1.,-7.50150692314296E-16));
#28605=DIRECTION('',(0.,-0.707106781186543,0.707106781186552));
#28606=DIRECTION('',(0.,0.,1.));
#28607=DIRECTION('',(0.,0.70710678118655,0.707106781186545));
#28608=DIRECTION('',(0.,1.,1.87537673078574E-16));
#28609=DIRECTION('',(0.,2.10269512239613E-16,1.));
#28610=DIRECTION('',(0.,0.707106781186562,0.707106781186533));
#28611=DIRECTION('',(0.,1.,5.90544162034659E-16));
#28612=DIRECTION('',(0.,2.55331806268467E-16,-1.));
#28613=DIRECTION('',(0.,-1.,-2.95272081017329E-16));
#28614=DIRECTION('',(0.,-0.707106781186582,0.707106781186513));
#28615=DIRECTION('center_axis',(0.,-1.,-2.10269512239613E-16));
#28616=DIRECTION('ref_axis',(0.,2.10269512239613E-16,-1.));
#28617=DIRECTION('',(-1.,0.,0.));
#28618=DIRECTION('',(-1.,0.,0.));
#28619=DIRECTION('center_axis',(0.,-0.707106781186513,-0.707106781186582));
#28620=DIRECTION('ref_axis',(0.,0.707106781186582,-0.707106781186513));
#28621=DIRECTION('',(-1.,0.,0.));
#28622=DIRECTION('center_axis',(0.,2.95272081017329E-16,-1.));
#28623=DIRECTION('ref_axis',(0.,1.,2.95272081017329E-16));
#28624=DIRECTION('',(-1.,0.,0.));
#28625=DIRECTION('center_axis',(0.,1.,2.55331806268467E-16));
#28626=DIRECTION('ref_axis',(0.,-2.55331806268467E-16,1.));
#28627=DIRECTION('',(-1.,0.,0.));
#28628=DIRECTION('center_axis',(0.,-5.90544162034659E-16,1.));
#28629=DIRECTION('ref_axis',(0.,-1.,-5.90544162034659E-16));
#28630=DIRECTION('',(-1.,0.,0.));
#28631=DIRECTION('center_axis',(0.,-0.707106781186533,0.707106781186562));
#28632=DIRECTION('ref_axis',(0.,-0.707106781186562,-0.707106781186533));
#28633=DIRECTION('',(-1.,0.,0.));
#28634=DIRECTION('center_axis',(0.,-1.,2.10269512239613E-16));
#28635=DIRECTION('ref_axis',(0.,-2.10269512239613E-16,-1.));
#28636=DIRECTION('',(-1.,0.,0.));
#28637=DIRECTION('center_axis',(0.,-1.87537673078574E-16,1.));
#28638=DIRECTION('ref_axis',(0.,-1.,-1.87537673078574E-16));
#28639=DIRECTION('',(-1.,0.,0.));
#28640=DIRECTION('center_axis',(0.,-0.707106781186545,0.70710678118655));
#28641=DIRECTION('ref_axis',(0.,-0.70710678118655,-0.707106781186545));
#28642=DIRECTION('',(-1.,0.,0.));
#28643=DIRECTION('center_axis',(0.,-1.,0.));
#28644=DIRECTION('ref_axis',(0.,0.,-1.));
#28645=DIRECTION('',(-1.,0.,0.));
#28646=DIRECTION('center_axis',(0.,-0.707106781186552,-0.707106781186543));
#28647=DIRECTION('ref_axis',(0.,0.707106781186543,-0.707106781186553));
#28648=DIRECTION('',(-1.,0.,0.));
#28649=DIRECTION('center_axis',(0.,7.50150692314296E-16,-1.));
#28650=DIRECTION('ref_axis',(0.,1.,7.50150692314296E-16));
#28651=DIRECTION('center_axis',(-1.,-1.73472347597681E-16,0.));
#28652=DIRECTION('ref_axis',(3.17206578464331E-16,-1.,0.));
#28653=DIRECTION('center_axis',(-1.,-1.73472347597681E-16,0.));
#28654=DIRECTION('ref_axis',(1.73472347597681E-16,-1.,0.));
#28655=DIRECTION('center_axis',(2.12442355226077E-32,-1.22464679914735E-16,
-1.));
#28656=DIRECTION('ref_axis',(0.,1.,-1.22464679914735E-16));
#28657=DIRECTION('center_axis',(-1.,-1.73472347597681E-16,0.));
#28658=DIRECTION('ref_axis',(1.73472347597681E-16,-1.,0.));
#28659=DIRECTION('center_axis',(-1.,-1.73472347597681E-16,0.));
#28660=DIRECTION('ref_axis',(1.73472347597681E-16,-1.,0.));
#28661=DIRECTION('',(-1.,-1.73472347597681E-16,0.));
#28662=DIRECTION('center_axis',(-1.,-1.73472347597681E-16,0.));
#28663=DIRECTION('ref_axis',(1.73472347597681E-16,-1.,0.));
#28664=DIRECTION('center_axis',(-1.,-1.73472347597681E-16,0.));
#28665=DIRECTION('ref_axis',(1.58603289232165E-16,-1.,0.));
#28666=DIRECTION('center_axis',(2.12442355226077E-32,-1.22464679914735E-16,
-1.));
#28667=DIRECTION('ref_axis',(-1.98254111540206E-16,1.,-1.22464679914735E-16));
#28668=DIRECTION('center_axis',(-1.,-1.73472347597681E-16,0.));
#28669=DIRECTION('ref_axis',(1.73472347597681E-16,-1.,0.));
#28670=DIRECTION('center_axis',(-1.,-1.73472347597681E-16,0.));
#28671=DIRECTION('ref_axis',(1.73472347597681E-16,-1.,0.));
#28672=DIRECTION('center_axis',(-1.,-1.73472347597681E-16,0.));
#28673=DIRECTION('ref_axis',(1.73472347597681E-16,-1.,0.));
#28674=DIRECTION('',(1.,1.73472347597681E-16,0.));
#28675=DIRECTION('center_axis',(-1.,-1.73472347597681E-16,0.));
#28676=DIRECTION('ref_axis',(1.73472347597681E-16,-1.,0.));
#28677=DIRECTION('center_axis',(-1.,-1.73472347597681E-16,0.));
#28678=DIRECTION('ref_axis',(1.73472347597681E-16,-1.,0.));
#28679=DIRECTION('center_axis',(-1.,-1.73472347597681E-16,0.));
#28680=DIRECTION('ref_axis',(1.73472347597681E-16,-1.,0.));
#28681=DIRECTION('',(-1.,-1.73472347597681E-16,0.));
#28682=DIRECTION('center_axis',(-1.,-1.73472347597681E-16,0.));
#28683=DIRECTION('ref_axis',(1.73472347597681E-16,-1.,0.));
#28684=DIRECTION('center_axis',(-1.,-1.73472347597681E-16,0.));
#28685=DIRECTION('ref_axis',(1.36642833800019E-16,-1.,0.));
#28686=DIRECTION('center_axis',(-1.,-1.73472347597681E-16,0.));
#28687=DIRECTION('ref_axis',(1.73472347597681E-16,-1.,0.));
#28688=DIRECTION('center_axis',(2.12442355226077E-32,-1.22464679914735E-16,
-1.));
#28689=DIRECTION('ref_axis',(-1.70803542250024E-16,1.,-1.22464679914735E-16));
#28690=DIRECTION('center_axis',(-1.,-1.73472347597681E-16,0.));
#28691=DIRECTION('ref_axis',(1.73472347597681E-16,-1.,0.));
#28692=DIRECTION('center_axis',(-1.,-1.73472347597681E-16,0.));
#28693=DIRECTION('ref_axis',(1.73472347597681E-16,-1.,0.));
#28694=DIRECTION('',(1.,1.73472347597681E-16,0.));
#28695=DIRECTION('center_axis',(-1.,-1.73472347597681E-16,0.));
#28696=DIRECTION('ref_axis',(1.73472347597681E-16,-1.,0.));
#28697=DIRECTION('center_axis',(-1.,-1.73472347597681E-16,0.));
#28698=DIRECTION('ref_axis',(1.36642833800019E-16,-1.,0.));
#28699=DIRECTION('center_axis',(2.12442355226077E-32,-1.22464679914735E-16,
-1.));
#28700=DIRECTION('ref_axis',(-1.70803542250024E-16,1.,-1.22464679914735E-16));
#28701=DIRECTION('center_axis',(-1.,-1.73472347597681E-16,0.));
#28702=DIRECTION('ref_axis',(1.73472347597681E-16,-1.,0.));
#28703=DIRECTION('center_axis',(-1.,-1.73472347597681E-16,0.));
#28704=DIRECTION('ref_axis',(1.73472347597681E-16,-1.,0.));
#28705=DIRECTION('center_axis',(-1.,-1.73472347597681E-16,0.));
#28706=DIRECTION('ref_axis',(1.73472347597681E-16,-1.,0.));
#28707=DIRECTION('',(-1.,-1.73472347597681E-16,0.));
#28708=DIRECTION('center_axis',(-1.,-1.73472347597681E-16,0.));
#28709=DIRECTION('ref_axis',(1.73472347597681E-16,-1.,0.));
#28710=DIRECTION('center_axis',(-1.,-1.73472347597681E-16,0.));
#28711=DIRECTION('ref_axis',(1.73472347597681E-16,-1.,0.));
#28712=DIRECTION('center_axis',(-1.,-1.73472347597681E-16,0.));
#28713=DIRECTION('ref_axis',(1.73472347597681E-16,-1.,0.));
#28714=DIRECTION('',(1.,1.73472347597681E-16,0.));
#28715=DIRECTION('center_axis',(-1.,-1.73472347597681E-16,0.));
#28716=DIRECTION('ref_axis',(1.73472347597681E-16,-1.,0.));
#28717=DIRECTION('center_axis',(-1.,-1.73472347597681E-16,0.));
#28718=DIRECTION('ref_axis',(1.73472347597681E-16,-1.,0.));
#28719=DIRECTION('center_axis',(-1.,-1.73472347597681E-16,0.));
#28720=DIRECTION('ref_axis',(1.73472347597681E-16,-1.,0.));
#28721=DIRECTION('center_axis',(1.,1.73472347597681E-16,0.));
#28722=DIRECTION('ref_axis',(-1.73472347597681E-16,1.,0.));
#28723=DIRECTION('center_axis',(1.,1.73472347597681E-16,0.));
#28724=DIRECTION('ref_axis',(-1.73472347597681E-16,1.,0.));
#28725=DIRECTION('center_axis',(1.,1.73472347597681E-16,0.));
#28726=DIRECTION('ref_axis',(-1.73472347597681E-16,1.,0.));
#28727=DIRECTION('center_axis',(-1.,-1.73472347597681E-16,0.));
#28728=DIRECTION('ref_axis',(1.73472347597681E-16,-1.,0.));
#28729=DIRECTION('axis',(0.,0.,1.));
#28730=DIRECTION('refdir',(1.,0.,0.));
#28731=DIRECTION('center_axis',(-1.,0.,0.));
#28732=DIRECTION('ref_axis',(0.,0.,1.));
#28733=DIRECTION('center_axis',(1.,0.,0.));
#28734=DIRECTION('ref_axis',(0.,0.,-1.));
#28735=DIRECTION('',(-1.,0.,0.));
#28736=DIRECTION('center_axis',(1.,0.,0.));
#28737=DIRECTION('ref_axis',(0.,0.,-1.));
#28738=DIRECTION('center_axis',(-1.,0.,0.));
#28739=DIRECTION('ref_axis',(0.,0.,1.));
#28740=DIRECTION('center_axis',(1.,0.,0.));
#28741=DIRECTION('ref_axis',(0.,0.,-1.));
#28742=DIRECTION('',(-1.,0.,0.));
#28743=DIRECTION('center_axis',(1.,0.,0.));
#28744=DIRECTION('ref_axis',(0.,0.,-1.));
#28745=DIRECTION('center_axis',(-1.,0.,0.));
#28746=DIRECTION('ref_axis',(0.,1.,6.12323399573676E-17));
#28747=DIRECTION('center_axis',(-1.,0.,0.));
#28748=DIRECTION('ref_axis',(0.,0.,-1.));
#28749=DIRECTION('',(-1.,0.,0.));
#28750=DIRECTION('center_axis',(-1.,0.,0.));
#28751=DIRECTION('ref_axis',(0.,0.,-1.));
#28752=DIRECTION('',(-1.,0.,0.));
#28753=DIRECTION('center_axis',(-1.,0.,0.));
#28754=DIRECTION('ref_axis',(0.,1.,6.12323399573677E-17));
#28755=DIRECTION('center_axis',(1.,0.,0.));
#28756=DIRECTION('ref_axis',(0.,0.,-1.));
#28757=DIRECTION('',(-1.,0.,0.));
#28758=DIRECTION('center_axis',(1.,0.,0.));
#28759=DIRECTION('ref_axis',(0.,0.,-1.));
#28760=DIRECTION('',(-1.,0.,0.));
#28761=DIRECTION('center_axis',(1.,0.,0.));
#28762=DIRECTION('ref_axis',(0.,0.,-1.));
#28763=DIRECTION('',(0.,1.020425574104E-15,-1.));
#28764=DIRECTION('center_axis',(1.,0.,0.));
#28765=DIRECTION('ref_axis',(0.,0.,-1.));
#28766=DIRECTION('',(0.,1.,0.));
#28767=DIRECTION('center_axis',(-1.,0.,0.));
#28768=DIRECTION('ref_axis',(0.,0.,-1.));
#28769=DIRECTION('center_axis',(-1.,0.,0.));
#28770=DIRECTION('ref_axis',(0.,0.,-1.));
#28771=DIRECTION('',(0.,-1.,0.));
#28772=DIRECTION('center_axis',(1.,0.,0.));
#28773=DIRECTION('ref_axis',(0.,0.,-1.));
#28774=DIRECTION('',(0.,-1.020425574104E-15,-1.));
#28775=DIRECTION('',(0.,1.,-1.61730259095139E-16));
#28776=DIRECTION('',(0.,-1.,-1.61730259095139E-16));
#28777=DIRECTION('center_axis',(1.,0.,0.));
#28778=DIRECTION('ref_axis',(0.,0.,-1.));
#28779=DIRECTION('',(0.,1.020425574104E-15,-1.));
#28780=DIRECTION('',(0.,-1.,-1.61730259095139E-16));
#28781=DIRECTION('',(0.,1.,-1.61730259095139E-16));
#28782=DIRECTION('',(0.,-1.020425574104E-15,-1.));
#28783=DIRECTION('center_axis',(1.,0.,0.));
#28784=DIRECTION('ref_axis',(0.,0.,-1.));
#28785=DIRECTION('',(0.,-1.,0.));
#28786=DIRECTION('center_axis',(-1.,0.,0.));
#28787=DIRECTION('ref_axis',(0.,0.,-1.));
#28788=DIRECTION('center_axis',(-1.,0.,0.));
#28789=DIRECTION('ref_axis',(0.,0.,-1.));
#28790=DIRECTION('',(0.,1.,0.));
#28791=DIRECTION('center_axis',(1.,0.,0.));
#28792=DIRECTION('ref_axis',(0.,0.,-1.));
#28793=DIRECTION('center_axis',(0.,1.,1.020425574104E-15));
#28794=DIRECTION('ref_axis',(0.,-1.020425574104E-15,1.));
#28795=DIRECTION('',(-1.,0.,0.));
#28796=DIRECTION('',(-1.,0.,0.));
#28797=DIRECTION('center_axis',(-1.,0.,0.));
#28798=DIRECTION('ref_axis',(0.,0.,1.));
#28799=DIRECTION('',(-1.,0.,0.));
#28800=DIRECTION('center_axis',(0.,0.,1.));
#28801=DIRECTION('ref_axis',(1.,0.,0.));
#28802=DIRECTION('',(-1.,0.,0.));
#28803=DIRECTION('center_axis',(-1.,0.,0.));
#28804=DIRECTION('ref_axis',(0.,0.,1.));
#28805=DIRECTION('center_axis',(-1.,0.,0.));
#28806=DIRECTION('ref_axis',(0.,0.,1.));
#28807=DIRECTION('',(-1.,0.,0.));
#28808=DIRECTION('center_axis',(0.,0.,-1.));
#28809=DIRECTION('ref_axis',(-1.,0.,0.));
#28810=DIRECTION('',(-1.,0.,0.));
#28811=DIRECTION('center_axis',(-1.,0.,0.));
#28812=DIRECTION('ref_axis',(0.,0.,1.));
#28813=DIRECTION('',(-1.,0.,0.));
#28814=DIRECTION('center_axis',(0.,1.,-1.020425574104E-15));
#28815=DIRECTION('ref_axis',(0.,1.020425574104E-15,1.));
#28816=DIRECTION('',(-1.,0.,0.));
#28817=DIRECTION('center_axis',(0.,1.61730259095139E-16,1.));
#28818=DIRECTION('ref_axis',(0.,-1.,1.61730259095139E-16));
#28819=DIRECTION('center_axis',(0.,1.61730259095139E-16,-1.));
#28820=DIRECTION('ref_axis',(0.,1.,1.61730259095139E-16));
#28821=DIRECTION('',(-6.90253292068385E-31,-7.21247185085526E-31,1.));
#28822=DIRECTION('',(1.,-2.46519032881566E-32,6.90253292068385E-31));
#28823=DIRECTION('',(1.21430643318377E-16,1.09063073495804E-16,-1.));
#28824=DIRECTION('',(-1.,-6.54590493145539E-16,-1.21430643318377E-16));
#28825=DIRECTION('axis',(0.,0.,1.));
#28826=DIRECTION('refdir',(1.,0.,0.));
#28827=DIRECTION('center_axis',(0.,0.,1.));
#28828=DIRECTION('ref_axis',(1.,0.,0.));
#28829=DIRECTION('center_axis',(0.,0.,1.));
#28830=DIRECTION('ref_axis',(1.,0.,0.));
#28831=DIRECTION('',(0.,0.,1.));
#28832=DIRECTION('center_axis',(0.,0.,1.));
#28833=DIRECTION('ref_axis',(1.,0.,0.));
#28834=DIRECTION('center_axis',(0.,0.,1.));
#28835=DIRECTION('ref_axis',(1.,0.,0.));
#28836=DIRECTION('center_axis',(0.,0.,1.));
#28837=DIRECTION('ref_axis',(1.,0.,0.));
#28838=DIRECTION('',(0.,0.,1.));
#28839=DIRECTION('center_axis',(0.,0.,1.));
#28840=DIRECTION('ref_axis',(1.,0.,0.));
#28841=DIRECTION('center_axis',(0.,0.,1.));
#28842=DIRECTION('ref_axis',(1.,0.,0.));
#28843=DIRECTION('center_axis',(0.,0.,1.));
#28844=DIRECTION('ref_axis',(1.,0.,0.));
#28845=DIRECTION('',(0.,0.,1.));
#28846=DIRECTION('center_axis',(0.,0.,1.));
#28847=DIRECTION('ref_axis',(1.,0.,0.));
#28848=DIRECTION('center_axis',(0.,0.,1.));
#28849=DIRECTION('ref_axis',(1.,0.,0.));
#28850=DIRECTION('center_axis',(0.,0.,1.));
#28851=DIRECTION('ref_axis',(1.,0.,0.));
#28852=DIRECTION('',(0.,0.,1.));
#28853=DIRECTION('center_axis',(0.,0.,1.));
#28854=DIRECTION('ref_axis',(1.,0.,0.));
#28855=DIRECTION('center_axis',(0.,0.,1.));
#28856=DIRECTION('ref_axis',(1.,0.,0.));
#28857=DIRECTION('',(-4.08170229641602E-16,1.,0.));
#28858=DIRECTION('',(-1.,0.,0.));
#28859=DIRECTION('',(0.,1.,0.));
#28860=DIRECTION('',(-1.,0.,0.));
#28861=DIRECTION('center_axis',(-1.,0.,0.));
#28862=DIRECTION('ref_axis',(0.,0.,1.));
#28863=DIRECTION('',(0.,0.,1.));
#28864=DIRECTION('',(0.,1.,0.));
#28865=DIRECTION('',(0.,0.,-1.));
#28866=DIRECTION('',(0.,1.,0.));
#28867=DIRECTION('',(0.,0.,-1.));
#28868=DIRECTION('center_axis',(0.,-1.,0.));
#28869=DIRECTION('ref_axis',(0.,0.,-1.));
#28870=DIRECTION('',(-1.,0.,0.));
#28871=DIRECTION('',(0.,0.,1.));
#28872=DIRECTION('',(-1.,0.,0.));
#28873=DIRECTION('',(0.,0.,-1.));
#28874=DIRECTION('center_axis',(1.,0.,0.));
#28875=DIRECTION('ref_axis',(0.,0.,-1.));
#28876=DIRECTION('',(0.,-1.,0.));
#28877=DIRECTION('',(0.,0.,1.));
#28878=DIRECTION('',(0.,-1.,0.));
#28879=DIRECTION('',(0.,-1.,0.));
#28880=DIRECTION('',(0.,0.,-1.));
#28881=DIRECTION('center_axis',(0.,1.,0.));
#28882=DIRECTION('ref_axis',(0.,0.,1.));
#28883=DIRECTION('',(1.,-1.73472347597681E-16,0.));
#28884=DIRECTION('',(0.,0.,1.));
#28885=DIRECTION('',(1.,0.,0.));
#28886=DIRECTION('',(1.,0.,0.));
#28887=DIRECTION('center_axis',(0.,0.,1.));
#28888=DIRECTION('ref_axis',(1.,0.,0.));
#28889=DIRECTION('',(1.73472347597681E-15,-1.,0.));
#28890=DIRECTION('',(1.,0.,0.));
#28891=DIRECTION('center_axis',(0.,0.,1.));
#28892=DIRECTION('ref_axis',(1.,0.,0.));
#28893=DIRECTION('center_axis',(1.,4.08170229641602E-16,0.));
#28894=DIRECTION('ref_axis',(-4.08170229641602E-16,1.,0.));
#28895=DIRECTION('',(-4.08170229641602E-16,1.,0.));
#28896=DIRECTION('',(0.,0.,1.));
#28897=DIRECTION('center_axis',(0.,1.,0.));
#28898=DIRECTION('ref_axis',(0.,0.,1.));
#28899=DIRECTION('',(-1.,0.,0.));
#28900=DIRECTION('center_axis',(-1.,-1.73472347597681E-15,0.));
#28901=DIRECTION('ref_axis',(1.73472347597681E-15,-1.,0.));
#28902=DIRECTION('',(1.73472347597681E-15,-1.,0.));
#28903=DIRECTION('',(0.,0.,1.));
#28904=DIRECTION('center_axis',(0.,-1.,0.));
#28905=DIRECTION('ref_axis',(0.,0.,-1.));
#28906=DIRECTION('',(1.,0.,0.));
#28907=DIRECTION('center_axis',(0.,0.,1.));
#28908=DIRECTION('ref_axis',(1.,0.,0.));
#28909=DIRECTION('axis',(0.,0.,1.));
#28910=DIRECTION('refdir',(1.,0.,0.));
#28911=DIRECTION('center_axis',(0.,0.,1.));
#28912=DIRECTION('ref_axis',(1.,0.,0.));
#28913=DIRECTION('center_axis',(0.,0.,1.));
#28914=DIRECTION('ref_axis',(1.,0.,0.));
#28915=DIRECTION('',(0.,0.,1.));
#28916=DIRECTION('center_axis',(0.,0.,1.));
#28917=DIRECTION('ref_axis',(1.,0.,0.));
#28918=DIRECTION('center_axis',(0.,0.,1.));
#28919=DIRECTION('ref_axis',(1.,0.,0.));
#28920=DIRECTION('center_axis',(0.,0.,1.));
#28921=DIRECTION('ref_axis',(1.,0.,0.));
#28922=DIRECTION('',(0.,0.,1.));
#28923=DIRECTION('center_axis',(0.,0.,1.));
#28924=DIRECTION('ref_axis',(1.,0.,0.));
#28925=DIRECTION('center_axis',(0.,0.,1.));
#28926=DIRECTION('ref_axis',(1.,0.,0.));
#28927=DIRECTION('center_axis',(0.,0.,1.));
#28928=DIRECTION('ref_axis',(1.,0.,0.));
#28929=DIRECTION('',(0.,0.,1.));
#28930=DIRECTION('center_axis',(0.,0.,1.));
#28931=DIRECTION('ref_axis',(1.,0.,0.));
#28932=DIRECTION('center_axis',(0.,0.,1.));
#28933=DIRECTION('ref_axis',(1.,0.,0.));
#28934=DIRECTION('center_axis',(0.,0.,1.));
#28935=DIRECTION('ref_axis',(1.,0.,0.));
#28936=DIRECTION('',(0.,0.,1.));
#28937=DIRECTION('center_axis',(0.,0.,1.));
#28938=DIRECTION('ref_axis',(1.,0.,0.));
#28939=DIRECTION('center_axis',(0.,0.,1.));
#28940=DIRECTION('ref_axis',(1.,0.,0.));
#28941=DIRECTION('',(-5.33761069531325E-16,1.,0.));
#28942=DIRECTION('',(-1.,0.,0.));
#28943=DIRECTION('',(0.,1.,0.));
#28944=DIRECTION('',(-1.,0.,0.));
#28945=DIRECTION('center_axis',(-1.,0.,0.));
#28946=DIRECTION('ref_axis',(0.,0.,1.));
#28947=DIRECTION('',(0.,0.,1.));
#28948=DIRECTION('',(6.93889390390723E-16,1.,0.));
#28949=DIRECTION('',(0.,0.,-1.));
#28950=DIRECTION('',(0.,1.,0.));
#28951=DIRECTION('',(0.,0.,-1.));
#28952=DIRECTION('center_axis',(0.,-1.,0.));
#28953=DIRECTION('ref_axis',(0.,0.,-1.));
#28954=DIRECTION('',(-1.,0.,0.));
#28955=DIRECTION('',(0.,0.,1.));
#28956=DIRECTION('',(-1.,0.,0.));
#28957=DIRECTION('',(0.,0.,-1.));
#28958=DIRECTION('center_axis',(1.,0.,0.));
#28959=DIRECTION('ref_axis',(0.,0.,-1.));
#28960=DIRECTION('',(0.,-1.,0.));
#28961=DIRECTION('',(0.,0.,1.));
#28962=DIRECTION('',(0.,-1.,0.));
#28963=DIRECTION('',(0.,-1.,0.));
#28964=DIRECTION('',(0.,0.,-1.));
#28965=DIRECTION('center_axis',(0.,1.,0.));
#28966=DIRECTION('ref_axis',(0.,0.,1.));
#28967=DIRECTION('',(1.,-8.67361737988404E-17,0.));
#28968=DIRECTION('',(0.,0.,1.));
#28969=DIRECTION('',(1.,0.,0.));
#28970=DIRECTION('',(1.,0.,0.));
#28971=DIRECTION('center_axis',(0.,0.,1.));
#28972=DIRECTION('ref_axis',(1.,0.,0.));
#28973=DIRECTION('',(0.,-1.,0.));
#28974=DIRECTION('',(1.,0.,0.));
#28975=DIRECTION('center_axis',(0.,0.,1.));
#28976=DIRECTION('ref_axis',(1.,0.,0.));
#28977=DIRECTION('center_axis',(1.,5.33761069531325E-16,0.));
#28978=DIRECTION('ref_axis',(-5.33761069531325E-16,1.,0.));
#28979=DIRECTION('',(-5.33761069531325E-16,1.,0.));
#28980=DIRECTION('',(0.,0.,1.));
#28981=DIRECTION('center_axis',(0.,1.,0.));
#28982=DIRECTION('ref_axis',(0.,0.,1.));
#28983=DIRECTION('',(-1.,0.,0.));
#28984=DIRECTION('center_axis',(-1.,0.,0.));
#28985=DIRECTION('ref_axis',(0.,0.,1.));
#28986=DIRECTION('',(0.,-1.,0.));
#28987=DIRECTION('',(0.,0.,1.));
#28988=DIRECTION('center_axis',(0.,-1.,0.));
#28989=DIRECTION('ref_axis',(0.,0.,-1.));
#28990=DIRECTION('',(1.,0.,0.));
#28991=DIRECTION('center_axis',(0.,0.,1.));
#28992=DIRECTION('ref_axis',(1.,0.,0.));
#28993=DIRECTION('axis',(0.,0.,1.));
#28994=DIRECTION('refdir',(1.,0.,0.));
#28995=DIRECTION('center_axis',(0.,0.,1.));
#28996=DIRECTION('ref_axis',(1.,0.,0.));
#28997=DIRECTION('center_axis',(0.,0.,1.));
#28998=DIRECTION('ref_axis',(1.,0.,0.));
#28999=DIRECTION('',(0.,0.,1.));
#29000=DIRECTION('center_axis',(0.,0.,1.));
#29001=DIRECTION('ref_axis',(1.,0.,0.));
#29002=DIRECTION('center_axis',(0.,0.,1.));
#29003=DIRECTION('ref_axis',(1.,0.,0.));
#29004=DIRECTION('center_axis',(0.,0.,1.));
#29005=DIRECTION('ref_axis',(1.,0.,0.));
#29006=DIRECTION('',(0.,0.,1.));
#29007=DIRECTION('center_axis',(0.,0.,1.));
#29008=DIRECTION('ref_axis',(1.,0.,0.));
#29009=DIRECTION('center_axis',(0.,0.,1.));
#29010=DIRECTION('ref_axis',(1.,0.,0.));
#29011=DIRECTION('center_axis',(0.,0.,1.));
#29012=DIRECTION('ref_axis',(1.,0.,0.));
#29013=DIRECTION('',(0.,0.,1.));
#29014=DIRECTION('center_axis',(0.,0.,1.));
#29015=DIRECTION('ref_axis',(1.,0.,0.));
#29016=DIRECTION('center_axis',(0.,0.,1.));
#29017=DIRECTION('ref_axis',(1.,0.,0.));
#29018=DIRECTION('center_axis',(0.,0.,1.));
#29019=DIRECTION('ref_axis',(1.,0.,0.));
#29020=DIRECTION('',(0.,0.,1.));
#29021=DIRECTION('center_axis',(0.,0.,1.));
#29022=DIRECTION('ref_axis',(1.,0.,0.));
#29023=DIRECTION('center_axis',(0.,0.,1.));
#29024=DIRECTION('ref_axis',(1.,0.,0.));
#29025=DIRECTION('center_axis',(0.,0.,1.));
#29026=DIRECTION('ref_axis',(1.,0.,0.));
#29027=DIRECTION('',(0.,0.,1.));
#29028=DIRECTION('center_axis',(0.,0.,1.));
#29029=DIRECTION('ref_axis',(1.,0.,0.));
#29030=DIRECTION('center_axis',(0.,0.,1.));
#29031=DIRECTION('ref_axis',(1.,0.,0.));
#29032=DIRECTION('center_axis',(0.,0.,1.));
#29033=DIRECTION('ref_axis',(1.,0.,0.));
#29034=DIRECTION('',(0.,0.,1.));
#29035=DIRECTION('center_axis',(0.,0.,1.));
#29036=DIRECTION('ref_axis',(1.,0.,0.));
#29037=DIRECTION('center_axis',(0.,0.,1.));
#29038=DIRECTION('ref_axis',(1.,0.,0.));
#29039=DIRECTION('center_axis',(0.,0.,1.));
#29040=DIRECTION('ref_axis',(1.,0.,0.));
#29041=DIRECTION('',(0.,0.,1.));
#29042=DIRECTION('center_axis',(0.,0.,1.));
#29043=DIRECTION('ref_axis',(1.,0.,0.));
#29044=DIRECTION('center_axis',(0.,0.,1.));
#29045=DIRECTION('ref_axis',(1.,0.,0.));
#29046=DIRECTION('center_axis',(0.,0.,1.));
#29047=DIRECTION('ref_axis',(1.,0.,0.));
#29048=DIRECTION('',(0.,0.,1.));
#29049=DIRECTION('center_axis',(0.,0.,1.));
#29050=DIRECTION('ref_axis',(1.,0.,0.));
#29051=DIRECTION('center_axis',(0.,0.,1.));
#29052=DIRECTION('ref_axis',(1.,0.,0.));
#29053=DIRECTION('center_axis',(0.,0.,1.));
#29054=DIRECTION('ref_axis',(1.,0.,0.));
#29055=DIRECTION('',(0.,0.,1.));
#29056=DIRECTION('center_axis',(0.,0.,1.));
#29057=DIRECTION('ref_axis',(1.,0.,0.));
#29058=DIRECTION('center_axis',(0.,0.,1.));
#29059=DIRECTION('ref_axis',(1.,0.,0.));
#29060=DIRECTION('center_axis',(0.,0.,1.));
#29061=DIRECTION('ref_axis',(1.,0.,0.));
#29062=DIRECTION('',(0.,0.,1.));
#29063=DIRECTION('center_axis',(0.,0.,1.));
#29064=DIRECTION('ref_axis',(1.,0.,0.));
#29065=DIRECTION('center_axis',(0.,0.,1.));
#29066=DIRECTION('ref_axis',(1.,0.,0.));
#29067=DIRECTION('center_axis',(0.,0.,1.));
#29068=DIRECTION('ref_axis',(1.,0.,0.));
#29069=DIRECTION('',(0.,0.,1.));
#29070=DIRECTION('center_axis',(0.,0.,1.));
#29071=DIRECTION('ref_axis',(1.,0.,0.));
#29072=DIRECTION('center_axis',(0.,0.,1.));
#29073=DIRECTION('ref_axis',(1.,0.,0.));
#29074=DIRECTION('center_axis',(0.,0.,1.));
#29075=DIRECTION('ref_axis',(1.,0.,0.));
#29076=DIRECTION('',(0.,0.,1.));
#29077=DIRECTION('center_axis',(0.,0.,1.));
#29078=DIRECTION('ref_axis',(1.,0.,0.));
#29079=DIRECTION('center_axis',(0.,0.,-1.));
#29080=DIRECTION('ref_axis',(-1.,0.,0.));
#29081=DIRECTION('',(0.,1.,0.));
#29082=DIRECTION('',(-1.,0.,0.));
#29083=DIRECTION('',(0.,-1.,0.));
#29084=DIRECTION('',(1.,0.,0.));
#29085=DIRECTION('center_axis',(-1.,0.,0.));
#29086=DIRECTION('ref_axis',(0.,0.,1.));
#29087=DIRECTION('',(0.,1.,0.));
#29088=DIRECTION('',(0.,0.,-1.));
#29089=DIRECTION('',(0.,0.,-1.));
#29090=DIRECTION('center_axis',(0.,-1.,0.));
#29091=DIRECTION('ref_axis',(0.,0.,-1.));
#29092=DIRECTION('',(-1.,0.,0.));
#29093=DIRECTION('',(0.,0.,-1.));
#29094=DIRECTION('center_axis',(1.,0.,0.));
#29095=DIRECTION('ref_axis',(0.,0.,-1.));
#29096=DIRECTION('',(0.,-1.,0.));
#29097=DIRECTION('',(0.,0.,-1.));
#29098=DIRECTION('center_axis',(0.,1.,0.));
#29099=DIRECTION('ref_axis',(0.,0.,1.));
#29100=DIRECTION('',(1.,0.,0.));
#29101=DIRECTION('center_axis',(0.,0.,-1.));
#29102=DIRECTION('ref_axis',(-1.,0.,0.));
#29103=DIRECTION('center_axis',(0.,0.,1.));
#29104=DIRECTION('ref_axis',(1.,0.,0.));
#29105=DIRECTION('center_axis',(0.,0.,-1.));
#29106=DIRECTION('ref_axis',(-1.,0.,0.));
#29107=DIRECTION('center_axis',(0.,0.,-1.));
#29108=DIRECTION('ref_axis',(-1.,0.,0.));
#29109=DIRECTION('axis',(0.,0.,1.));
#29110=DIRECTION('refdir',(1.,0.,0.));
#29111=DIRECTION('axis',(0.,0.,1.));
#29112=DIRECTION('refdir',(1.,0.,0.));
#29113=DIRECTION('axis',(0.,0.,1.));
#29114=DIRECTION('refdir',(1.,0.,0.));
#29115=DIRECTION('center_axis',(-1.,0.,0.));
#29116=DIRECTION('ref_axis',(0.,0.,1.));
#29117=DIRECTION('center_axis',(-1.,0.,0.));
#29118=DIRECTION('ref_axis',(0.,1.,-7.80005689667481E-12));
#29119=DIRECTION('center_axis',(1.,0.,0.));
#29120=DIRECTION('ref_axis',(0.,-1.,7.80005689667481E-12));
#29121=DIRECTION('',(-1.,0.,0.));
#29122=DIRECTION('center_axis',(-1.,0.,0.));
#29123=DIRECTION('ref_axis',(0.,-1.,7.80005689667481E-12));
#29124=DIRECTION('center_axis',(-1.,0.,0.));
#29125=DIRECTION('ref_axis',(0.,0.866025403788329,0.499999999993262));
#29126=DIRECTION('center_axis',(1.,0.,0.));
#29127=DIRECTION('ref_axis',(0.,0.866025403788329,0.499999999993262));
#29128=DIRECTION('',(-1.,0.,0.));
#29129=DIRECTION('center_axis',(1.,0.,0.));
#29130=DIRECTION('ref_axis',(0.,-0.866025403788329,-0.499999999993262));
#29131=DIRECTION('center_axis',(-1.,0.,0.));
#29132=DIRECTION('ref_axis',(0.,0.,1.));
#29133=DIRECTION('center_axis',(-1.,0.,0.));
#29134=DIRECTION('ref_axis',(0.,0.499999999993262,-0.866025403788329));
#29135=DIRECTION('center_axis',(1.,0.,0.));
#29136=DIRECTION('ref_axis',(0.,-0.499999999993262,0.866025403788329));
#29137=DIRECTION('center_axis',(-1.,0.,0.));
#29138=DIRECTION('ref_axis',(0.,-0.499999999993262,0.866025403788329));
#29139=DIRECTION('',(-1.,0.,0.));
#29140=DIRECTION('center_axis',(-0.909343589801517,-0.351779907850729,0.222137642283841));
#29141=DIRECTION('ref_axis',(-0.184944722510291,0.820060785619066,0.541567869712958));
#29142=DIRECTION('center_axis',(0.909343589801493,0.351779907850753,-0.2221376422839));
#29143=DIRECTION('ref_axis',(-0.341106909868786,0.936079511754707,0.0860303650627931));
#29144=DIRECTION('center_axis',(-1.6864379156382E-6,0.0915162499593412,
-0.995803583037607));
#29145=DIRECTION('ref_axis',(-0.34113926666238,0.936068028098637,0.0860270161785332));
#29146=DIRECTION('center_axis',(-9.8391347151436E-16,-0.864344564896165,
0.502900062770387));
#29147=DIRECTION('ref_axis',(0.0165957593644498,0.502830803827501,0.864225528142572));
#29148=DIRECTION('center_axis',(0.872337072829626,0.488810663329849,0.00960035322651945));
#29149=DIRECTION('ref_axis',(0.357490239572424,-0.624340021233245,-0.69455040601595));
#29150=DIRECTION('center_axis',(-0.872337165983214,0.252719928315943,0.418521811470274));
#29151=DIRECTION('ref_axis',(-0.357492608063605,-0.913666211044819,-0.193424636421748));
#29152=DIRECTION('center_axis',(0.,-0.816631319604251,0.577159672743531));
#29153=DIRECTION('ref_axis',(1.,0.,0.));
#29154=DIRECTION('center_axis',(0.,0.0033519474796912,0.999994382208267));
#29155=DIRECTION('ref_axis',(1.,0.,0.));
#29156=DIRECTION('center_axis',(1.,2.42086419888004E-12,-4.76508631093348E-9));
#29157=DIRECTION('ref_axis',(4.76508363468576E-9,-0.00168336254192495,0.999998583144272));
#29158=DIRECTION('center_axis',(1.51830655795334E-16,0.0033519474626319,
-0.999994382208324));
#29159=DIRECTION('ref_axis',(-0.0165957593611889,0.999856663884339,0.00335148583545193));
#29160=DIRECTION('center_axis',(-3.10862446895044E-14,0.816631319604264,
-0.577159672743512));
#29161=DIRECTION('ref_axis',(0.818873283807973,0.33127484328694,0.468725424177909));
#29162=DIRECTION('center_axis',(-0.909343584374911,-0.016486906074352,0.415719169012309));
#29163=DIRECTION('ref_axis',(0.341106909670097,0.542544239120665,0.767653453566317));
#29164=DIRECTION('center_axis',(0.9093435898015,-0.0164868874227782,0.415719157881892));
#29165=DIRECTION('ref_axis',(0.0165957593541801,0.999856663884451,0.00335148583689117));
#29166=DIRECTION('center_axis',(-0.872334653160836,-0.252721554400087,-0.41852606709304));
#29167=DIRECTION('ref_axis',(0.357508978425797,-0.913652443783903,-0.193459407402805));
#29168=DIRECTION('center_axis',(1.15170725409523E-6,-0.816634222548046,
0.577155565304556));
#29169=DIRECTION('ref_axis',(-0.999999999666746,1.39449692278666E-5,2.17266316248917E-5));
#29170=DIRECTION('center_axis',(-0.909343589801518,0.0164868874227569,-0.415719157881855));
#29171=DIRECTION('ref_axis',(-0.184944722510292,0.879041925861211,0.439409538123383));
#29172=DIRECTION('center_axis',(-1.35716939467332E-15,0.00335194746035888,
-0.999994382208332));
#29173=DIRECTION('ref_axis',(-1.,-1.17865786493649E-10,-3.93724966170751E-13));
#29174=DIRECTION('center_axis',(0.872337121117555,0.252719440142821,-0.418522199762732));
#29175=DIRECTION('ref_axis',(0.357492026988926,-0.913666559888409,0.19342406256986));
#29176=DIRECTION('center_axis',(-1.68628111100734E-6,-0.81663307513297,
-0.577157188810835));
#29177=DIRECTION('ref_axis',(-0.341139266645681,0.542535595401582,-0.767645183971539));
#29178=DIRECTION('center_axis',(-0.909343589801519,0.0164868874292406,0.415719157881595));
#29179=DIRECTION('ref_axis',(-0.184944722510296,0.87904192585435,-0.439409538137107));
#29180=DIRECTION('center_axis',(0.909343589801544,-0.0164868874292662,-0.415719157881539));
#29181=DIRECTION('ref_axis',(-0.341106909868691,0.542544237518575,-0.76765345461036));
#29182=DIRECTION('center_axis',(-1.61391540184803E-16,0.00335194747587369,
0.99999438220828));
#29183=DIRECTION('ref_axis',(0.016595759364439,0.999856663884241,-0.00335148584869172));
#29184=DIRECTION('center_axis',(0.999995050428565,0.00314628644158368,3.89202510670605E-13));
#29185=DIRECTION('ref_axis',(5.29618892397034E-9,-1.68342965936362E-6,0.999999999998583));
#29186=DIRECTION('center_axis',(-0.909343590214608,-0.0164868860208534,
-0.415719157033859));
#29187=DIRECTION('ref_axis',(-0.0165957582094495,0.999856663906389,-0.00335148496028424));
#29188=DIRECTION('center_axis',(1.33226762954886E-14,-0.00335194747968279,
-0.999994382208267));
#29189=DIRECTION('ref_axis',(0.701214746224632,0.712946119051022,-0.00238977137213218));
#29190=DIRECTION('center_axis',(-1.72180181182493E-5,-0.816644232415063,
-0.577141401535839));
#29191=DIRECTION('ref_axis',(0.999999999425232,2.7958306584923E-6,-3.37893227556071E-5));
#29192=DIRECTION('center_axis',(0.872334424881579,-0.252721294015423,0.418526700125207));
#29193=DIRECTION('ref_axis',(-0.357509234129503,-0.913652180043168,0.193460180436447));
#29194=DIRECTION('center_axis',(-0.872337165908837,0.488810485061077,-0.00960097226811875));
#29195=DIRECTION('ref_axis',(-0.357492574939675,-0.624343693581199,0.694545902837521));
#29196=DIRECTION('center_axis',(0.,0.0915192788336707,0.995803304675057));
#29197=DIRECTION('ref_axis',(1.,0.,0.));
#29198=DIRECTION('center_axis',(0.,0.86769651237392,0.497094319434588));
#29199=DIRECTION('ref_axis',(1.,0.,0.));
#29200=DIRECTION('center_axis',(1.,-4.12985136017776E-9,-2.38437093081533E-9));
#29201=DIRECTION('ref_axis',(4.76873489842038E-9,0.8651823496475,0.501457377908064));
#29202=DIRECTION('center_axis',(5.42101086242752E-18,-0.864344564902831,
-0.502900062758931));
#29203=DIRECTION('ref_axis',(-0.0165957593611997,0.502830803816073,-0.864225528149283));
#29204=DIRECTION('center_axis',(-2.22044604925032E-15,-0.091519278833694,
-0.995803304675055));
#29205=DIRECTION('ref_axis',(0.818873283807975,0.571565546381172,-0.0525297178322415));
#29206=DIRECTION('center_axis',(-0.909343584373447,0.351779908167727,0.222137664002207));
#29207=DIRECTION('ref_axis',(0.341106909670685,0.9360795116516,-0.0860303669701453));
#29208=DIRECTION('center_axis',(0.909343589801524,0.351779907854156,0.222137642278383));
#29209=DIRECTION('ref_axis',(0.0165957593541706,0.502830803817422,-0.864225528148633));
#29210=DIRECTION('center_axis',(-0.872334659306141,-0.488814972476424,0.00960025291910624));
#29211=DIRECTION('ref_axis',(0.357509612665106,-0.624368160481923,0.694515138084452));
#29212=DIRECTION('center_axis',(1.15170339592403E-6,0.091514270219573,0.995803764978247));
#29213=DIRECTION('ref_axis',(-0.999999999666746,2.57883005308933E-5,-1.21338575712886E-6));
#29214=DIRECTION('center_axis',(-0.909343589801512,-0.351779907854202,-0.222137642278361));
#29215=DIRECTION('ref_axis',(-0.184944722510301,0.820060785610628,-0.541567869725733));
#29216=DIRECTION('center_axis',(-3.57959140632929E-17,-0.864344564903985,
-0.502900062756946));
#29217=DIRECTION('ref_axis',(-1.,-5.92716031326802E-11,1.01871380838448E-10));
#29218=DIRECTION('center_axis',(0.87233712123921,-0.236091136889651,-0.42812255487213));
#29219=DIRECTION('ref_axis',(0.357492075733543,-0.28932299193772,0.887970507462905));
#29220=DIRECTION('center_axis',(-1.68626957992325E-6,-0.908149325054355,
0.418646394228443));
#29221=DIRECTION('ref_axis',(-0.341139266648757,-0.393532432712662,-0.853672200059017));
#29222=DIRECTION('center_axis',(-0.909343589801511,0.368266795279956,0.193581515597778));
#29223=DIRECTION('ref_axis',(-0.1849447225103,0.0589811402353276,-0.980977407850012));
#29224=DIRECTION('center_axis',(0.909343589801499,-0.368266795279986,-0.193581515597776));
#29225=DIRECTION('ref_axis',(-0.341106909868806,-0.393535274236167,-0.853683819673079));
#29226=DIRECTION('center_axis',(2.71050543116904E-18,0.867696512372032,
0.497094319437884));
#29227=DIRECTION('ref_axis',(0.0165957593644693,0.497025860056731,-0.867577013991256));
#29228=DIRECTION('center_axis',(0.99999505042847,0.00157314323581978,-0.00272476401205455));
#29229=DIRECTION('ref_axis',(-1.62748491112573E-10,0.866025429650388,0.499999955198858));
#29230=DIRECTION('center_axis',(-0.909343590214268,-0.368266793842775,-0.193581516392936));
#29231=DIRECTION('ref_axis',(-0.0165957582102913,0.497025860836397,-0.867577013566671));
#29232=DIRECTION('center_axis',(0.,-0.867696512373919,-0.497094319434589));
#29233=DIRECTION('ref_axis',(0.701214746224636,0.354403456808009,-0.618624336313771));
#29234=DIRECTION('center_axis',(-1.72180195932569E-5,-0.908141231516168,
0.418663950351399));
#29235=DIRECTION('ref_axis',(0.999999999425232,-2.7864497681015E-5,-1.93159206798986E-5));
#29236=DIRECTION('center_axis',(0.872334413842153,0.236094117750599,0.428126427577455));
#29237=DIRECTION('ref_axis',(-0.35750837102373,-0.289287102352822,0.887975639902507));
#29238=DIRECTION('center_axis',(-0.872337161491928,0.236090560831439,-0.42812279052452));
#29239=DIRECTION('ref_axis',(-0.357491177692246,0.289326452437243,0.887969741484636));
#29240=DIRECTION('center_axis',(0.,0.908150598437932,0.418643631931534));
#29241=DIRECTION('ref_axis',(1.,0.,0.));
#29242=DIRECTION('center_axis',(0.,0.864344564894221,-0.502900062773729));
#29243=DIRECTION('ref_axis',(1.,0.,0.));
#29244=DIRECTION('center_axis',(1.,-4.13180676296342E-9,2.3882947650968E-9));
#29245=DIRECTION('ref_axis',(4.7723861707432E-9,0.866865647562842,-0.498541822794693));
#29246=DIRECTION('center_axis',(-4.54009659728305E-16,-0.867696512365431,
0.497094319449405));
#29247=DIRECTION('ref_axis',(-0.0165957593611997,-0.497025860068278,-0.867577013984703));
#29248=DIRECTION('center_axis',(-4.44089209850062E-15,-0.908150598437929,
-0.41864363193154));
#29249=DIRECTION('ref_axis',(0.818873283807975,0.24029070309425,-0.521255142010144));
#29250=DIRECTION('center_axis',(-0.909343584372254,0.368266814251329,-0.193581505010677));
#29251=DIRECTION('ref_axis',(0.341106909671091,0.393535272534209,-0.853683820536658));
#29252=DIRECTION('center_axis',(0.909343589801533,0.36826679527692,-0.19358151560345));
#29253=DIRECTION('ref_axis',(0.0165957593541802,-0.497025860067054,-0.867577013985539));
#29254=DIRECTION('center_axis',(-0.872335303813278,-0.236092825490624,0.428125326829481));
#29255=DIRECTION('ref_axis',(0.357518325797022,0.289256956575762,0.887981452391784));
#29256=DIRECTION('center_axis',(1.15182100555332E-6,0.908148492690305,0.41864819983251));
#29257=DIRECTION('ref_axis',(-0.999999999666752,1.18433208703558E-5,-2.29397212159883E-5));
#29258=DIRECTION('center_axis',(-0.90934358980152,-0.368266795276941,0.193581515603471));
#29259=DIRECTION('ref_axis',(-0.184944722510296,-0.0589811402505156,-0.9809774078491));
#29260=DIRECTION('center_axis',(-1.16345885865374E-15,-0.867696512364302,
0.497094319451376));
#29261=DIRECTION('ref_axis',(-1.,5.85957252551265E-11,1.02278664219265E-10));
#29262=DIRECTION('center_axis',(0.872337121208026,-0.488810576952673,-0.00960035528969041));
#29263=DIRECTION('ref_axis',(0.357492065497932,0.624343502497626,0.694546336823555));
#29264=DIRECTION('center_axis',(-1.68643573492616E-6,-0.0915162499578196,
0.995803583037746));
#29265=DIRECTION('ref_axis',(-0.341139266673693,-0.936068028094749,-0.086027016175985));
#29266=DIRECTION('center_axis',(-0.909343589801517,0.351779907850729,-0.222137642283841));
#29267=DIRECTION('ref_axis',(-0.184944722510291,-0.820060785619066,-0.541567869712958));
#29268=DIRECTION('center_axis',(0.909343589801493,-0.351779907850753,0.2221376422839));
#29269=DIRECTION('ref_axis',(-0.341106909868786,-0.936079511754707,-0.0860303650627931));
#29270=DIRECTION('center_axis',(-9.89334482376699E-16,0.864344564896165,
-0.502900062770387));
#29271=DIRECTION('ref_axis',(0.0165957593644802,-0.502830803827501,-0.864225528142571));
#29272=DIRECTION('center_axis',(0.999995050428028,-0.00157314330632356,
-0.00272476413353121));
#29273=DIRECTION('ref_axis',(-1.09147368725947E-8,0.866023669196806,-0.500003004381874));
#29274=DIRECTION('center_axis',(-0.909343590213997,-0.351779907820795,0.222137640642713));
#29275=DIRECTION('ref_axis',(-0.0165957582109795,-0.502830803070625,-0.864225528605093));
#29276=DIRECTION('center_axis',(-1.77635683939847E-14,-0.864344564894251,
0.502900062773677));
#29277=DIRECTION('ref_axis',(0.701214746224631,-0.358542662243024,-0.616234564941639));
#29278=DIRECTION('center_axis',(-1.72180172530394E-5,-0.0914969991021175,
0.995805351893053));
#29279=DIRECTION('ref_axis',(0.999999999425232,-3.06603499728098E-5,1.44733980403473E-5));
#29280=DIRECTION('center_axis',(0.872334418927631,0.488815412109119,0.00959971034899223));
#29281=DIRECTION('ref_axis',(-0.357508592704786,0.624366331201059,0.694517307635146));
#29282=DIRECTION('center_axis',(-0.872337088253931,-0.252719995041193,-0.418521933192315));
#29283=DIRECTION('ref_axis',(-0.357492387674659,0.913666486545701,0.19342374238419));
#29284=DIRECTION('center_axis',(0.,0.816631319604251,-0.577159672743531));
#29285=DIRECTION('ref_axis',(1.,0.,0.));
#29286=DIRECTION('center_axis',(0.,-0.00335194747960493,-0.999994382208267));
#29287=DIRECTION('ref_axis',(1.,0.,0.));
#29288=DIRECTION('center_axis',(1.,2.42058998900158E-12,4.77239700262987E-9));
#29289=DIRECTION('ref_axis',(4.77238616670059E-9,0.00168330521887406,-0.999998583240767));
#29290=DIRECTION('center_axis',(1.51830655795334E-16,-0.0033519474626319,
0.999994382208324));
#29291=DIRECTION('ref_axis',(-0.0165957593611889,-0.999856663884339,-0.00335148583545193));
#29292=DIRECTION('center_axis',(-3.10862446895044E-14,-0.816631319604264,
0.577159672743512));
#29293=DIRECTION('ref_axis',(0.818873283807973,-0.33127484328694,-0.468725424177909));
#29294=DIRECTION('center_axis',(-0.909343584372272,0.0164869060835493,-0.415719169017717));
#29295=DIRECTION('ref_axis',(0.341106909671091,-0.54254423911736,-0.767653453568212));
#29296=DIRECTION('center_axis',(0.9093435898015,0.016486887422769,-0.415719157881893));
#29297=DIRECTION('ref_axis',(0.01659575935417,-0.999856663884451,-0.00335148583689154));
#29298=DIRECTION('center_axis',(-0.872334977453413,0.2527212762883,0.418525559103105));
#29299=DIRECTION('ref_axis',(0.357507402186026,0.913653676946343,0.193456496361912));
#29300=DIRECTION('center_axis',(1.15166574883469E-6,0.816634222527976,-0.577155565332953));
#29301=DIRECTION('ref_axis',(-0.999999999666747,-1.3944963123932E-5,-2.172655107418E-5));
#29302=DIRECTION('center_axis',(-0.909343589801518,-0.0164868874227569,
0.415719157881854));
#29303=DIRECTION('ref_axis',(-0.184944722510291,-0.879041925861207,-0.439409538123392));
#29304=DIRECTION('center_axis',(3.05791507767584E-15,-0.00335194746035888,
0.999994382208332));
#29305=DIRECTION('ref_axis',(-1.,1.17874460205389E-10,3.98169149435635E-13));
#29306=DIRECTION('center_axis',(0.872336706091693,-0.252719795504182,0.418522850230927));
#29307=DIRECTION('ref_axis',(0.357487400579544,0.913671323189871,-0.193410112474378));
#29308=DIRECTION('center_axis',(-1.68617080662445E-6,0.816633075161264,
0.577157188770802));
#29309=DIRECTION('ref_axis',(-0.341139266540615,-0.542535595355228,0.767645184050991));
#29310=DIRECTION('center_axis',(-0.909343589801519,-0.0164868874292406,
-0.415719157881595));
#29311=DIRECTION('ref_axis',(-0.184944722510296,-0.87904192585435,0.439409538137107));
#29312=DIRECTION('center_axis',(0.909343589801512,0.0164868874292142,0.415719157881612));
#29313=DIRECTION('ref_axis',(-0.341106909868779,-0.542544237518574,0.767653454610322));
#29314=DIRECTION('center_axis',(-1.59898644615292E-16,-0.00335194747587375,
-0.99999438220828));
#29315=DIRECTION('ref_axis',(0.0165957593644498,-0.999856663884241,0.00335148584869178));
#29316=DIRECTION('center_axis',(0.999995050428519,-0.00314628645604584,
-3.89202510576123E-13));
#29317=DIRECTION('ref_axis',(5.29426700772326E-9,1.68281880237154E-6,-0.999999999998584));
#29318=DIRECTION('center_axis',(-0.909343590214001,0.0164868860229314,0.415719157035105));
#29319=DIRECTION('ref_axis',(-0.0165957582109798,-0.999856663906358,0.00335148496194759));
#29320=DIRECTION('center_axis',(1.33226762954886E-14,0.00335194747968279,
0.999994382208267));
#29321=DIRECTION('ref_axis',(0.701214746224632,-0.712946119051022,0.00238977137213218));
#29322=DIRECTION('center_axis',(-1.72180378594051E-5,0.816644232407161,
0.57714140154702));
#29323=DIRECTION('ref_axis',(0.999999999425228,-2.79588956264274E-6,3.37894403045313E-5));
#29324=DIRECTION('center_axis',(0.872334340382926,0.252721365861299,-0.418526832862464));
#29325=DIRECTION('ref_axis',(-0.357509057710921,0.913652418969074,-0.193459378078731));
#29326=DIRECTION('center_axis',(-1.33226762954919E-14,0.86434456489425,
-0.502900062773679));
#29327=DIRECTION('ref_axis',(0.701214746224629,0.35854266224302,0.616234564941643));
#29328=DIRECTION('center_axis',(0.,-0.864344564894221,0.502900062773729));
#29329=DIRECTION('ref_axis',(1.,0.,0.));
#29330=DIRECTION('center_axis',(-1.7218016834779E-5,0.0914969991024323,
-0.995805351893024));
#29331=DIRECTION('ref_axis',(0.999999999425232,3.06603442363514E-5,-1.44733981459298E-5));
#29332=DIRECTION('center_axis',(-0.909343590214593,0.351779907820795,-0.222137640640273));
#29333=DIRECTION('ref_axis',(-0.0165957582094507,0.502830803069125,0.864225528605995));
#29334=DIRECTION('center_axis',(1.,4.212129460891E-9,-2.43187398740037E-9));
#29335=DIRECTION('ref_axis',(4.86374121739737E-9,-0.866866002087437,0.498541206346019));
#29336=DIRECTION('center_axis',(-4.54009659728305E-16,0.867696512365431,
-0.497094319449405));
#29337=DIRECTION('ref_axis',(-0.0165957593611997,0.497025860068278,0.867577013984703));
#29338=DIRECTION('center_axis',(-4.44089209850062E-15,0.908150598437929,
0.41864363193154));
#29339=DIRECTION('ref_axis',(0.818873283807975,-0.24029070309425,0.521255142010144));
#29340=DIRECTION('center_axis',(0.,-0.908150598437932,-0.418643631931534));
#29341=DIRECTION('ref_axis',(1.,0.,0.));
#29342=DIRECTION('center_axis',(-0.90934358437491,-0.368266814242001,0.193581505015946));
#29343=DIRECTION('ref_axis',(0.341106909670097,-0.393535272530976,0.853683820538545));
#29344=DIRECTION('center_axis',(-0.872337165954994,-0.23609055663585,0.428122783744317));
#29345=DIRECTION('ref_axis',(-0.357492608396839,-0.289322455852271,-0.887970467685291));
#29346=DIRECTION('center_axis',(-0.872334654387134,0.236093427908942,-0.428126317870655));
#29347=DIRECTION('ref_axis',(0.357509141512415,-0.28928500211756,-0.887976013913044));
#29348=DIRECTION('center_axis',(0.9093435898015,-0.368266795276978,0.193581515603494));
#29349=DIRECTION('ref_axis',(0.0165957593541708,0.497025860067054,0.867577013985539));
#29350=DIRECTION('center_axis',(-0.90934358980152,0.368266795276941,-0.193581515603471));
#29351=DIRECTION('ref_axis',(-0.184944722510296,0.0589811402505156,0.9809774078491));
#29352=DIRECTION('center_axis',(2.04681325985981E-15,0.867696512364302,
-0.497094319451376));
#29353=DIRECTION('ref_axis',(-1.,-5.85977525160398E-11,-1.02288660952578E-10));
#29354=DIRECTION('center_axis',(1.15181146809394E-6,-0.908148492693187,
-0.418648199826257));
#29355=DIRECTION('ref_axis',(-0.999999999666753,-1.18433108705755E-5,2.29397223096969E-5));
#29356=DIRECTION('center_axis',(-0.87233721909546,-0.488810390102957,0.00960097433567008));
#29357=DIRECTION('ref_axis',(-0.35749205135526,0.624342897076992,-0.69454688832887));
#29358=DIRECTION('center_axis',(0.,-0.0915192788337281,-0.995803304675052));
#29359=DIRECTION('ref_axis',(1.,0.,0.));
#29360=DIRECTION('center_axis',(0.,-0.86769651237392,-0.497094319434588));
#29361=DIRECTION('ref_axis',(1.,0.,0.));
#29362=DIRECTION('center_axis',(1.,4.22162271441645E-9,2.43735514986856E-9));
#29363=DIRECTION('ref_axis',(4.87470318552635E-9,-0.865182573208305,-0.501456992190413));
#29364=DIRECTION('center_axis',(1.35525271560688E-18,0.864344564902831,
0.502900062758931));
#29365=DIRECTION('ref_axis',(-0.016595759361191,-0.502830803816073,0.864225528149283));
#29366=DIRECTION('center_axis',(-2.22044604925032E-15,0.091519278833694,
0.995803304675055));
#29367=DIRECTION('ref_axis',(0.818873283807975,-0.571565546381172,0.0525297178322415));
#29368=DIRECTION('center_axis',(-0.909343584370803,-0.351779908167854,-0.222137664012828));
#29369=DIRECTION('ref_axis',(0.341106909671707,-0.936079511651572,0.0860303669663984));
#29370=DIRECTION('center_axis',(0.909343589801524,-0.351779907854152,-0.222137642278389));
#29371=DIRECTION('ref_axis',(0.0165957593541805,-0.502830803817418,0.864225528148635));
#29372=DIRECTION('center_axis',(-0.872335148377002,0.488814099296658,-0.00960027264571843));
#29373=DIRECTION('ref_axis',(0.357508508680803,0.624367614508793,-0.694516197200201));
#29374=DIRECTION('center_axis',(1.15179046766159E-6,-0.0915142700473301,
-0.995803764994076));
#29375=DIRECTION('ref_axis',(-0.999999999666754,-2.57879850815794E-5,1.21326932795859E-6));
#29376=DIRECTION('center_axis',(-0.909343589801512,0.351779907854202,0.222137642278361));
#29377=DIRECTION('ref_axis',(-0.184944722510301,-0.820060785610628,0.541567869725733));
#29378=DIRECTION('center_axis',(-2.59499130955602E-17,0.864344564903985,
0.502900062756946));
#29379=DIRECTION('ref_axis',(-1.,5.92813457518923E-11,-1.0188810609777E-10));
#29380=DIRECTION('center_axis',(0.872337163237809,0.236091097930777,0.428122490780446));
#29381=DIRECTION('ref_axis',(0.357491458240221,0.289324548017128,-0.887970249051152));
#29382=DIRECTION('center_axis',(-1.68635658201456E-6,0.908149325052148,
-0.418646394233229));
#29383=DIRECTION('ref_axis',(-0.341139266558313,0.393532432703947,0.853672200099177));
#29384=DIRECTION('center_axis',(-0.909343589801511,-0.368266795279956,-0.193581515597778));
#29385=DIRECTION('ref_axis',(-0.1849447225103,-0.0589811402353276,0.980977407850012));
#29386=DIRECTION('center_axis',(0.909343589801501,0.368266795279979,0.19358151559778));
#29387=DIRECTION('ref_axis',(-0.341106909868806,0.393535274236167,0.853683819673079));
#29388=DIRECTION('center_axis',(1.35525271558452E-18,-0.867696512372032,
-0.497094319437884));
#29389=DIRECTION('ref_axis',(0.0165957593644498,-0.497025860056731,0.867577013991256));
#29390=DIRECTION('center_axis',(0.999995050428592,-0.00157314321649704,
0.00272476397858654));
#29391=DIRECTION('ref_axis',(4.67404295639049E-10,-0.866025329508561,-0.500000128649572));
#29392=DIRECTION('center_axis',(-0.909343590213624,0.368266793844967,0.19358151639179));
#29393=DIRECTION('ref_axis',(-0.0165957582118193,-0.497025860834913,0.867577013567492));
#29394=DIRECTION('center_axis',(0.,0.867696512373919,0.497094319434589));
#29395=DIRECTION('ref_axis',(0.701214746224636,-0.354403456808009,0.618624336313771));
#29396=DIRECTION('center_axis',(-1.7218041121248E-5,0.908141231519907,-0.418663950343286));
#29397=DIRECTION('ref_axis',(0.999999999425228,2.78645745094749E-5,1.93160359156296E-5));
#29398=DIRECTION('center_axis',(0.872334911744233,-0.236093655852982,-0.428125667787106));
#29399=DIRECTION('ref_axis',(-0.357507870022192,0.289286581381741,-0.887976011334012));
#29400=DIRECTION('center_axis',(1.,0.,0.));
#29401=DIRECTION('ref_axis',(0.,0.981895700022487,0.189422370055255));
#29402=DIRECTION('center_axis',(-1.,0.,0.));
#29403=DIRECTION('ref_axis',(0.,0.654992470158046,0.755635404170729));
#29404=DIRECTION('center_axis',(1.,0.,0.));
#29405=DIRECTION('ref_axis',(0.,0.654992434517533,-0.755635435064288));
#29406=DIRECTION('center_axis',(-1.,0.,0.));
#29407=DIRECTION('ref_axis',(0.,0.981895710396792,-0.189422316278677));
#29408=DIRECTION('center_axis',(1.,0.,0.));
#29409=DIRECTION('ref_axis',(0.,-0.326903271294508,-0.945057803108862));
#29410=DIRECTION('center_axis',(-1.,0.,0.));
#29411=DIRECTION('ref_axis',(0.,0.326903317255781,-0.945057787210479));
#29412=DIRECTION('center_axis',(1.,0.,0.));
#29413=DIRECTION('ref_axis',(0.,-0.981895688630785,-0.189422429105626));
#29414=DIRECTION('center_axis',(-1.,0.,0.));
#29415=DIRECTION('ref_axis',(0.,-0.65499239314391,-0.75563547092736));
#29416=DIRECTION('center_axis',(1.,0.,0.));
#29417=DIRECTION('ref_axis',(0.,-0.654992632839938,0.755635263156376));
#29418=DIRECTION('center_axis',(-1.,0.,0.));
#29419=DIRECTION('ref_axis',(0.,-0.981896389769016,0.189418794628653));
#29420=DIRECTION('center_axis',(1.,0.,0.));
#29421=DIRECTION('ref_axis',(0.,0.32690326548914,0.945057805116987));
#29422=DIRECTION('center_axis',(-1.,0.,0.));
#29423=DIRECTION('ref_axis',(0.,-0.32690305834171,0.945057876770961));
#29424=DIRECTION('center_axis',(-1.,0.,0.));
#29425=DIRECTION('ref_axis',(0.,0.,1.));
#29426=DIRECTION('center_axis',(-1.,0.,0.));
#29427=DIRECTION('ref_axis',(0.,0.500000000006722,0.866025403780558));
#29428=DIRECTION('center_axis',(1.,0.,0.));
#29429=DIRECTION('ref_axis',(0.,-0.500000000006722,-0.866025403780558));
#29430=DIRECTION('center_axis',(-1.,0.,0.));
#29431=DIRECTION('ref_axis',(0.,-0.500000000006722,-0.866025403780558));
#29432=DIRECTION('',(-1.,0.,0.));
#29433=DIRECTION('center_axis',(-1.,0.,0.));
#29434=DIRECTION('ref_axis',(0.,0.,1.));
#29435=DIRECTION('center_axis',(-1.,0.,0.));
#29436=DIRECTION('ref_axis',(0.,-1.,7.80005689667481E-12));
#29437=DIRECTION('center_axis',(1.,0.,0.));
#29438=DIRECTION('ref_axis',(0.,1.,-7.80005689667481E-12));
#29439=DIRECTION('center_axis',(-1.,0.,0.));
#29440=DIRECTION('ref_axis',(0.,1.,-7.80005689667481E-12));
#29441=DIRECTION('',(-1.,0.,0.));
#29442=DIRECTION('center_axis',(1.,0.,0.));
#29443=DIRECTION('ref_axis',(0.,1.,0.));
#29444=DIRECTION('center_axis',(0.999995050427998,0.00157314331111629,0.00272476414181539));
#29445=DIRECTION('ref_axis',(-1.20457054480573E-8,-0.866023489464513,0.500003315684714));
#29446=DIRECTION('center_axis',(0.872335130168889,-0.488814142273061,-0.00959973890682644));
#29447=DIRECTION('ref_axis',(-0.357518018969466,-0.624385691970657,-0.694495049496015));
#29448=DIRECTION('center_axis',(-1.,0.,0.));
#29449=DIRECTION('ref_axis',(0.,0.,1.));
#29450=DIRECTION('center_axis',(-1.,0.,0.));
#29451=DIRECTION('ref_axis',(0.,-0.499999999993262,0.866025403788329));
#29452=DIRECTION('center_axis',(1.,0.,0.));
#29453=DIRECTION('ref_axis',(0.,0.499999999993262,-0.866025403788329));
#29454=DIRECTION('',(-1.,0.,0.));
#29455=DIRECTION('center_axis',(-1.,0.,0.));
#29456=DIRECTION('ref_axis',(0.,0.499999999993262,-0.866025403788329));
#29457=DIRECTION('center_axis',(-1.,0.,0.));
#29458=DIRECTION('ref_axis',(0.,0.,1.));
#29459=DIRECTION('center_axis',(-1.,0.,0.));
#29460=DIRECTION('ref_axis',(0.,-0.500000000006722,-0.866025403780558));
#29461=DIRECTION('center_axis',(1.,0.,0.));
#29462=DIRECTION('ref_axis',(0.,0.500000000006722,0.866025403780558));
#29463=DIRECTION('',(-1.,0.,0.));
#29464=DIRECTION('center_axis',(-1.,0.,0.));
#29465=DIRECTION('ref_axis',(0.,0.500000000006722,0.866025403780558));
#29466=DIRECTION('center_axis',(1.,0.,0.));
#29467=DIRECTION('ref_axis',(0.,1.,0.));
#29468=DIRECTION('axis',(0.,0.,1.));
#29469=DIRECTION('refdir',(1.,0.,0.));
#29470=DIRECTION('center_axis',(0.,0.,1.));
#29471=DIRECTION('ref_axis',(1.,0.,0.));
#29472=DIRECTION('center_axis',(0.,0.,1.));
#29473=DIRECTION('ref_axis',(-1.,0.,0.));
#29474=DIRECTION('',(-0.866025403761798,0.500000000039214,0.));
#29475=DIRECTION('',(0.,1.,0.));
#29476=DIRECTION('',(0.866025403761798,0.500000000039214,0.));
#29477=DIRECTION('',(0.866025403761798,-0.500000000039214,0.));
#29478=DIRECTION('',(0.,-1.,0.));
#29479=DIRECTION('',(-0.866025403761798,-0.500000000039214,0.));
#29480=DIRECTION('center_axis',(0.,0.,-1.));
#29481=DIRECTION('ref_axis',(0.,-1.,0.));
#29482=DIRECTION('center_axis',(0.,0.,-1.));
#29483=DIRECTION('ref_axis',(-1.,0.,0.));
#29484=DIRECTION('center_axis',(0.,0.,1.));
#29485=DIRECTION('ref_axis',(-1.,0.,0.));
#29486=DIRECTION('',(0.,0.,-1.));
#29487=DIRECTION('center_axis',(0.,0.,-1.));
#29488=DIRECTION('ref_axis',(0.,-1.,0.));
#29489=DIRECTION('',(-0.866025403761798,-0.500000000039214,0.));
#29490=DIRECTION('',(0.,-1.,0.));
#29491=DIRECTION('',(0.866025403761798,-0.500000000039214,0.));
#29492=DIRECTION('',(0.866025403761798,0.500000000039214,0.));
#29493=DIRECTION('',(0.,1.,0.));
#29494=DIRECTION('',(-0.866025403761798,0.500000000039214,0.));
#29495=DIRECTION('center_axis',(0.500000000039214,-0.866025403761798,0.));
#29496=DIRECTION('ref_axis',(0.,0.,-1.));
#29497=DIRECTION('',(0.,0.,1.));
#29498=DIRECTION('',(0.,0.,1.));
#29499=DIRECTION('center_axis',(1.,0.,0.));
#29500=DIRECTION('ref_axis',(0.,1.,0.));
#29501=DIRECTION('',(0.,0.,1.));
#29502=DIRECTION('center_axis',(0.500000000039214,0.866025403761798,0.));
#29503=DIRECTION('ref_axis',(0.,0.,-1.));
#29504=DIRECTION('',(0.,0.,1.));
#29505=DIRECTION('center_axis',(-0.500000000039214,0.866025403761798,0.));
#29506=DIRECTION('ref_axis',(0.,0.,1.));
#29507=DIRECTION('',(0.,0.,1.));
#29508=DIRECTION('center_axis',(-1.,0.,0.));
#29509=DIRECTION('ref_axis',(0.,0.,1.));
#29510=DIRECTION('',(0.,0.,1.));
#29511=DIRECTION('center_axis',(-0.500000000039214,-0.866025403761798,0.));
#29512=DIRECTION('ref_axis',(-0.866025403761798,0.500000000039214,0.));
#29513=DIRECTION('axis',(0.,0.,1.));
#29514=DIRECTION('refdir',(1.,0.,0.));
#29515=DIRECTION('center_axis',(-1.,0.,0.));
#29516=DIRECTION('ref_axis',(0.,0.,1.));
#29517=DIRECTION('center_axis',(1.,0.,0.));
#29518=DIRECTION('ref_axis',(0.,-0.499999999993262,0.866025403788329));
#29519=DIRECTION('center_axis',(1.,0.,0.));
#29520=DIRECTION('ref_axis',(0.,0.,-1.));
#29521=DIRECTION('center_axis',(1.,0.,0.));
#29522=DIRECTION('ref_axis',(0.,1.,0.));
#29523=DIRECTION('center_axis',(1.,0.,0.));
#29524=DIRECTION('ref_axis',(0.,0.,1.));
#29525=DIRECTION('center_axis',(1.,0.,0.));
#29526=DIRECTION('ref_axis',(0.,1.,0.));
#29527=DIRECTION('center_axis',(1.,0.,0.));
#29528=DIRECTION('ref_axis',(0.,0.,-1.));
#29529=DIRECTION('',(0.,0.,-1.));
#29530=DIRECTION('center_axis',(-1.,0.,0.));
#29531=DIRECTION('ref_axis',(0.,0.,-1.));
#29532=DIRECTION('',(0.,0.,1.));
#29533=DIRECTION('',(0.,1.,0.));
#29534=DIRECTION('center_axis',(-1.,0.,0.));
#29535=DIRECTION('ref_axis',(0.,0.,-1.));
#29536=DIRECTION('center_axis',(1.,0.,0.));
#29537=DIRECTION('ref_axis',(0.,0.,-1.));
#29538=DIRECTION('',(0.707106781186548,-8.65956056235493E-17,-0.707106781186547));
#29539=DIRECTION('center_axis',(1.,0.,0.));
#29540=DIRECTION('ref_axis',(0.,0.,-1.));
#29541=DIRECTION('',(1.,0.,0.));
#29542=DIRECTION('',(-1.,0.,0.));
#29543=DIRECTION('center_axis',(1.,0.,0.));
#29544=DIRECTION('ref_axis',(0.,0.,-1.));
#29545=DIRECTION('center_axis',(-1.,0.,0.));
#29546=DIRECTION('ref_axis',(0.,0.,1.));
#29547=DIRECTION('center_axis',(1.,0.,0.));
#29548=DIRECTION('ref_axis',(0.,1.,0.));
#29549=DIRECTION('center_axis',(1.,0.,0.));
#29550=DIRECTION('ref_axis',(0.,0.,-1.));
#29551=DIRECTION('center_axis',(1.,0.,0.));
#29552=DIRECTION('ref_axis',(0.,-0.499999999993262,-0.866025403788329));
#29553=DIRECTION('center_axis',(1.,0.,0.));
#29554=DIRECTION('ref_axis',(0.,0.,1.));
#29555=DIRECTION('center_axis',(-1.,0.,0.));
#29556=DIRECTION('ref_axis',(0.,0.,1.));
#29557=DIRECTION('center_axis',(1.,0.,0.));
#29558=DIRECTION('ref_axis',(0.,-0.499999999993262,0.866025403788329));
#29559=DIRECTION('center_axis',(1.,0.,0.));
#29560=DIRECTION('ref_axis',(0.,0.,1.));
#29561=DIRECTION('center_axis',(1.,0.,0.));
#29562=DIRECTION('ref_axis',(0.,-0.499999999993262,-0.866025403788329));
#29563=DIRECTION('center_axis',(1.,0.,0.));
#29564=DIRECTION('ref_axis',(0.,0.,-1.));
#29565=DIRECTION('center_axis',(-1.,0.,0.));
#29566=DIRECTION('ref_axis',(0.,-0.499999999993262,0.866025403788329));
#29567=DIRECTION('center_axis',(1.,0.,0.));
#29568=DIRECTION('ref_axis',(0.,-0.499999999993262,0.866025403788329));
#29569=DIRECTION('',(1.,0.,0.));
#29570=DIRECTION('',(-1.,0.,0.));
#29571=DIRECTION('center_axis',(-1.,0.,0.));
#29572=DIRECTION('ref_axis',(0.,1.22464679914735E-16,-1.));
#29573=DIRECTION('',(1.,0.,0.));
#29574=DIRECTION('center_axis',(1.,0.,0.));
#29575=DIRECTION('ref_axis',(0.,0.,1.));
#29576=DIRECTION('',(-1.,0.,0.));
#29577=DIRECTION('center_axis',(-1.,0.,0.));
#29578=DIRECTION('ref_axis',(0.,0.,1.));
#29579=DIRECTION('',(1.,0.,0.));
#29580=DIRECTION('center_axis',(1.,0.,0.));
#29581=DIRECTION('ref_axis',(0.,0.,1.));
#29582=DIRECTION('',(-1.,0.,0.));
#29583=DIRECTION('center_axis',(-1.,0.,0.));
#29584=DIRECTION('ref_axis',(0.,0.,1.));
#29585=DIRECTION('',(1.,0.,0.));
#29586=DIRECTION('center_axis',(1.,0.,0.));
#29587=DIRECTION('ref_axis',(0.,0.,1.));
#29588=DIRECTION('center_axis',(-1.,0.,0.));
#29589=DIRECTION('ref_axis',(0.,0.17575598334211,0.98443376329718));
#29590=DIRECTION('',(-1.,0.,0.));
#29591=DIRECTION('center_axis',(1.,0.,0.));
#29592=DIRECTION('ref_axis',(0.,-0.499999999993262,-0.866025403788329));
#29593=DIRECTION('center_axis',(-1.,0.,0.));
#29594=DIRECTION('ref_axis',(0.,-0.499999999993262,-0.866025403788329));
#29595=DIRECTION('center_axis',(1.,0.,0.));
#29596=DIRECTION('ref_axis',(0.,-0.499999999993262,-0.866025403788329));
#29597=DIRECTION('',(1.,0.,0.));
#29598=DIRECTION('center_axis',(1.,0.,0.));
#29599=DIRECTION('ref_axis',(0.,1.,0.));
#29600=DIRECTION('center_axis',(1.,0.,0.));
#29601=DIRECTION('ref_axis',(0.,0.,-1.));
#29602=DIRECTION('center_axis',(1.,0.,0.));
#29603=DIRECTION('ref_axis',(0.,1.,0.));
#29604=DIRECTION('center_axis',(1.,0.,0.));
#29605=DIRECTION('ref_axis',(0.,0.,-1.));
#29606=DIRECTION('center_axis',(1.,0.,0.));
#29607=DIRECTION('ref_axis',(0.,0.,-1.));
#29608=DIRECTION('center_axis',(1.,0.,0.));
#29609=DIRECTION('ref_axis',(0.,1.,0.));
#29610=DIRECTION('center_axis',(1.,0.,0.));
#29611=DIRECTION('ref_axis',(0.,0.,-1.));
#29612=DIRECTION('center_axis',(1.,0.,0.));
#29613=DIRECTION('ref_axis',(0.,-0.499999999993262,0.866025403788329));
#29614=DIRECTION('',(0.,0.,1.));
#29615=DIRECTION('',(0.,-1.,0.));
#29616=DIRECTION('',(0.,0.,-1.));
#29617=DIRECTION('center_axis',(1.,0.,0.));
#29618=DIRECTION('ref_axis',(0.,0.,-1.));
#29619=DIRECTION('center_axis',(-1.,0.,0.));
#29620=DIRECTION('ref_axis',(0.,-0.94042263903113,-0.340007735202781));
#29621=DIRECTION('',(-1.,0.,0.));
#29622=DIRECTION('center_axis',(-1.,0.,0.));
#29623=DIRECTION('ref_axis',(0.,1.,0.));
#29624=DIRECTION('',(1.,0.,0.));
#29625=DIRECTION('center_axis',(-1.,0.,0.));
#29626=DIRECTION('ref_axis',(0.,0.764666655685446,-0.644426028092314));
#29627=DIRECTION('',(-1.,0.,0.));
#29628=DIRECTION('center_axis',(1.,0.,0.));
#29629=DIRECTION('ref_axis',(0.,0.,-1.));
#29630=DIRECTION('',(-1.,0.,0.));
#29631=DIRECTION('',(1.,0.,0.));
#29632=DIRECTION('center_axis',(0.,0.,1.));
#29633=DIRECTION('ref_axis',(1.,0.,0.));
#29634=DIRECTION('',(-1.,0.,0.));
#29635=DIRECTION('',(1.,0.,0.));
#29636=DIRECTION('center_axis',(0.,0.,-1.));
#29637=DIRECTION('ref_axis',(-1.,0.,0.));
#29638=DIRECTION('center_axis',(0.,-1.,0.));
#29639=DIRECTION('ref_axis',(0.,0.,-1.));
#29640=DIRECTION('center_axis',(0.,1.,0.));
#29641=DIRECTION('ref_axis',(1.,0.,0.));
#29642=DIRECTION('center_axis',(0.,0.,1.));
#29643=DIRECTION('ref_axis',(-1.,0.,0.));
#29644=DIRECTION('',(0.,0.,1.));
#29645=DIRECTION('center_axis',(1.,0.,0.));
#29646=DIRECTION('ref_axis',(0.,0.,-1.));
#29647=DIRECTION('',(-1.,0.,0.));
#29648=DIRECTION('',(-1.,0.,0.));
#29649=DIRECTION('center_axis',(0.946028810149232,-0.324082536350894,7.74377105026033E-10));
#29650=DIRECTION('ref_axis',(0.0328036819517733,0.0957571728004204,-0.994864052173802));
#29651=DIRECTION('',(-1.,0.,0.));
#29652=DIRECTION('center_axis',(-0.94602881016076,0.324082536317243,7.10771293430115E-14));
#29653=DIRECTION('ref_axis',(0.0103965438556825,0.03034853443635,-0.999485306712121));
#29654=DIRECTION('',(-1.,0.,0.));
#29655=DIRECTION('center_axis',(1.,0.,0.));
#29656=DIRECTION('ref_axis',(0.,0.,-1.));
#29657=DIRECTION('',(-1.,0.,0.));
#29658=DIRECTION('center_axis',(-1.,0.,0.));
#29659=DIRECTION('ref_axis',(0.,0.,-1.));
#29660=DIRECTION('',(1.,0.,0.));
#29661=DIRECTION('center_axis',(1.,0.,0.));
#29662=DIRECTION('ref_axis',(0.,0.,-1.));
#29663=DIRECTION('',(-1.,0.,0.));
#29664=DIRECTION('center_axis',(-1.,0.,0.));
#29665=DIRECTION('ref_axis',(0.,0.,-1.));
#29666=DIRECTION('',(-1.,0.,0.));
#29667=DIRECTION('center_axis',(-1.,0.,0.));
#29668=DIRECTION('ref_axis',(0.,0.,-1.));
#29669=DIRECTION('',(1.,0.,0.));
#29670=DIRECTION('center_axis',(1.,0.,0.));
#29671=DIRECTION('ref_axis',(0.,0.,-1.));
#29672=DIRECTION('',(-1.,0.,0.));
#29673=DIRECTION('',(1.,0.,0.));
#29674=DIRECTION('center_axis',(0.50000000001139,-0.866025403777863,5.6567377117582E-14));
#29675=DIRECTION('ref_axis',(0.866025403777863,0.50000000001139,-7.49337626227376E-11));
#29676=DIRECTION('center_axis',(-0.500000000011408,-0.866025403777852,-1.85864239100662E-13));
#29677=DIRECTION('ref_axis',(0.866025403777852,-0.500000000011408,-4.16431008826601E-10));
#29678=DIRECTION('',(1.,0.,0.));
#29679=DIRECTION('center_axis',(0.500000000001134,0.866025403783784,-5.52352953831563E-15));
#29680=DIRECTION('ref_axis',(0.866025403783784,-0.500000000001134,-1.60186152837855E-11));
#29681=DIRECTION('center_axis',(-0.500000000001135,0.866025403783783,5.52352953831541E-15));
#29682=DIRECTION('ref_axis',(0.866025403783783,0.500000000001135,-3.15235664736174E-11));
#29683=DIRECTION('center_axis',(-0.855183382509445,0.518325556267202,0.));
#29684=DIRECTION('ref_axis',(0.518325556267202,0.855183382509445,0.));
#29685=DIRECTION('',(-1.,0.,0.));
#29686=DIRECTION('center_axis',(-0.855183382508501,0.518325556268759,0.));
#29687=DIRECTION('ref_axis',(0.518325556268759,0.855183382508501,0.));
#29688=DIRECTION('center_axis',(1.,0.,0.));
#29689=DIRECTION('ref_axis',(0.,0.,-1.));
#29690=DIRECTION('',(-1.,0.,0.));
#29691=DIRECTION('center_axis',(-1.,0.,0.));
#29692=DIRECTION('ref_axis',(0.,0.,-1.));
#29693=DIRECTION('',(1.,0.,0.));
#29694=DIRECTION('center_axis',(1.,0.,0.));
#29695=DIRECTION('ref_axis',(0.,0.,-1.));
#29696=DIRECTION('center_axis',(-0.829037572548639,-0.55919290348024,0.));
#29697=DIRECTION('ref_axis',(-0.55919290348024,0.829037572548639,0.));
#29698=DIRECTION('',(1.,0.,0.));
#29699=DIRECTION('center_axis',(0.82903757255312,0.559192903473596,0.));
#29700=DIRECTION('ref_axis',(-0.559192903473596,0.82903757255312,0.));
#29701=DIRECTION('center_axis',(0.500000000011392,0.866025403777861,2.42431616218218E-14));
#29702=DIRECTION('ref_axis',(0.866025403777861,-0.500000000011392,1.34504687835035E-10));
#29703=DIRECTION('',(-1.,0.,0.));
#29704=DIRECTION('center_axis',(-0.500000000001136,-0.866025403783783,8.28529430747307E-15));
#29705=DIRECTION('ref_axis',(0.866025403783783,-0.500000000001136,-3.29777777975133E-11));
#29706=DIRECTION('center_axis',(0.500000000001135,-0.866025403783783,5.5235295383155E-15));
#29707=DIRECTION('ref_axis',(0.866025403783783,0.500000000001135,-1.55386342491463E-11));
#29708=DIRECTION('',(-1.,0.,0.));
#29709=DIRECTION('center_axis',(-0.50000000001139,0.866025403777863,4.84863232436438E-14));
#29710=DIRECTION('ref_axis',(0.866025403777863,0.50000000001139,-3.46934311402352E-10));
#29711=DIRECTION('center_axis',(1.,0.,0.));
#29712=DIRECTION('ref_axis',(0.,0.,-1.));
#29713=DIRECTION('center_axis',(-1.,0.,0.));
#29714=DIRECTION('ref_axis',(0.,0.,-1.));
#29715=DIRECTION('',(1.,0.,0.));
#29716=DIRECTION('center_axis',(-1.,0.,0.));
#29717=DIRECTION('ref_axis',(0.,0.,-1.));
#29718=DIRECTION('',(-1.,0.,0.));
#29719=DIRECTION('center_axis',(1.,0.,0.));
#29720=DIRECTION('ref_axis',(0.,0.,-1.));
#29721=DIRECTION('',(1.,0.,0.));
#29722=DIRECTION('center_axis',(1.,0.,0.));
#29723=DIRECTION('ref_axis',(0.,0.,-1.));
#29724=DIRECTION('',(1.,0.,0.));
#29725=DIRECTION('center_axis',(-1.,0.,0.));
#29726=DIRECTION('ref_axis',(0.,0.,1.));
#29727=DIRECTION('',(0.,0.,-1.));
#29728=DIRECTION('',(0.,0.,-1.));
#29729=DIRECTION('center_axis',(0.,1.,0.));
#29730=DIRECTION('ref_axis',(1.,0.,0.));
#29731=DIRECTION('',(0.,0.,-1.));
#29732=DIRECTION('center_axis',(0.,1.,0.));
#29733=DIRECTION('ref_axis',(1.,0.,0.));
#29734=DIRECTION('',(0.,0.,-1.));
#29735=DIRECTION('center_axis',(-1.,0.,0.));
#29736=DIRECTION('ref_axis',(0.,0.,1.));
#29737=DIRECTION('',(0.,0.,-1.));
#29738=DIRECTION('center_axis',(0.,-1.,0.));
#29739=DIRECTION('ref_axis',(0.,0.,-1.));
#29740=DIRECTION('',(0.,0.,-1.));
#29741=DIRECTION('center_axis',(1.,0.,0.));
#29742=DIRECTION('ref_axis',(0.,1.,0.));
#29743=DIRECTION('',(0.,0.,-1.));
#29744=DIRECTION('center_axis',(0.,1.,0.));
#29745=DIRECTION('ref_axis',(1.,0.,0.));
#29746=DIRECTION('',(0.,0.,-1.));
#29747=DIRECTION('center_axis',(1.,0.,0.));
#29748=DIRECTION('ref_axis',(0.,1.,0.));
#29749=DIRECTION('center_axis',(-0.855183382508501,0.518325556268759,0.));
#29750=DIRECTION('ref_axis',(0.,0.,1.));
#29751=DIRECTION('',(0.,0.,-1.));
#29752=DIRECTION('center_axis',(0.855183382508501,-0.518325556268759,0.));
#29753=DIRECTION('ref_axis',(0.518325556268759,0.855183382508501,0.));
#29754=DIRECTION('',(0.,0.,-1.));
#29755=DIRECTION('center_axis',(0.,1.,0.));
#29756=DIRECTION('ref_axis',(1.,0.,0.));
#29757=DIRECTION('',(0.,0.,-1.));
#29758=DIRECTION('',(1.,0.,0.));
#29759=DIRECTION('center_axis',(0.855183382509445,-0.518325556267202,0.));
#29760=DIRECTION('ref_axis',(0.,0.,-1.));
#29761=DIRECTION('',(0.,0.,-1.));
#29762=DIRECTION('center_axis',(0.855183382509445,-0.518325556267202,0.));
#29763=DIRECTION('ref_axis',(0.518325556267202,0.855183382509445,0.));
#29764=DIRECTION('center_axis',(0.,-1.,0.));
#29765=DIRECTION('ref_axis',(0.,0.,-1.));
#29766=DIRECTION('',(0.,0.,-1.));
#29767=DIRECTION('',(-1.,0.,0.));
#29768=DIRECTION('',(0.,0.,-1.));
#29769=DIRECTION('center_axis',(-0.829037572548639,-0.55919290348024,0.));
#29770=DIRECTION('ref_axis',(-0.55919290348024,0.829037572548639,0.));
#29771=DIRECTION('',(0.,0.,-1.));
#29772=DIRECTION('center_axis',(0.829037572548639,0.55919290348024,0.));
#29773=DIRECTION('ref_axis',(-0.55919290348024,0.829037572548639,0.));
#29774=DIRECTION('center_axis',(1.,0.,0.));
#29775=DIRECTION('ref_axis',(0.,1.,0.));
#29776=DIRECTION('',(0.,0.,-1.));
#29777=DIRECTION('center_axis',(-1.,0.,0.));
#29778=DIRECTION('ref_axis',(0.,0.,-1.));
#29779=DIRECTION('center_axis',(0.,-1.,0.));
#29780=DIRECTION('ref_axis',(0.,0.,-1.));
#29781=DIRECTION('',(0.,0.,-1.));
#29782=DIRECTION('',(-1.,0.,0.));
#29783=DIRECTION('center_axis',(-1.,0.,0.));
#29784=DIRECTION('ref_axis',(0.,0.,1.));
#29785=DIRECTION('',(0.,0.,-1.));
#29786=DIRECTION('center_axis',(1.,0.,0.));
#29787=DIRECTION('ref_axis',(0.,0.,-1.));
#29788=DIRECTION('center_axis',(0.,1.,0.));
#29789=DIRECTION('ref_axis',(1.,0.,0.));
#29790=DIRECTION('',(0.,0.,-1.));
#29791=DIRECTION('',(1.,0.,0.));
#29792=DIRECTION('center_axis',(1.,0.,0.));
#29793=DIRECTION('ref_axis',(0.,1.,0.));
#29794=DIRECTION('center_axis',(-1.,0.,0.));
#29795=DIRECTION('ref_axis',(0.,0.,-1.));
#29796=DIRECTION('center_axis',(0.82903757255312,0.559192903473596,0.));
#29797=DIRECTION('ref_axis',(0.,0.,-1.));
#29798=DIRECTION('center_axis',(-0.82903757255312,-0.559192903473596,0.));
#29799=DIRECTION('ref_axis',(-0.559192903473596,0.82903757255312,0.));
#29800=DIRECTION('center_axis',(1.,0.,0.));
#29801=DIRECTION('ref_axis',(0.,0.,-1.));
#29802=DIRECTION('center_axis',(1.,0.,0.));
#29803=DIRECTION('ref_axis',(0.,0.,-1.));
#29804=DIRECTION('center_axis',(-0.500000000001133,-0.866025403783785,1.87875446695563E-14));
#29805=DIRECTION('ref_axis',(0.866025403783785,-0.500000000001133,1.73760906682291E-11));
#29806=DIRECTION('',(-1.,0.,0.));
#29807=DIRECTION('center_axis',(0.500000000011412,0.86602540377785,2.35812383115421E-13));
#29808=DIRECTION('ref_axis',(0.86602540377785,-0.500000000011412,4.13106356090107E-10));
#29809=DIRECTION('center_axis',(-0.500000000011409,0.866025403777852,1.88649906492394E-13));
#29810=DIRECTION('ref_axis',(0.866025403777852,0.500000000011409,-1.71455444984074E-12));
#29811=DIRECTION('',(-1.,0.,0.));
#29812=DIRECTION('center_axis',(0.500000000001134,-0.866025403783784,2.6839349527939E-15));
#29813=DIRECTION('ref_axis',(0.866025403783784,0.500000000001134,2.2215382786634E-11));
#29814=DIRECTION('center_axis',(-0.500000000011394,-0.866025403777861,0.));
#29815=DIRECTION('ref_axis',(-0.866025403777861,0.500000000011394,0.));
#29816=DIRECTION('',(0.,0.,-1.));
#29817=DIRECTION('',(0.,0.,-1.));
#29818=DIRECTION('center_axis',(0.500000000011394,-0.866025403777861,0.));
#29819=DIRECTION('ref_axis',(0.,0.,-1.));
#29820=DIRECTION('',(0.,0.,-1.));
#29821=DIRECTION('center_axis',(0.,-1.,0.));
#29822=DIRECTION('ref_axis',(0.,0.,-1.));
#29823=DIRECTION('',(0.,0.,-1.));
#29824=DIRECTION('center_axis',(0.500000000001135,0.866025403783784,0.));
#29825=DIRECTION('ref_axis',(0.,0.,-1.));
#29826=DIRECTION('',(0.,0.,-1.));
#29827=DIRECTION('center_axis',(-0.500000000001135,0.866025403783784,0.));
#29828=DIRECTION('ref_axis',(0.,0.,1.));
#29829=DIRECTION('',(0.,0.,-1.));
#29830=DIRECTION('center_axis',(0.,-1.,0.));
#29831=DIRECTION('ref_axis',(0.,0.,-1.));
#29832=DIRECTION('center_axis',(0.,1.,0.));
#29833=DIRECTION('ref_axis',(1.,0.,0.));
#29834=DIRECTION('',(0.,0.,-1.));
#29835=DIRECTION('',(1.,0.,0.));
#29836=DIRECTION('',(0.,0.,-1.));
#29837=DIRECTION('center_axis',(0.500000000001135,-0.866025403783784,0.));
#29838=DIRECTION('ref_axis',(0.,0.,-1.));
#29839=DIRECTION('',(0.,0.,-1.));
#29840=DIRECTION('center_axis',(-0.500000000001134,0.866025403783784,1.34196747639693E-14));
#29841=DIRECTION('ref_axis',(0.866025403783784,0.500000000001134,-2.93336016297228E-11));
#29842=DIRECTION('center_axis',(-0.500000000001135,-0.866025403783784,0.));
#29843=DIRECTION('ref_axis',(-0.866025403783784,0.500000000001135,0.));
#29844=DIRECTION('',(0.,0.,-1.));
#29845=DIRECTION('center_axis',(0.500000000001132,0.866025403783785,2.41554145751436E-14));
#29846=DIRECTION('ref_axis',(0.866025403783785,-0.500000000001132,1.58006467766065E-11));
#29847=DIRECTION('center_axis',(0.,1.,0.));
#29848=DIRECTION('ref_axis',(1.,0.,0.));
#29849=DIRECTION('',(0.,0.,-1.));
#29850=DIRECTION('',(1.,0.,0.));
#29851=DIRECTION('center_axis',(-0.500000000011394,0.866025403777861,0.));
#29852=DIRECTION('ref_axis',(0.,0.,1.));
#29853=DIRECTION('center_axis',(0.500000000011412,-0.86602540377785,2.35812383115473E-13));
#29854=DIRECTION('ref_axis',(0.86602540377785,0.500000000011412,1.59264985720823E-10));
#29855=DIRECTION('',(0.,0.,-1.));
#29856=DIRECTION('center_axis',(0.500000000011394,0.866025403777861,0.));
#29857=DIRECTION('ref_axis',(0.,0.,-1.));
#29858=DIRECTION('center_axis',(-0.500000000011402,-0.866025403777856,1.17906191557739E-13));
#29859=DIRECTION('ref_axis',(0.866025403777856,-0.500000000011402,-2.60506588040655E-10));
#29860=DIRECTION('center_axis',(1.,0.,0.));
#29861=DIRECTION('ref_axis',(0.,0.,-1.));
#29862=DIRECTION('center_axis',(-0.946028810160758,0.324082536317247,0.));
#29863=DIRECTION('ref_axis',(0.,0.,1.));
#29864=DIRECTION('',(0.,0.,-1.));
#29865=DIRECTION('center_axis',(0.94602881016076,-0.324082536317242,-7.53842350672448E-14));
#29866=DIRECTION('ref_axis',(0.033646559749939,0.0982176184129628,-0.99459600263136));
#29867=DIRECTION('',(0.,0.,-1.));
#29868=DIRECTION('center_axis',(0.,1.,0.));
#29869=DIRECTION('ref_axis',(1.,0.,0.));
#29870=DIRECTION('',(0.,0.,-1.));
#29871=DIRECTION('',(1.,0.,0.));
#29872=DIRECTION('center_axis',(0.946028810171404,-0.324082536286173,0.));
#29873=DIRECTION('ref_axis',(0.,0.,-1.));
#29874=DIRECTION('',(0.,0.,-1.));
#29875=DIRECTION('center_axis',(-0.946028810149238,0.324082536350876,-7.54583899480575E-10));
#29876=DIRECTION('ref_axis',(0.00721450072149016,0.0210598351143057,-0.999752186456373));
#29877=DIRECTION('center_axis',(0.,0.,-1.));
#29878=DIRECTION('ref_axis',(0.587785252292473,0.809016994374947,0.));
#29879=DIRECTION('',(0.,0.,-1.));
#29880=DIRECTION('center_axis',(0.,-1.,0.));
#29881=DIRECTION('ref_axis',(0.,0.,-1.));
#29882=DIRECTION('',(0.,0.,-1.));
#29883=DIRECTION('',(-1.,0.,0.));
#29884=DIRECTION('center_axis',(-1.,0.,0.));
#29885=DIRECTION('ref_axis',(0.,0.,1.));
#29886=DIRECTION('',(0.,0.,-1.));
#29887=DIRECTION('center_axis',(-1.,0.,0.));
#29888=DIRECTION('ref_axis',(0.,0.,-1.));
#29889=DIRECTION('',(0.,0.,-1.));
#29890=DIRECTION('center_axis',(0.,-1.,0.));
#29891=DIRECTION('ref_axis',(0.,0.,-1.));
#29892=DIRECTION('',(0.,0.,-1.));
#29893=DIRECTION('',(1.,0.,0.));
#29894=DIRECTION('center_axis',(-1.,0.,0.));
#29895=DIRECTION('ref_axis',(0.,0.,1.));
#29896=DIRECTION('',(0.,0.,-1.));
#29897=DIRECTION('center_axis',(1.,0.,0.));
#29898=DIRECTION('ref_axis',(0.,0.,-1.));
#29899=DIRECTION('center_axis',(0.,1.,0.));
#29900=DIRECTION('ref_axis',(1.,0.,0.));
#29901=DIRECTION('',(0.,0.,-1.));
#29902=DIRECTION('',(1.,0.,0.));
#29903=DIRECTION('center_axis',(1.,0.,0.));
#29904=DIRECTION('ref_axis',(0.,1.,0.));
#29905=DIRECTION('',(0.,0.,-1.));
#29906=DIRECTION('center_axis',(-1.,0.,0.));
#29907=DIRECTION('ref_axis',(0.,0.,-1.));
#29908=DIRECTION('center_axis',(0.,1.,0.));
#29909=DIRECTION('ref_axis',(1.,0.,0.));
#29910=DIRECTION('',(1.,0.,0.));
#29911=DIRECTION('center_axis',(0.,0.,-1.));
#29912=DIRECTION('ref_axis',(0.,1.,0.));
#29913=DIRECTION('',(0.,0.,-1.));
#29914=DIRECTION('center_axis',(0.,1.,0.));
#29915=DIRECTION('ref_axis',(1.,0.,0.));
#29916=DIRECTION('',(-1.,0.,0.));
#29917=DIRECTION('center_axis',(1.,0.,0.));
#29918=DIRECTION('ref_axis',(0.,0.,-1.));
#29919=DIRECTION('axis',(0.,0.,1.));
#29920=DIRECTION('refdir',(1.,0.,0.));
#29921=DIRECTION('center_axis',(0.,0.,-1.));
#29922=DIRECTION('ref_axis',(0.,-1.,0.));
#29923=DIRECTION('center_axis',(0.,0.,-1.));
#29924=DIRECTION('ref_axis',(1.,0.,0.));
#29925=DIRECTION('',(0.866025403761798,0.500000000039214,0.));
#29926=DIRECTION('',(0.,1.,0.));
#29927=DIRECTION('',(-0.866025403761798,0.500000000039214,0.));
#29928=DIRECTION('',(-0.866025403761798,-0.500000000039214,0.));
#29929=DIRECTION('',(0.,-1.,0.));
#29930=DIRECTION('',(0.866025403761798,-0.500000000039214,0.));
#29931=DIRECTION('center_axis',(0.,0.,1.));
#29932=DIRECTION('ref_axis',(1.,0.,0.));
#29933=DIRECTION('center_axis',(0.,0.,1.));
#29934=DIRECTION('ref_axis',(1.,0.,0.));
#29935=DIRECTION('center_axis',(0.,0.,-1.));
#29936=DIRECTION('ref_axis',(1.,0.,0.));
#29937=DIRECTION('',(0.,0.,1.));
#29938=DIRECTION('center_axis',(0.,0.,1.));
#29939=DIRECTION('ref_axis',(1.,0.,0.));
#29940=DIRECTION('',(0.866025403761798,-0.500000000039214,0.));
#29941=DIRECTION('',(0.,-1.,0.));
#29942=DIRECTION('',(-0.866025403761798,-0.500000000039214,0.));
#29943=DIRECTION('',(-0.866025403761798,0.500000000039214,0.));
#29944=DIRECTION('',(0.,1.,0.));
#29945=DIRECTION('',(0.866025403761798,0.500000000039214,0.));
#29946=DIRECTION('center_axis',(-0.500000000039214,-0.866025403761798,0.));
#29947=DIRECTION('ref_axis',(-0.866025403761798,0.500000000039214,0.));
#29948=DIRECTION('',(0.,0.,-1.));
#29949=DIRECTION('',(0.,0.,-1.));
#29950=DIRECTION('center_axis',(-1.,0.,0.));
#29951=DIRECTION('ref_axis',(0.,0.,1.));
#29952=DIRECTION('',(0.,0.,-1.));
#29953=DIRECTION('center_axis',(-0.500000000039214,0.866025403761798,0.));
#29954=DIRECTION('ref_axis',(0.,0.,1.));
#29955=DIRECTION('',(0.,0.,-1.));
#29956=DIRECTION('center_axis',(0.500000000039214,0.866025403761798,0.));
#29957=DIRECTION('ref_axis',(0.,0.,-1.));
#29958=DIRECTION('',(0.,0.,-1.));
#29959=DIRECTION('center_axis',(1.,0.,0.));
#29960=DIRECTION('ref_axis',(0.,1.,0.));
#29961=DIRECTION('',(0.,0.,-1.));
#29962=DIRECTION('center_axis',(0.500000000039214,-0.866025403761798,0.));
#29963=DIRECTION('ref_axis',(0.,0.,-1.));
#29964=DIRECTION('axis',(0.,0.,1.));
#29965=DIRECTION('refdir',(1.,0.,0.));
#29966=DIRECTION('center_axis',(1.,0.,0.));
#29967=DIRECTION('ref_axis',(0.,1.,0.));
#29968=DIRECTION('center_axis',(-1.,0.,0.));
#29969=DIRECTION('ref_axis',(0.,-0.499999999993262,-0.866025403788329));
#29970=DIRECTION('center_axis',(-1.,0.,0.));
#29971=DIRECTION('ref_axis',(0.,0.,1.));
#29972=DIRECTION('center_axis',(-1.,0.,0.));
#29973=DIRECTION('ref_axis',(0.,1.,0.));
#29974=DIRECTION('center_axis',(-1.,0.,0.));
#29975=DIRECTION('ref_axis',(0.,0.,-1.));
#29976=DIRECTION('center_axis',(-1.,0.,0.));
#29977=DIRECTION('ref_axis',(0.,0.,1.));
#29978=DIRECTION('center_axis',(-1.,0.,0.));
#29979=DIRECTION('ref_axis',(0.,0.,1.));
#29980=DIRECTION('',(0.,0.,-1.));
#29981=DIRECTION('',(0.,1.,0.));
#29982=DIRECTION('',(0.,0.,1.));
#29983=DIRECTION('center_axis',(1.,0.,0.));
#29984=DIRECTION('ref_axis',(0.,0.,1.));
#29985=DIRECTION('center_axis',(1.,0.,0.));
#29986=DIRECTION('ref_axis',(0.,0.,1.));
#29987=DIRECTION('center_axis',(-1.,0.,0.));
#29988=DIRECTION('ref_axis',(0.,0.,1.));
#29989=DIRECTION('',(-0.707106781186548,-8.65956056235493E-17,0.707106781186547));
#29990=DIRECTION('center_axis',(-1.,0.,0.));
#29991=DIRECTION('ref_axis',(0.,0.,1.));
#29992=DIRECTION('',(-1.,0.,0.));
#29993=DIRECTION('',(1.,0.,0.));
#29994=DIRECTION('center_axis',(-1.,0.,0.));
#29995=DIRECTION('ref_axis',(0.,0.,1.));
#29996=DIRECTION('center_axis',(1.,0.,0.));
#29997=DIRECTION('ref_axis',(0.,1.,0.));
#29998=DIRECTION('center_axis',(-1.,0.,0.));
#29999=DIRECTION('ref_axis',(0.,1.,0.));
#30000=DIRECTION('center_axis',(-1.,0.,0.));
#30001=DIRECTION('ref_axis',(0.,0.,1.));
#30002=DIRECTION('center_axis',(-1.,0.,0.));
#30003=DIRECTION('ref_axis',(0.,-0.499999999993262,0.866025403788329));
#30004=DIRECTION('center_axis',(-1.,0.,0.));
#30005=DIRECTION('ref_axis',(0.,0.,-1.));
#30006=DIRECTION('center_axis',(1.,0.,0.));
#30007=DIRECTION('ref_axis',(0.,1.,0.));
#30008=DIRECTION('center_axis',(-1.,0.,0.));
#30009=DIRECTION('ref_axis',(0.,-0.499999999993262,-0.866025403788329));
#30010=DIRECTION('center_axis',(-1.,0.,0.));
#30011=DIRECTION('ref_axis',(0.,0.,-1.));
#30012=DIRECTION('center_axis',(-1.,0.,0.));
#30013=DIRECTION('ref_axis',(0.,-0.499999999993262,0.866025403788329));
#30014=DIRECTION('center_axis',(-1.,0.,0.));
#30015=DIRECTION('ref_axis',(0.,0.,1.));
#30016=DIRECTION('center_axis',(1.,0.,0.));
#30017=DIRECTION('ref_axis',(0.,-0.499999999993262,-0.866025403788329));
#30018=DIRECTION('center_axis',(-1.,0.,0.));
#30019=DIRECTION('ref_axis',(0.,-0.499999999993262,-0.866025403788329));
#30020=DIRECTION('',(-1.,0.,0.));
#30021=DIRECTION('',(1.,0.,0.));
#30022=DIRECTION('center_axis',(1.,0.,0.));
#30023=DIRECTION('ref_axis',(0.,1.22464679914735E-16,1.));
#30024=DIRECTION('',(-1.,0.,0.));
#30025=DIRECTION('center_axis',(-1.,0.,0.));
#30026=DIRECTION('ref_axis',(0.,0.,-1.));
#30027=DIRECTION('',(1.,0.,0.));
#30028=DIRECTION('center_axis',(1.,0.,0.));
#30029=DIRECTION('ref_axis',(0.,0.,-1.));
#30030=DIRECTION('',(-1.,0.,0.));
#30031=DIRECTION('center_axis',(-1.,0.,0.));
#30032=DIRECTION('ref_axis',(0.,0.,-1.));
#30033=DIRECTION('',(1.,0.,0.));
#30034=DIRECTION('center_axis',(1.,0.,0.));
#30035=DIRECTION('ref_axis',(0.,0.,-1.));
#30036=DIRECTION('',(-1.,0.,0.));
#30037=DIRECTION('center_axis',(-1.,0.,0.));
#30038=DIRECTION('ref_axis',(0.,0.,-1.));
#30039=DIRECTION('center_axis',(1.,0.,0.));
#30040=DIRECTION('ref_axis',(0.,0.17575598334211,-0.98443376329718));
#30041=DIRECTION('',(1.,0.,0.));
#30042=DIRECTION('center_axis',(-1.,0.,0.));
#30043=DIRECTION('ref_axis',(0.,-0.499999999993262,0.866025403788329));
#30044=DIRECTION('center_axis',(1.,0.,0.));
#30045=DIRECTION('ref_axis',(0.,-0.499999999993262,0.866025403788329));
#30046=DIRECTION('center_axis',(-1.,0.,0.));
#30047=DIRECTION('ref_axis',(0.,-0.499999999993262,0.866025403788329));
#30048=DIRECTION('',(-1.,0.,0.));
#30049=DIRECTION('center_axis',(-1.,0.,0.));
#30050=DIRECTION('ref_axis',(0.,0.,1.));
#30051=DIRECTION('center_axis',(-1.,0.,0.));
#30052=DIRECTION('ref_axis',(0.,0.,1.));
#30053=DIRECTION('center_axis',(-1.,0.,0.));
#30054=DIRECTION('ref_axis',(0.,1.,0.));
#30055=DIRECTION('center_axis',(-1.,0.,0.));
#30056=DIRECTION('ref_axis',(0.,0.,1.));
#30057=DIRECTION('center_axis',(-1.,0.,0.));
#30058=DIRECTION('ref_axis',(0.,0.,1.));
#30059=DIRECTION('center_axis',(-1.,0.,0.));
#30060=DIRECTION('ref_axis',(0.,1.,0.));
#30061=DIRECTION('center_axis',(-1.,0.,0.));
#30062=DIRECTION('ref_axis',(0.,0.,1.));
#30063=DIRECTION('center_axis',(-1.,0.,0.));
#30064=DIRECTION('ref_axis',(0.,-0.499999999993262,-0.866025403788329));
#30065=DIRECTION('',(0.,0.,1.));
#30066=DIRECTION('center_axis',(-1.,0.,0.));
#30067=DIRECTION('ref_axis',(0.,0.,1.));
#30068=DIRECTION('',(0.,0.,-1.));
#30069=DIRECTION('',(0.,-1.,0.));
#30070=DIRECTION('center_axis',(1.,0.,0.));
#30071=DIRECTION('ref_axis',(0.,-0.94042263903113,0.340007735202781));
#30072=DIRECTION('',(1.,0.,0.));
#30073=DIRECTION('center_axis',(1.,0.,0.));
#30074=DIRECTION('ref_axis',(0.,1.,0.));
#30075=DIRECTION('',(-1.,0.,0.));
#30076=DIRECTION('center_axis',(1.,0.,0.));
#30077=DIRECTION('ref_axis',(0.,0.764666655685446,0.644426028092314));
#30078=DIRECTION('',(1.,0.,0.));
#30079=DIRECTION('center_axis',(-1.,0.,0.));
#30080=DIRECTION('ref_axis',(0.,0.,1.));
#30081=DIRECTION('',(1.,0.,0.));
#30082=DIRECTION('',(1.,0.,0.));
#30083=DIRECTION('',(-1.,0.,0.));
#30084=DIRECTION('',(-1.,0.,0.));
#30085=DIRECTION('center_axis',(0.,-1.,0.));
#30086=DIRECTION('ref_axis',(0.,0.,-1.));
#30087=DIRECTION('',(0.,0.,1.));
#30088=DIRECTION('',(1.,0.,0.));
#30089=DIRECTION('center_axis',(0.,-1.,0.));
#30090=DIRECTION('ref_axis',(0.,0.,-1.));
#30091=DIRECTION('',(0.,0.,-1.));
#30092=DIRECTION('',(1.,0.,0.));
#30093=DIRECTION('center_axis',(0.,0.,-1.));
#30094=DIRECTION('ref_axis',(0.,-1.,0.));
#30095=DIRECTION('center_axis',(0.,0.,1.));
#30096=DIRECTION('ref_axis',(1.,0.,0.));
#30097=DIRECTION('',(-1.,0.,0.));
#30098=DIRECTION('center_axis',(0.,0.,-1.));
#30099=DIRECTION('ref_axis',(0.,-1.,0.));
#30100=DIRECTION('center_axis',(0.,0.,1.));
#30101=DIRECTION('ref_axis',(1.,0.,0.));
#30102=DIRECTION('',(-1.,0.,0.));
#30103=DIRECTION('center_axis',(0.,0.,1.));
#30104=DIRECTION('ref_axis',(1.,0.,0.));
#30105=DIRECTION('center_axis',(0.,1.,0.));
#30106=DIRECTION('ref_axis',(1.,0.,0.));
#30107=DIRECTION('',(0.,0.,-1.));
#30108=DIRECTION('center_axis',(0.,1.,0.));
#30109=DIRECTION('ref_axis',(1.,0.,0.));
#30110=DIRECTION('',(0.,0.,1.));
#30111=DIRECTION('center_axis',(0.,0.,-1.));
#30112=DIRECTION('ref_axis',(1.,0.,0.));
#30113=DIRECTION('',(0.,0.,-1.));
#30114=DIRECTION('center_axis',(-1.,0.,0.));
#30115=DIRECTION('ref_axis',(0.,0.,1.));
#30116=DIRECTION('',(1.,0.,0.));
#30117=DIRECTION('',(1.,0.,0.));
#30118=DIRECTION('center_axis',(-0.946028810149232,-0.324082536350894,-7.74377105026033E-10));
#30119=DIRECTION('ref_axis',(-0.0328036819517733,0.0957571728004204,0.994864052173802));
#30120=DIRECTION('',(1.,0.,0.));
#30121=DIRECTION('center_axis',(0.94602881016076,0.324082536317243,-7.10771293430115E-14));
#30122=DIRECTION('ref_axis',(-0.0103965438556825,0.03034853443635,0.999485306712121));
#30123=DIRECTION('',(1.,0.,0.));
#30124=DIRECTION('center_axis',(-1.,0.,0.));
#30125=DIRECTION('ref_axis',(0.,0.,1.));
#30126=DIRECTION('',(1.,0.,0.));
#30127=DIRECTION('center_axis',(1.,0.,0.));
#30128=DIRECTION('ref_axis',(0.,0.,1.));
#30129=DIRECTION('',(-1.,0.,0.));
#30130=DIRECTION('center_axis',(-1.,0.,0.));
#30131=DIRECTION('ref_axis',(0.,0.,1.));
#30132=DIRECTION('',(1.,0.,0.));
#30133=DIRECTION('center_axis',(1.,0.,0.));
#30134=DIRECTION('ref_axis',(0.,0.,1.));
#30135=DIRECTION('',(1.,0.,0.));
#30136=DIRECTION('center_axis',(1.,0.,0.));
#30137=DIRECTION('ref_axis',(0.,0.,1.));
#30138=DIRECTION('',(-1.,0.,0.));
#30139=DIRECTION('center_axis',(-1.,0.,0.));
#30140=DIRECTION('ref_axis',(0.,0.,1.));
#30141=DIRECTION('',(1.,0.,0.));
#30142=DIRECTION('',(-1.,0.,0.));
#30143=DIRECTION('center_axis',(-0.50000000001139,-0.866025403777863,-5.6567377117582E-14));
#30144=DIRECTION('ref_axis',(0.866025403777863,-0.50000000001139,-7.49337626227376E-11));
#30145=DIRECTION('center_axis',(0.500000000011408,-0.866025403777852,1.85864239100662E-13));
#30146=DIRECTION('ref_axis',(0.866025403777852,0.500000000011408,-4.16431008826601E-10));
#30147=DIRECTION('',(-1.,0.,0.));
#30148=DIRECTION('center_axis',(-0.500000000001134,0.866025403783784,5.52352953831563E-15));
#30149=DIRECTION('ref_axis',(0.866025403783784,0.500000000001134,-1.60186152837855E-11));
#30150=DIRECTION('center_axis',(0.500000000001135,0.866025403783783,-5.52352953831541E-15));
#30151=DIRECTION('ref_axis',(0.866025403783783,-0.500000000001135,-3.15235664736174E-11));
#30152=DIRECTION('center_axis',(0.855183382509445,0.518325556267202,0.));
#30153=DIRECTION('ref_axis',(-0.518325556267202,0.855183382509445,0.));
#30154=DIRECTION('',(1.,0.,0.));
#30155=DIRECTION('center_axis',(0.855183382508501,0.518325556268759,0.));
#30156=DIRECTION('ref_axis',(-0.518325556268759,0.855183382508501,0.));
#30157=DIRECTION('center_axis',(-1.,0.,0.));
#30158=DIRECTION('ref_axis',(0.,0.,1.));
#30159=DIRECTION('',(1.,0.,0.));
#30160=DIRECTION('center_axis',(1.,0.,0.));
#30161=DIRECTION('ref_axis',(0.,0.,1.));
#30162=DIRECTION('',(-1.,0.,0.));
#30163=DIRECTION('center_axis',(-1.,0.,0.));
#30164=DIRECTION('ref_axis',(0.,0.,1.));
#30165=DIRECTION('center_axis',(0.829037572548639,-0.55919290348024,0.));
#30166=DIRECTION('ref_axis',(0.55919290348024,0.829037572548639,0.));
#30167=DIRECTION('',(-1.,0.,0.));
#30168=DIRECTION('center_axis',(-0.82903757255312,0.559192903473596,0.));
#30169=DIRECTION('ref_axis',(0.559192903473596,0.82903757255312,0.));
#30170=DIRECTION('center_axis',(-0.500000000011392,0.866025403777861,-2.42431616218218E-14));
#30171=DIRECTION('ref_axis',(0.866025403777861,0.500000000011392,1.34504687835035E-10));
#30172=DIRECTION('',(1.,0.,0.));
#30173=DIRECTION('center_axis',(0.500000000001136,-0.866025403783783,-8.28529430747307E-15));
#30174=DIRECTION('ref_axis',(0.866025403783783,0.500000000001136,-3.29777777975133E-11));
#30175=DIRECTION('center_axis',(-0.500000000001135,-0.866025403783783,-5.5235295383155E-15));
#30176=DIRECTION('ref_axis',(0.866025403783783,-0.500000000001135,-1.55386342491463E-11));
#30177=DIRECTION('',(1.,0.,0.));
#30178=DIRECTION('center_axis',(0.50000000001139,0.866025403777863,-4.84863232436438E-14));
#30179=DIRECTION('ref_axis',(0.866025403777863,-0.50000000001139,-3.46934311402352E-10));
#30180=DIRECTION('center_axis',(-1.,0.,0.));
#30181=DIRECTION('ref_axis',(0.,0.,1.));
#30182=DIRECTION('center_axis',(1.,0.,0.));
#30183=DIRECTION('ref_axis',(0.,0.,1.));
#30184=DIRECTION('',(-1.,0.,0.));
#30185=DIRECTION('center_axis',(1.,0.,0.));
#30186=DIRECTION('ref_axis',(0.,0.,1.));
#30187=DIRECTION('',(1.,0.,0.));
#30188=DIRECTION('center_axis',(-1.,0.,0.));
#30189=DIRECTION('ref_axis',(0.,0.,1.));
#30190=DIRECTION('',(-1.,0.,0.));
#30191=DIRECTION('center_axis',(-1.,0.,0.));
#30192=DIRECTION('ref_axis',(0.,0.,1.));
#30193=DIRECTION('',(-1.,0.,0.));
#30194=DIRECTION('center_axis',(1.,0.,0.));
#30195=DIRECTION('ref_axis',(0.,1.,0.));
#30196=DIRECTION('',(0.,0.,1.));
#30197=DIRECTION('',(0.,0.,1.));
#30198=DIRECTION('center_axis',(0.,1.,0.));
#30199=DIRECTION('ref_axis',(1.,0.,0.));
#30200=DIRECTION('',(0.,0.,1.));
#30201=DIRECTION('center_axis',(0.,1.,0.));
#30202=DIRECTION('ref_axis',(1.,0.,0.));
#30203=DIRECTION('',(0.,0.,1.));
#30204=DIRECTION('center_axis',(1.,0.,0.));
#30205=DIRECTION('ref_axis',(0.,1.,0.));
#30206=DIRECTION('',(0.,0.,1.));
#30207=DIRECTION('center_axis',(0.,-1.,0.));
#30208=DIRECTION('ref_axis',(0.,0.,-1.));
#30209=DIRECTION('',(0.,0.,1.));
#30210=DIRECTION('center_axis',(-1.,0.,0.));
#30211=DIRECTION('ref_axis',(0.,0.,1.));
#30212=DIRECTION('',(0.,0.,1.));
#30213=DIRECTION('center_axis',(0.,1.,0.));
#30214=DIRECTION('ref_axis',(1.,0.,0.));
#30215=DIRECTION('',(0.,0.,1.));
#30216=DIRECTION('center_axis',(-1.,0.,0.));
#30217=DIRECTION('ref_axis',(0.,0.,1.));
#30218=DIRECTION('center_axis',(0.855183382508501,0.518325556268759,0.));
#30219=DIRECTION('ref_axis',(0.,0.,-1.));
#30220=DIRECTION('',(0.,0.,1.));
#30221=DIRECTION('center_axis',(-0.855183382508501,-0.518325556268759,0.));
#30222=DIRECTION('ref_axis',(-0.518325556268759,0.855183382508501,0.));
#30223=DIRECTION('',(0.,0.,1.));
#30224=DIRECTION('center_axis',(0.,1.,0.));
#30225=DIRECTION('ref_axis',(1.,0.,0.));
#30226=DIRECTION('',(0.,0.,1.));
#30227=DIRECTION('',(-1.,0.,0.));
#30228=DIRECTION('center_axis',(-0.855183382509445,-0.518325556267202,0.));
#30229=DIRECTION('ref_axis',(-0.518325556267202,0.855183382509445,0.));
#30230=DIRECTION('',(0.,0.,1.));
#30231=DIRECTION('center_axis',(-0.855183382509445,-0.518325556267202,0.));
#30232=DIRECTION('ref_axis',(-0.518325556267202,0.855183382509445,0.));
#30233=DIRECTION('center_axis',(0.,-1.,0.));
#30234=DIRECTION('ref_axis',(0.,0.,-1.));
#30235=DIRECTION('',(0.,0.,1.));
#30236=DIRECTION('',(1.,0.,0.));
#30237=DIRECTION('',(0.,0.,1.));
#30238=DIRECTION('center_axis',(0.829037572548639,-0.55919290348024,0.));
#30239=DIRECTION('ref_axis',(0.,0.,-1.));
#30240=DIRECTION('',(0.,0.,1.));
#30241=DIRECTION('center_axis',(-0.829037572548639,0.55919290348024,0.));
#30242=DIRECTION('ref_axis',(0.55919290348024,0.829037572548639,0.));
#30243=DIRECTION('center_axis',(-1.,0.,0.));
#30244=DIRECTION('ref_axis',(0.,0.,1.));
#30245=DIRECTION('',(0.,0.,1.));
#30246=DIRECTION('center_axis',(1.,0.,0.));
#30247=DIRECTION('ref_axis',(0.,0.,1.));
#30248=DIRECTION('center_axis',(0.,-1.,0.));
#30249=DIRECTION('ref_axis',(0.,0.,-1.));
#30250=DIRECTION('',(0.,0.,1.));
#30251=DIRECTION('',(1.,0.,0.));
#30252=DIRECTION('center_axis',(1.,0.,0.));
#30253=DIRECTION('ref_axis',(0.,1.,0.));
#30254=DIRECTION('',(0.,0.,1.));
#30255=DIRECTION('center_axis',(-1.,0.,0.));
#30256=DIRECTION('ref_axis',(0.,0.,1.));
#30257=DIRECTION('center_axis',(0.,1.,0.));
#30258=DIRECTION('ref_axis',(1.,0.,0.));
#30259=DIRECTION('',(0.,0.,1.));
#30260=DIRECTION('',(-1.,0.,0.));
#30261=DIRECTION('center_axis',(-1.,0.,0.));
#30262=DIRECTION('ref_axis',(0.,0.,1.));
#30263=DIRECTION('center_axis',(1.,0.,0.));
#30264=DIRECTION('ref_axis',(0.,0.,1.));
#30265=DIRECTION('center_axis',(-0.82903757255312,0.559192903473596,0.));
#30266=DIRECTION('ref_axis',(0.,0.,1.));
#30267=DIRECTION('center_axis',(0.82903757255312,-0.559192903473596,0.));
#30268=DIRECTION('ref_axis',(0.559192903473596,0.82903757255312,0.));
#30269=DIRECTION('center_axis',(-1.,0.,0.));
#30270=DIRECTION('ref_axis',(0.,0.,1.));
#30271=DIRECTION('center_axis',(-1.,0.,0.));
#30272=DIRECTION('ref_axis',(0.,0.,1.));
#30273=DIRECTION('center_axis',(0.500000000001133,-0.866025403783785,-1.87875446695563E-14));
#30274=DIRECTION('ref_axis',(0.866025403783785,0.500000000001133,1.73760906682291E-11));
#30275=DIRECTION('',(1.,0.,0.));
#30276=DIRECTION('center_axis',(-0.500000000011412,0.86602540377785,-2.35812383115421E-13));
#30277=DIRECTION('ref_axis',(0.86602540377785,0.500000000011412,4.13106356090107E-10));
#30278=DIRECTION('center_axis',(0.500000000011409,0.866025403777852,-1.88649906492394E-13));
#30279=DIRECTION('ref_axis',(0.866025403777852,-0.500000000011409,-1.71455444984074E-12));
#30280=DIRECTION('',(1.,0.,0.));
#30281=DIRECTION('center_axis',(-0.500000000001134,-0.866025403783784,-2.6839349527939E-15));
#30282=DIRECTION('ref_axis',(0.866025403783784,-0.500000000001134,2.2215382786634E-11));
#30283=DIRECTION('center_axis',(0.500000000011394,-0.866025403777861,0.));
#30284=DIRECTION('ref_axis',(0.,0.,-1.));
#30285=DIRECTION('',(0.,0.,1.));
#30286=DIRECTION('',(0.,0.,1.));
#30287=DIRECTION('center_axis',(-0.500000000011394,-0.866025403777861,0.));
#30288=DIRECTION('ref_axis',(-0.866025403777861,0.500000000011394,0.));
#30289=DIRECTION('',(0.,0.,1.));
#30290=DIRECTION('center_axis',(0.,-1.,0.));
#30291=DIRECTION('ref_axis',(0.,0.,-1.));
#30292=DIRECTION('',(0.,0.,1.));
#30293=DIRECTION('center_axis',(-0.500000000001135,0.866025403783784,0.));
#30294=DIRECTION('ref_axis',(0.,0.,1.));
#30295=DIRECTION('',(0.,0.,1.));
#30296=DIRECTION('center_axis',(0.500000000001135,0.866025403783784,0.));
#30297=DIRECTION('ref_axis',(0.,0.,-1.));
#30298=DIRECTION('',(0.,0.,1.));
#30299=DIRECTION('center_axis',(0.,-1.,0.));
#30300=DIRECTION('ref_axis',(0.,0.,-1.));
#30301=DIRECTION('center_axis',(0.,1.,0.));
#30302=DIRECTION('ref_axis',(1.,0.,0.));
#30303=DIRECTION('',(0.,0.,1.));
#30304=DIRECTION('',(-1.,0.,0.));
#30305=DIRECTION('',(0.,0.,1.));
#30306=DIRECTION('center_axis',(-0.500000000001135,-0.866025403783784,0.));
#30307=DIRECTION('ref_axis',(-0.866025403783784,0.500000000001135,0.));
#30308=DIRECTION('',(0.,0.,1.));
#30309=DIRECTION('center_axis',(0.500000000001134,0.866025403783784,-1.34196747639693E-14));
#30310=DIRECTION('ref_axis',(0.866025403783784,-0.500000000001134,-2.93336016297228E-11));
#30311=DIRECTION('center_axis',(0.500000000001135,-0.866025403783784,0.));
#30312=DIRECTION('ref_axis',(0.,0.,-1.));
#30313=DIRECTION('',(0.,0.,1.));
#30314=DIRECTION('center_axis',(-0.500000000001132,0.866025403783785,-2.41554145751436E-14));
#30315=DIRECTION('ref_axis',(0.866025403783785,0.500000000001132,1.58006467766065E-11));
#30316=DIRECTION('center_axis',(0.,1.,0.));
#30317=DIRECTION('ref_axis',(1.,0.,0.));
#30318=DIRECTION('',(0.,0.,1.));
#30319=DIRECTION('',(-1.,0.,0.));
#30320=DIRECTION('center_axis',(0.500000000011394,0.866025403777861,0.));
#30321=DIRECTION('ref_axis',(0.,0.,-1.));
#30322=DIRECTION('center_axis',(-0.500000000011412,-0.86602540377785,-2.35812383115473E-13));
#30323=DIRECTION('ref_axis',(0.86602540377785,-0.500000000011412,1.59264985720823E-10));
#30324=DIRECTION('',(0.,0.,1.));
#30325=DIRECTION('center_axis',(-0.500000000011394,0.866025403777861,0.));
#30326=DIRECTION('ref_axis',(0.,0.,1.));
#30327=DIRECTION('center_axis',(0.500000000011402,-0.866025403777856,-1.17906191557739E-13));
#30328=DIRECTION('ref_axis',(0.866025403777856,0.500000000011402,-2.60506588040655E-10));
#30329=DIRECTION('center_axis',(-1.,0.,0.));
#30330=DIRECTION('ref_axis',(0.,0.,1.));
#30331=DIRECTION('center_axis',(0.946028810160758,0.324082536317247,0.));
#30332=DIRECTION('ref_axis',(0.,0.,-1.));
#30333=DIRECTION('',(0.,0.,1.));
#30334=DIRECTION('center_axis',(-0.94602881016076,-0.324082536317242,7.53842350672448E-14));
#30335=DIRECTION('ref_axis',(-0.033646559749939,0.0982176184129628,0.99459600263136));
#30336=DIRECTION('',(0.,0.,1.));
#30337=DIRECTION('center_axis',(0.,1.,0.));
#30338=DIRECTION('ref_axis',(1.,0.,0.));
#30339=DIRECTION('',(0.,0.,1.));
#30340=DIRECTION('',(-1.,0.,0.));
#30341=DIRECTION('center_axis',(-0.946028810171404,-0.324082536286173,0.));
#30342=DIRECTION('ref_axis',(-0.324082536286173,0.946028810171404,0.));
#30343=DIRECTION('',(0.,0.,1.));
#30344=DIRECTION('center_axis',(0.946028810149238,0.324082536350876,7.54583899480575E-10));
#30345=DIRECTION('ref_axis',(-0.00721450072149016,0.0210598351143057,0.999752186456373));
#30346=DIRECTION('center_axis',(0.,0.,1.));
#30347=DIRECTION('ref_axis',(-0.587785252292473,0.809016994374947,0.));
#30348=DIRECTION('',(0.,0.,1.));
#30349=DIRECTION('center_axis',(0.,-1.,0.));
#30350=DIRECTION('ref_axis',(0.,0.,-1.));
#30351=DIRECTION('',(0.,0.,1.));
#30352=DIRECTION('',(1.,0.,0.));
#30353=DIRECTION('center_axis',(1.,0.,0.));
#30354=DIRECTION('ref_axis',(0.,1.,0.));
#30355=DIRECTION('',(0.,0.,1.));
#30356=DIRECTION('center_axis',(1.,0.,0.));
#30357=DIRECTION('ref_axis',(0.,0.,1.));
#30358=DIRECTION('',(0.,0.,1.));
#30359=DIRECTION('center_axis',(0.,-1.,0.));
#30360=DIRECTION('ref_axis',(0.,0.,-1.));
#30361=DIRECTION('',(0.,0.,1.));
#30362=DIRECTION('',(-1.,0.,0.));
#30363=DIRECTION('center_axis',(1.,0.,0.));
#30364=DIRECTION('ref_axis',(0.,1.,0.));
#30365=DIRECTION('',(0.,0.,1.));
#30366=DIRECTION('center_axis',(-1.,0.,0.));
#30367=DIRECTION('ref_axis',(0.,0.,1.));
#30368=DIRECTION('center_axis',(0.,1.,0.));
#30369=DIRECTION('ref_axis',(1.,0.,0.));
#30370=DIRECTION('',(0.,0.,1.));
#30371=DIRECTION('',(-1.,0.,0.));
#30372=DIRECTION('center_axis',(-1.,0.,0.));
#30373=DIRECTION('ref_axis',(0.,0.,1.));
#30374=DIRECTION('',(0.,0.,1.));
#30375=DIRECTION('center_axis',(1.,0.,0.));
#30376=DIRECTION('ref_axis',(0.,0.,1.));
#30377=DIRECTION('center_axis',(0.,1.,0.));
#30378=DIRECTION('ref_axis',(1.,0.,0.));
#30379=DIRECTION('',(-1.,0.,0.));
#30380=DIRECTION('center_axis',(0.,0.,1.));
#30381=DIRECTION('ref_axis',(0.,1.,0.));
#30382=DIRECTION('',(0.,0.,1.));
#30383=DIRECTION('center_axis',(0.,1.,0.));
#30384=DIRECTION('ref_axis',(1.,0.,0.));
#30385=DIRECTION('',(1.,0.,0.));
#30386=DIRECTION('center_axis',(-1.,0.,0.));
#30387=DIRECTION('ref_axis',(0.,0.,1.));
#30388=DIRECTION('',(-1.54074395550979E-33,-2.06796457519173E-35,1.));
#30389=DIRECTION('',(1.,1.54074395550979E-33,1.54074395550979E-33));
#30390=DIRECTION('',(-1.54074395550979E-33,-2.06796457519173E-35,1.));
#30391=DIRECTION('',(1.,1.54074395550979E-33,1.54074395550979E-33));
#30392=DIRECTION('',(-1.54074395550979E-33,-2.06796457519173E-35,1.));
#30393=DIRECTION('',(1.,1.54074395550979E-33,1.54074395550979E-33));
#30394=DIRECTION('',(-1.54074395550979E-33,-2.06796457519173E-35,1.));
#30395=DIRECTION('',(1.,1.54074395550979E-33,1.54074395550979E-33));
#30396=DIRECTION('',(-1.54074395550979E-33,-2.06796457519173E-35,1.));
#30397=DIRECTION('',(1.,1.54074395550979E-33,1.54074395550979E-33));
#30398=DIRECTION('',(-7.70371977754895E-34,-2.06796457519173E-35,1.));
#30399=DIRECTION('',(1.,7.70371977754894E-34,7.70371977754895E-34));
#30400=DIRECTION('axis',(0.,0.,1.));
#30401=DIRECTION('refdir',(1.,0.,0.));
#30402=DIRECTION('axis',(0.,0.,1.));
#30403=DIRECTION('refdir',(1.,0.,0.));
#30404=DIRECTION('center_axis',(0.,-1.,0.));
#30405=DIRECTION('ref_axis',(0.,0.,-1.));
#30406=DIRECTION('center_axis',(0.,-1.,0.));
#30407=DIRECTION('ref_axis',(0.,0.,-1.));
#30408=DIRECTION('',(0.,-1.,0.));
#30409=DIRECTION('center_axis',(0.,-1.,0.));
#30410=DIRECTION('ref_axis',(0.,0.,-1.));
#30411=DIRECTION('center_axis',(0.,-1.,0.));
#30412=DIRECTION('ref_axis',(0.,0.,-1.));
#30413=DIRECTION('center_axis',(0.,-1.,0.));
#30414=DIRECTION('ref_axis',(0.,0.,-1.));
#30415=DIRECTION('',(0.,-1.,0.));
#30416=DIRECTION('center_axis',(0.,-1.,0.));
#30417=DIRECTION('ref_axis',(0.,0.,-1.));
#30418=DIRECTION('center_axis',(0.,-1.,0.));
#30419=DIRECTION('ref_axis',(0.,0.,-1.));
#30420=DIRECTION('center_axis',(0.,-1.,0.));
#30421=DIRECTION('ref_axis',(0.,0.,-1.));
#30422=DIRECTION('',(0.,-1.,0.));
#30423=DIRECTION('center_axis',(0.,-1.,0.));
#30424=DIRECTION('ref_axis',(0.,0.,-1.));
#30425=DIRECTION('center_axis',(0.,-1.,0.));
#30426=DIRECTION('ref_axis',(0.,0.,-1.));
#30427=DIRECTION('center_axis',(0.,-1.,0.));
#30428=DIRECTION('ref_axis',(0.,0.,-1.));
#30429=DIRECTION('',(0.,-1.,0.));
#30430=DIRECTION('center_axis',(0.,-1.,0.));
#30431=DIRECTION('ref_axis',(0.,0.,-1.));
#30432=DIRECTION('center_axis',(0.,-1.,0.));
#30433=DIRECTION('ref_axis',(0.,0.,-1.));
#30434=DIRECTION('center_axis',(0.,-1.,0.));
#30435=DIRECTION('ref_axis',(0.,0.,-1.));
#30436=DIRECTION('',(0.,-1.,0.));
#30437=DIRECTION('center_axis',(0.,-1.,0.));
#30438=DIRECTION('ref_axis',(0.,0.,-1.));
#30439=DIRECTION('center_axis',(0.,-1.,0.));
#30440=DIRECTION('ref_axis',(0.,0.,-1.));
#30441=DIRECTION('center_axis',(0.,-1.,0.));
#30442=DIRECTION('ref_axis',(0.,0.,-1.));
#30443=DIRECTION('',(0.,-1.,0.));
#30444=DIRECTION('center_axis',(0.,-1.,0.));
#30445=DIRECTION('ref_axis',(0.,0.,-1.));
#30446=DIRECTION('center_axis',(0.,-1.,0.));
#30447=DIRECTION('ref_axis',(0.,0.,-1.));
#30448=DIRECTION('center_axis',(0.,-1.,0.));
#30449=DIRECTION('ref_axis',(0.,0.,-1.));
#30450=DIRECTION('',(0.,-1.,0.));
#30451=DIRECTION('center_axis',(0.,-1.,0.));
#30452=DIRECTION('ref_axis',(0.,0.,-1.));
#30453=DIRECTION('center_axis',(0.,1.,0.));
#30454=DIRECTION('ref_axis',(0.,0.,1.));
#30455=DIRECTION('',(0.,0.,-1.));
#30456=DIRECTION('center_axis',(0.,-1.,0.));
#30457=DIRECTION('ref_axis',(0.,0.,1.));
#30458=DIRECTION('',(1.,0.,0.));
#30459=DIRECTION('',(0.,0.,-1.));
#30460=DIRECTION('',(1.,0.,0.));
#30461=DIRECTION('center_axis',(0.,-1.,0.));
#30462=DIRECTION('ref_axis',(0.,0.,1.));
#30463=DIRECTION('center_axis',(-1.,0.,0.));
#30464=DIRECTION('ref_axis',(0.,0.,1.));
#30465=DIRECTION('',(0.,0.,-1.));
#30466=DIRECTION('',(0.,-1.,0.));
#30467=DIRECTION('',(0.,1.,0.));
#30468=DIRECTION('center_axis',(0.,-1.,0.));
#30469=DIRECTION('ref_axis',(0.,0.,-1.));
#30470=DIRECTION('',(-1.,0.,0.));
#30471=DIRECTION('center_axis',(0.,1.,0.));
#30472=DIRECTION('ref_axis',(0.,0.,-1.));
#30473=DIRECTION('center_axis',(0.,1.,0.));
#30474=DIRECTION('ref_axis',(0.,0.,-1.));
#30475=DIRECTION('',(-1.,0.,0.));
#30476=DIRECTION('',(0.,0.,-1.));
#30477=DIRECTION('center_axis',(1.,0.,0.));
#30478=DIRECTION('ref_axis',(0.,0.,-1.));
#30479=DIRECTION('',(0.,-1.,0.));
#30480=DIRECTION('',(0.,-1.,0.));
#30481=DIRECTION('center_axis',(0.,0.,-1.));
#30482=DIRECTION('ref_axis',(-1.,0.,0.));
#30483=DIRECTION('',(0.,1.,0.));
#30484=DIRECTION('center_axis',(0.,0.,-1.));
#30485=DIRECTION('ref_axis',(-1.,0.,0.));
#30486=DIRECTION('',(0.,-1.,0.));
#30487=DIRECTION('center_axis',(0.,1.,0.));
#30488=DIRECTION('ref_axis',(0.,0.,1.));
#30489=DIRECTION('center_axis',(0.,-1.,0.));
#30490=DIRECTION('ref_axis',(0.,0.,-1.));
#30491=DIRECTION('axis',(0.,0.,1.));
#30492=DIRECTION('refdir',(1.,0.,0.));
#30493=DIRECTION('center_axis',(0.,0.,1.));
#30494=DIRECTION('ref_axis',(1.,0.,0.));
#30495=DIRECTION('center_axis',(0.,0.,1.));
#30496=DIRECTION('ref_axis',(1.,0.,0.));
#30497=DIRECTION('',(0.,0.,1.));
#30498=DIRECTION('center_axis',(0.,0.,1.));
#30499=DIRECTION('ref_axis',(1.,0.,0.));
#30500=DIRECTION('center_axis',(0.,0.,1.));
#30501=DIRECTION('ref_axis',(1.,0.,0.));
#30502=DIRECTION('center_axis',(0.,0.,1.));
#30503=DIRECTION('ref_axis',(1.,0.,0.));
#30504=DIRECTION('',(0.,0.,1.));
#30505=DIRECTION('center_axis',(0.,0.,1.));
#30506=DIRECTION('ref_axis',(1.,0.,0.));
#30507=DIRECTION('center_axis',(0.,0.,1.));
#30508=DIRECTION('ref_axis',(1.,0.,0.));
#30509=DIRECTION('center_axis',(0.,0.,1.));
#30510=DIRECTION('ref_axis',(1.,0.,0.));
#30511=DIRECTION('',(0.,0.,1.));
#30512=DIRECTION('center_axis',(0.,0.,1.));
#30513=DIRECTION('ref_axis',(1.,0.,0.));
#30514=DIRECTION('center_axis',(0.,0.,1.));
#30515=DIRECTION('ref_axis',(1.,0.,0.));
#30516=DIRECTION('center_axis',(0.,0.,1.));
#30517=DIRECTION('ref_axis',(1.,0.,0.));
#30518=DIRECTION('',(0.,0.,1.));
#30519=DIRECTION('center_axis',(0.,0.,1.));
#30520=DIRECTION('ref_axis',(1.,0.,0.));
#30521=DIRECTION('center_axis',(0.,0.,1.));
#30522=DIRECTION('ref_axis',(1.,0.,0.));
#30523=DIRECTION('center_axis',(0.,0.,1.));
#30524=DIRECTION('ref_axis',(1.,0.,0.));
#30525=DIRECTION('',(0.,0.,1.));
#30526=DIRECTION('center_axis',(0.,0.,1.));
#30527=DIRECTION('ref_axis',(1.,0.,0.));
#30528=DIRECTION('center_axis',(0.,0.,1.));
#30529=DIRECTION('ref_axis',(1.,0.,0.));
#30530=DIRECTION('center_axis',(0.,0.,1.));
#30531=DIRECTION('ref_axis',(1.,0.,0.));
#30532=DIRECTION('',(0.,0.,1.));
#30533=DIRECTION('center_axis',(0.,0.,1.));
#30534=DIRECTION('ref_axis',(1.,0.,0.));
#30535=DIRECTION('center_axis',(-1.,-9.25185853854297E-17,0.));
#30536=DIRECTION('ref_axis',(9.25185853854297E-17,-1.,0.));
#30537=DIRECTION('',(-9.25185853854297E-17,1.,0.));
#30538=DIRECTION('',(0.,0.,-1.));
#30539=DIRECTION('',(-9.25185853854297E-17,1.,0.));
#30540=DIRECTION('',(0.,0.,-1.));
#30541=DIRECTION('center_axis',(0.,-1.,0.));
#30542=DIRECTION('ref_axis',(0.,0.,-1.));
#30543=DIRECTION('',(-1.,0.,0.));
#30544=DIRECTION('',(0.,0.,-1.));
#30545=DIRECTION('',(-1.,0.,0.));
#30546=DIRECTION('center_axis',(1.,1.85037170770859E-16,0.));
#30547=DIRECTION('ref_axis',(-1.85037170770859E-16,1.,0.));
#30548=DIRECTION('',(1.85037170770859E-16,-1.,0.));
#30549=DIRECTION('',(0.,0.,-1.));
#30550=DIRECTION('',(1.85037170770859E-16,-1.,0.));
#30551=DIRECTION('center_axis',(0.,1.,0.));
#30552=DIRECTION('ref_axis',(0.,0.,1.));
#30553=DIRECTION('',(1.,0.,0.));
#30554=DIRECTION('',(1.,0.,0.));
#30555=DIRECTION('center_axis',(0.,0.,1.));
#30556=DIRECTION('ref_axis',(1.,0.,0.));
#30557=DIRECTION('center_axis',(0.,0.,1.));
#30558=DIRECTION('ref_axis',(1.,0.,0.));
#30559=DIRECTION('',(-6.16297582203385E-33,4.59047288926841E-32,1.));
#30560=DIRECTION('',(1.,-4.93038065763132E-32,6.16297582203385E-33));
#30561=DIRECTION('',(-1.,1.22464679914694E-16,9.47091042991064E-17));
#30562=DIRECTION('',(9.47091042991064E-17,-1.22464679914778E-16,1.));
#30563=DIRECTION('axis',(0.,0.,1.));
#30564=DIRECTION('refdir',(1.,0.,0.));
#30565=DIRECTION('center_axis',(0.,0.,1.));
#30566=DIRECTION('ref_axis',(1.,0.,0.));
#30567=DIRECTION('center_axis',(0.,0.,1.));
#30568=DIRECTION('ref_axis',(1.,0.,0.));
#30569=DIRECTION('',(0.,0.,1.));
#30570=DIRECTION('center_axis',(0.,0.,1.));
#30571=DIRECTION('ref_axis',(1.,0.,0.));
#30572=DIRECTION('center_axis',(0.,0.,1.));
#30573=DIRECTION('ref_axis',(1.,0.,0.));
#30574=DIRECTION('center_axis',(0.,0.,1.));
#30575=DIRECTION('ref_axis',(1.,0.,0.));
#30576=DIRECTION('',(0.,0.,1.));
#30577=DIRECTION('center_axis',(0.,0.,1.));
#30578=DIRECTION('ref_axis',(1.,0.,0.));
#30579=DIRECTION('center_axis',(0.,0.,1.));
#30580=DIRECTION('ref_axis',(1.,0.,0.));
#30581=DIRECTION('center_axis',(0.,0.,1.));
#30582=DIRECTION('ref_axis',(1.,0.,0.));
#30583=DIRECTION('',(0.,0.,1.));
#30584=DIRECTION('center_axis',(0.,0.,1.));
#30585=DIRECTION('ref_axis',(1.,0.,0.));
#30586=DIRECTION('center_axis',(0.,0.,1.));
#30587=DIRECTION('ref_axis',(1.,0.,0.));
#30588=DIRECTION('center_axis',(0.,0.,1.));
#30589=DIRECTION('ref_axis',(1.,0.,0.));
#30590=DIRECTION('',(0.,0.,1.));
#30591=DIRECTION('center_axis',(0.,0.,1.));
#30592=DIRECTION('ref_axis',(1.,0.,0.));
#30593=DIRECTION('center_axis',(0.,0.,1.));
#30594=DIRECTION('ref_axis',(1.,0.,0.));
#30595=DIRECTION('center_axis',(0.,0.,1.));
#30596=DIRECTION('ref_axis',(1.,0.,0.));
#30597=DIRECTION('',(0.,0.,1.));
#30598=DIRECTION('center_axis',(0.,0.,1.));
#30599=DIRECTION('ref_axis',(1.,0.,0.));
#30600=DIRECTION('center_axis',(0.,0.,1.));
#30601=DIRECTION('ref_axis',(1.,0.,0.));
#30602=DIRECTION('center_axis',(0.,0.,1.));
#30603=DIRECTION('ref_axis',(1.,0.,0.));
#30604=DIRECTION('',(0.,0.,1.));
#30605=DIRECTION('center_axis',(0.,0.,1.));
#30606=DIRECTION('ref_axis',(1.,0.,0.));
#30607=DIRECTION('center_axis',(-1.,-2.77555756156289E-16,0.));
#30608=DIRECTION('ref_axis',(2.77555756156289E-16,-1.,0.));
#30609=DIRECTION('',(-2.77555756156289E-16,1.,0.));
#30610=DIRECTION('',(0.,0.,-1.));
#30611=DIRECTION('',(-2.77555756156289E-16,1.,0.));
#30612=DIRECTION('',(0.,0.,-1.));
#30613=DIRECTION('center_axis',(0.,-1.,0.));
#30614=DIRECTION('ref_axis',(0.,0.,-1.));
#30615=DIRECTION('',(-1.,0.,0.));
#30616=DIRECTION('',(0.,0.,-1.));
#30617=DIRECTION('',(-1.,0.,0.));
#30618=DIRECTION('center_axis',(1.,1.85037170770859E-16,0.));
#30619=DIRECTION('ref_axis',(-1.85037170770859E-16,1.,0.));
#30620=DIRECTION('',(1.85037170770859E-16,-1.,0.));
#30621=DIRECTION('',(0.,0.,-1.));
#30622=DIRECTION('',(1.85037170770859E-16,-1.,0.));
#30623=DIRECTION('center_axis',(0.,1.,0.));
#30624=DIRECTION('ref_axis',(0.,0.,1.));
#30625=DIRECTION('',(1.,0.,0.));
#30626=DIRECTION('',(1.,0.,0.));
#30627=DIRECTION('center_axis',(0.,0.,1.));
#30628=DIRECTION('ref_axis',(1.,0.,0.));
#30629=DIRECTION('center_axis',(0.,0.,1.));
#30630=DIRECTION('ref_axis',(1.,0.,0.));
#30631=DIRECTION('axis',(0.,0.,1.));
#30632=DIRECTION('refdir',(1.,0.,0.));
#30633=DIRECTION('center_axis',(1.,0.,-3.96508223080413E-16));
#30634=DIRECTION('ref_axis',(-3.96508223080413E-16,0.,-1.));
#30635=DIRECTION('',(3.96508223080413E-16,0.,1.));
#30636=DIRECTION('',(0.,-1.,0.));
#30637=DIRECTION('',(3.96508223080413E-16,0.,1.));
#30638=DIRECTION('',(0.,-1.,0.));
#30639=DIRECTION('center_axis',(0.270745576918284,0.,-0.962650940153899));
#30640=DIRECTION('ref_axis',(-0.962650940153899,0.,-0.270745576918284));
#30641=DIRECTION('',(0.962650940153899,0.,0.270745576918284));
#30642=DIRECTION('',(0.,-1.,0.));
#30643=DIRECTION('',(0.962650940153899,0.,0.270745576918284));
#30644=DIRECTION('center_axis',(0.,0.,-1.));
#30645=DIRECTION('ref_axis',(-1.,0.,0.));
#30646=DIRECTION('',(1.,0.,0.));
#30647=DIRECTION('',(0.,-1.,0.));
#30648=DIRECTION('',(1.,0.,0.));
#30649=DIRECTION('center_axis',(1.,0.,0.));
#30650=DIRECTION('ref_axis',(0.,0.,-1.));
#30651=DIRECTION('',(0.,0.,1.));
#30652=DIRECTION('',(0.,-1.,0.));
#30653=DIRECTION('',(0.,0.,1.));
#30654=DIRECTION('center_axis',(0.,0.,-1.));
#30655=DIRECTION('ref_axis',(-1.,0.,0.));
#30656=DIRECTION('',(1.,0.,0.));
#30657=DIRECTION('',(1.,0.,0.));
#30658=DIRECTION('center_axis',(0.,1.,0.));
#30659=DIRECTION('ref_axis',(0.,0.,1.));
#30660=DIRECTION('center_axis',(0.,1.,0.));
#30661=DIRECTION('ref_axis',(0.,0.,1.));
#30662=DIRECTION('center_axis',(1.,0.,-3.96508223080413E-16));
#30663=DIRECTION('ref_axis',(-3.96508223080413E-16,0.,-1.));
#30664=DIRECTION('',(3.96508223080413E-16,0.,1.));
#30665=DIRECTION('',(0.,1.,0.));
#30666=DIRECTION('',(3.96508223080413E-16,0.,1.));
#30667=DIRECTION('',(0.,1.,0.));
#30668=DIRECTION('center_axis',(0.270745576918284,0.,-0.962650940153899));
#30669=DIRECTION('ref_axis',(-0.962650940153899,0.,-0.270745576918284));
#30670=DIRECTION('',(0.962650940153899,0.,0.270745576918284));
#30671=DIRECTION('',(0.962650940153899,0.,0.270745576918284));
#30672=DIRECTION('',(0.,1.,0.));
#30673=DIRECTION('center_axis',(0.,0.,-1.));
#30674=DIRECTION('ref_axis',(-1.,0.,0.));
#30675=DIRECTION('',(1.,0.,0.));
#30676=DIRECTION('',(1.,0.,0.));
#30677=DIRECTION('',(0.,1.,0.));
#30678=DIRECTION('center_axis',(1.,0.,0.));
#30679=DIRECTION('ref_axis',(0.,0.,-1.));
#30680=DIRECTION('',(0.,0.,1.));
#30681=DIRECTION('',(0.,0.,1.));
#30682=DIRECTION('',(0.,1.,0.));
#30683=DIRECTION('center_axis',(0.,0.,-1.));
#30684=DIRECTION('ref_axis',(-1.,0.,0.));
#30685=DIRECTION('',(1.,0.,0.));
#30686=DIRECTION('',(1.,0.,0.));
#30687=DIRECTION('center_axis',(0.,-1.,0.));
#30688=DIRECTION('ref_axis',(0.,0.,1.));
#30689=DIRECTION('center_axis',(0.,-1.,0.));
#30690=DIRECTION('ref_axis',(0.,0.,1.));
#30691=DIRECTION('center_axis',(0.,0.,-1.));
#30692=DIRECTION('ref_axis',(-1.,0.,0.));
#30693=DIRECTION('center_axis',(0.,0.,1.));
#30694=DIRECTION('ref_axis',(-1.,1.77635683940025E-15,0.));
#30695=DIRECTION('',(0.,0.,-1.));
#30696=DIRECTION('center_axis',(0.,0.,-1.));
#30697=DIRECTION('ref_axis',(-1.,0.,0.));
#30698=DIRECTION('',(0.,0.,-1.));
#30699=DIRECTION('center_axis',(0.,0.,1.));
#30700=DIRECTION('ref_axis',(1.,0.,0.));
#30701=DIRECTION('center_axis',(0.,0.,-1.));
#30702=DIRECTION('ref_axis',(-1.,0.,0.));
#30703=DIRECTION('',(0.,0.,1.));
#30704=DIRECTION('center_axis',(0.,0.,1.));
#30705=DIRECTION('ref_axis',(1.,0.,0.));
#30706=DIRECTION('center_axis',(0.,0.,1.));
#30707=DIRECTION('ref_axis',(1.,0.,0.));
#30708=DIRECTION('center_axis',(0.,0.,-1.));
#30709=DIRECTION('ref_axis',(-1.,0.,0.));
#30710=DIRECTION('',(0.,0.,1.));
#30711=DIRECTION('center_axis',(0.,0.,1.));
#30712=DIRECTION('ref_axis',(1.,0.,0.));
#30713=DIRECTION('center_axis',(0.,0.,1.));
#30714=DIRECTION('ref_axis',(1.,0.,0.));
#30715=DIRECTION('center_axis',(0.,0.,-1.));
#30716=DIRECTION('ref_axis',(-1.,0.,0.));
#30717=DIRECTION('',(0.,0.,1.));
#30718=DIRECTION('center_axis',(0.,0.,1.));
#30719=DIRECTION('ref_axis',(1.,0.,0.));
#30720=DIRECTION('center_axis',(0.,0.,1.));
#30721=DIRECTION('ref_axis',(1.,0.,0.));
#30722=DIRECTION('center_axis',(0.,0.,-1.));
#30723=DIRECTION('ref_axis',(-1.,0.,0.));
#30724=DIRECTION('',(0.,0.,1.));
#30725=DIRECTION('center_axis',(0.,0.,1.));
#30726=DIRECTION('ref_axis',(1.,0.,0.));
#30727=DIRECTION('center_axis',(0.,0.,1.));
#30728=DIRECTION('ref_axis',(1.,0.,0.));
#30729=DIRECTION('center_axis',(0.,0.,-1.));
#30730=DIRECTION('ref_axis',(-1.,0.,0.));
#30731=DIRECTION('',(0.,0.,1.));
#30732=DIRECTION('center_axis',(0.,0.,1.));
#30733=DIRECTION('ref_axis',(1.,0.,0.));
#30734=DIRECTION('center_axis',(0.,0.,1.));
#30735=DIRECTION('ref_axis',(1.,0.,0.));
#30736=DIRECTION('center_axis',(0.,0.,-1.));
#30737=DIRECTION('ref_axis',(-1.,0.,0.));
#30738=DIRECTION('',(0.,0.,1.));
#30739=DIRECTION('center_axis',(0.,0.,1.));
#30740=DIRECTION('ref_axis',(1.,0.,0.));
#30741=DIRECTION('center_axis',(0.,0.,1.));
#30742=DIRECTION('ref_axis',(1.,0.,0.));
#30743=DIRECTION('center_axis',(0.,0.,-1.));
#30744=DIRECTION('ref_axis',(-1.,0.,0.));
#30745=DIRECTION('',(0.,0.,1.));
#30746=DIRECTION('center_axis',(0.,0.,1.));
#30747=DIRECTION('ref_axis',(1.,0.,0.));
#30748=DIRECTION('center_axis',(0.,0.,1.));
#30749=DIRECTION('ref_axis',(1.,0.,0.));
#30750=DIRECTION('center_axis',(0.,0.,-1.));
#30751=DIRECTION('ref_axis',(-1.,0.,0.));
#30752=DIRECTION('',(0.,0.,1.));
#30753=DIRECTION('center_axis',(0.,0.,1.));
#30754=DIRECTION('ref_axis',(1.,0.,0.));
#30755=DIRECTION('center_axis',(0.,0.,1.));
#30756=DIRECTION('ref_axis',(1.,0.,0.));
#30757=DIRECTION('center_axis',(0.,0.,-1.));
#30758=DIRECTION('ref_axis',(-1.,0.,0.));
#30759=DIRECTION('',(0.,0.,1.));
#30760=DIRECTION('center_axis',(0.,0.,1.));
#30761=DIRECTION('ref_axis',(1.,0.,0.));
#30762=DIRECTION('center_axis',(0.,0.,1.));
#30763=DIRECTION('ref_axis',(1.,0.,0.));
#30764=DIRECTION('center_axis',(0.,0.,1.));
#30765=DIRECTION('ref_axis',(1.,0.,0.));
#30766=DIRECTION('',(0.,0.,1.));
#30767=DIRECTION('center_axis',(0.,0.,1.));
#30768=DIRECTION('ref_axis',(1.,0.,0.));
#30769=DIRECTION('center_axis',(-1.,0.,0.));
#30770=DIRECTION('ref_axis',(0.,0.,1.));
#30771=DIRECTION('center_axis',(1.,0.,0.));
#30772=DIRECTION('ref_axis',(0.,0.,-1.));
#30773=DIRECTION('',(-1.,0.,0.));
#30774=DIRECTION('center_axis',(-1.,0.,0.));
#30775=DIRECTION('ref_axis',(0.,0.,1.));
#30776=DIRECTION('center_axis',(-1.,0.,0.));
#30777=DIRECTION('ref_axis',(0.,0.,1.));
#30778=DIRECTION('center_axis',(1.,0.,0.));
#30779=DIRECTION('ref_axis',(0.,0.,-1.));
#30780=DIRECTION('',(-1.,0.,0.));
#30781=DIRECTION('center_axis',(-1.,0.,0.));
#30782=DIRECTION('ref_axis',(0.,0.,1.));
#30783=DIRECTION('center_axis',(-1.,0.,0.));
#30784=DIRECTION('ref_axis',(0.,0.,1.));
#30785=DIRECTION('center_axis',(1.,0.,0.));
#30786=DIRECTION('ref_axis',(0.,0.,-1.));
#30787=DIRECTION('',(-1.,0.,0.));
#30788=DIRECTION('center_axis',(-1.,0.,0.));
#30789=DIRECTION('ref_axis',(0.,0.,1.));
#30790=DIRECTION('center_axis',(-1.,0.,0.));
#30791=DIRECTION('ref_axis',(0.,0.,1.));
#30792=DIRECTION('center_axis',(1.,0.,0.));
#30793=DIRECTION('ref_axis',(0.,0.,-1.));
#30794=DIRECTION('',(-1.,0.,0.));
#30795=DIRECTION('center_axis',(-1.,0.,0.));
#30796=DIRECTION('ref_axis',(0.,0.,1.));
#30797=DIRECTION('center_axis',(-1.,0.,0.));
#30798=DIRECTION('ref_axis',(0.,0.,1.));
#30799=DIRECTION('center_axis',(1.,0.,0.));
#30800=DIRECTION('ref_axis',(0.,0.,-1.));
#30801=DIRECTION('',(-1.,0.,0.));
#30802=DIRECTION('center_axis',(-1.,0.,0.));
#30803=DIRECTION('ref_axis',(0.,0.,1.));
#30804=DIRECTION('center_axis',(-1.,0.,0.));
#30805=DIRECTION('ref_axis',(0.,0.,1.));
#30806=DIRECTION('center_axis',(1.,0.,0.));
#30807=DIRECTION('ref_axis',(0.,0.,-1.));
#30808=DIRECTION('',(-1.,0.,0.));
#30809=DIRECTION('center_axis',(-1.,0.,0.));
#30810=DIRECTION('ref_axis',(0.,0.,1.));
#30811=DIRECTION('center_axis',(1.,0.,0.));
#30812=DIRECTION('ref_axis',(0.,0.,-1.));
#30813=DIRECTION('center_axis',(1.,0.,0.));
#30814=DIRECTION('ref_axis',(0.,0.,-1.));
#30815=DIRECTION('',(1.,0.,0.));
#30816=DIRECTION('center_axis',(1.,0.,0.));
#30817=DIRECTION('ref_axis',(0.,0.,-1.));
#30818=DIRECTION('center_axis',(1.,0.,0.));
#30819=DIRECTION('ref_axis',(0.,0.,-1.));
#30820=DIRECTION('center_axis',(1.,0.,0.));
#30821=DIRECTION('ref_axis',(0.,0.,-1.));
#30822=DIRECTION('',(1.,0.,0.));
#30823=DIRECTION('center_axis',(1.,0.,0.));
#30824=DIRECTION('ref_axis',(0.,0.,-1.));
#30825=DIRECTION('center_axis',(1.,0.,0.));
#30826=DIRECTION('ref_axis',(0.,0.,-1.));
#30827=DIRECTION('center_axis',(1.,0.,0.));
#30828=DIRECTION('ref_axis',(0.,0.,-1.));
#30829=DIRECTION('',(1.,0.,0.));
#30830=DIRECTION('center_axis',(1.,0.,0.));
#30831=DIRECTION('ref_axis',(0.,0.,-1.));
#30832=DIRECTION('center_axis',(1.,0.,0.));
#30833=DIRECTION('ref_axis',(0.,0.,-1.));
#30834=DIRECTION('center_axis',(1.,0.,0.));
#30835=DIRECTION('ref_axis',(0.,0.,-1.));
#30836=DIRECTION('',(1.,0.,0.));
#30837=DIRECTION('center_axis',(1.,0.,0.));
#30838=DIRECTION('ref_axis',(0.,0.,-1.));
#30839=DIRECTION('center_axis',(1.,0.,0.));
#30840=DIRECTION('ref_axis',(0.,0.,-1.));
#30841=DIRECTION('center_axis',(1.,0.,0.));
#30842=DIRECTION('ref_axis',(0.,0.,-1.));
#30843=DIRECTION('',(1.,0.,0.));
#30844=DIRECTION('center_axis',(1.,0.,0.));
#30845=DIRECTION('ref_axis',(0.,0.,-1.));
#30846=DIRECTION('center_axis',(1.,0.,0.));
#30847=DIRECTION('ref_axis',(0.,0.,-1.));
#30848=DIRECTION('center_axis',(1.,0.,0.));
#30849=DIRECTION('ref_axis',(0.,0.,-1.));
#30850=DIRECTION('',(1.,0.,0.));
#30851=DIRECTION('center_axis',(1.,0.,0.));
#30852=DIRECTION('ref_axis',(0.,0.,-1.));
#30853=DIRECTION('center_axis',(1.,0.,0.));
#30854=DIRECTION('ref_axis',(0.,0.,-1.));
#30855=DIRECTION('center_axis',(1.,0.,0.));
#30856=DIRECTION('ref_axis',(0.,0.,-1.));
#30857=DIRECTION('',(1.,0.,0.));
#30858=DIRECTION('center_axis',(1.,0.,0.));
#30859=DIRECTION('ref_axis',(0.,0.,-1.));
#30860=DIRECTION('center_axis',(1.,0.,0.));
#30861=DIRECTION('ref_axis',(0.,0.,-1.));
#30862=DIRECTION('center_axis',(1.,0.,0.));
#30863=DIRECTION('ref_axis',(0.,0.,-1.));
#30864=DIRECTION('',(1.,0.,0.));
#30865=DIRECTION('center_axis',(1.,0.,0.));
#30866=DIRECTION('ref_axis',(0.,0.,-1.));
#30867=DIRECTION('center_axis',(1.,0.,0.));
#30868=DIRECTION('ref_axis',(0.,0.,-1.));
#30869=DIRECTION('center_axis',(1.,0.,0.));
#30870=DIRECTION('ref_axis',(0.,0.,-1.));
#30871=DIRECTION('',(1.,0.,0.));
#30872=DIRECTION('center_axis',(1.,0.,0.));
#30873=DIRECTION('ref_axis',(0.,0.,-1.));
#30874=DIRECTION('center_axis',(1.,0.,0.));
#30875=DIRECTION('ref_axis',(0.,0.,-1.));
#30876=DIRECTION('center_axis',(1.,0.,0.));
#30877=DIRECTION('ref_axis',(0.,0.,-1.));
#30878=DIRECTION('',(1.,0.,0.));
#30879=DIRECTION('center_axis',(1.,0.,0.));
#30880=DIRECTION('ref_axis',(0.,0.,-1.));
#30881=DIRECTION('center_axis',(1.,0.,0.));
#30882=DIRECTION('ref_axis',(0.,0.,-1.));
#30883=DIRECTION('center_axis',(1.,0.,0.));
#30884=DIRECTION('ref_axis',(0.,0.,-1.));
#30885=DIRECTION('',(1.,0.,0.));
#30886=DIRECTION('center_axis',(1.,0.,0.));
#30887=DIRECTION('ref_axis',(0.,0.,-1.));
#30888=DIRECTION('center_axis',(1.,0.,0.));
#30889=DIRECTION('ref_axis',(0.,0.,-1.));
#30890=DIRECTION('center_axis',(1.,0.,0.));
#30891=DIRECTION('ref_axis',(0.,0.,-1.));
#30892=DIRECTION('',(1.,0.,0.));
#30893=DIRECTION('center_axis',(1.,0.,0.));
#30894=DIRECTION('ref_axis',(0.,0.,-1.));
#30895=DIRECTION('center_axis',(1.,0.,0.));
#30896=DIRECTION('ref_axis',(0.,0.,-1.));
#30897=DIRECTION('center_axis',(1.,0.,0.));
#30898=DIRECTION('ref_axis',(0.,0.,-1.));
#30899=DIRECTION('',(1.,0.,0.));
#30900=DIRECTION('center_axis',(1.,0.,0.));
#30901=DIRECTION('ref_axis',(0.,0.,-1.));
#30902=DIRECTION('center_axis',(1.,0.,0.));
#30903=DIRECTION('ref_axis',(0.,0.,-1.));
#30904=DIRECTION('center_axis',(1.,0.,0.));
#30905=DIRECTION('ref_axis',(0.,0.,-1.));
#30906=DIRECTION('',(1.,0.,0.));
#30907=DIRECTION('center_axis',(1.,0.,0.));
#30908=DIRECTION('ref_axis',(0.,0.,-1.));
#30909=DIRECTION('center_axis',(1.,0.,0.));
#30910=DIRECTION('ref_axis',(0.,0.,-1.));
#30911=DIRECTION('center_axis',(1.,0.,0.));
#30912=DIRECTION('ref_axis',(0.,0.,-1.));
#30913=DIRECTION('',(1.,0.,0.));
#30914=DIRECTION('center_axis',(1.,0.,0.));
#30915=DIRECTION('ref_axis',(0.,0.,-1.));
#30916=DIRECTION('center_axis',(1.,0.,0.));
#30917=DIRECTION('ref_axis',(0.,0.,-1.));
#30918=DIRECTION('center_axis',(1.,0.,0.));
#30919=DIRECTION('ref_axis',(0.,0.,-1.));
#30920=DIRECTION('',(1.,0.,0.));
#30921=DIRECTION('center_axis',(1.,0.,0.));
#30922=DIRECTION('ref_axis',(0.,0.,-1.));
#30923=DIRECTION('center_axis',(1.,0.,0.));
#30924=DIRECTION('ref_axis',(0.,0.,-1.));
#30925=DIRECTION('center_axis',(1.,0.,0.));
#30926=DIRECTION('ref_axis',(0.,0.,-1.));
#30927=DIRECTION('',(1.,0.,0.));
#30928=DIRECTION('center_axis',(1.,0.,0.));
#30929=DIRECTION('ref_axis',(0.,0.,-1.));
#30930=DIRECTION('center_axis',(1.,0.,0.));
#30931=DIRECTION('ref_axis',(0.,0.,-1.));
#30932=DIRECTION('center_axis',(1.,0.,0.));
#30933=DIRECTION('ref_axis',(0.,0.,-1.));
#30934=DIRECTION('',(1.,0.,0.));
#30935=DIRECTION('center_axis',(1.,0.,0.));
#30936=DIRECTION('ref_axis',(0.,0.,-1.));
#30937=DIRECTION('center_axis',(1.,0.,0.));
#30938=DIRECTION('ref_axis',(0.,0.,-1.));
#30939=DIRECTION('center_axis',(1.,0.,0.));
#30940=DIRECTION('ref_axis',(0.,0.,-1.));
#30941=DIRECTION('',(1.,0.,0.));
#30942=DIRECTION('center_axis',(1.,0.,0.));
#30943=DIRECTION('ref_axis',(0.,0.,-1.));
#30944=DIRECTION('center_axis',(1.,0.,0.));
#30945=DIRECTION('ref_axis',(0.,0.,-1.));
#30946=DIRECTION('center_axis',(1.,0.,0.));
#30947=DIRECTION('ref_axis',(0.,0.,-1.));
#30948=DIRECTION('',(1.,0.,0.));
#30949=DIRECTION('center_axis',(1.,0.,0.));
#30950=DIRECTION('ref_axis',(0.,0.,-1.));
#30951=DIRECTION('center_axis',(1.,0.,0.));
#30952=DIRECTION('ref_axis',(0.,0.,-1.));
#30953=DIRECTION('center_axis',(1.,0.,0.));
#30954=DIRECTION('ref_axis',(0.,0.,-1.));
#30955=DIRECTION('',(1.,0.,0.));
#30956=DIRECTION('center_axis',(1.,0.,0.));
#30957=DIRECTION('ref_axis',(0.,0.,-1.));
#30958=DIRECTION('center_axis',(1.,0.,0.));
#30959=DIRECTION('ref_axis',(0.,0.,-1.));
#30960=DIRECTION('center_axis',(1.,0.,0.));
#30961=DIRECTION('ref_axis',(0.,0.,-1.));
#30962=DIRECTION('',(1.,0.,0.));
#30963=DIRECTION('center_axis',(1.,0.,0.));
#30964=DIRECTION('ref_axis',(0.,0.,-1.));
#30965=DIRECTION('center_axis',(1.,0.,0.));
#30966=DIRECTION('ref_axis',(0.,0.,-1.));
#30967=DIRECTION('center_axis',(1.,0.,0.));
#30968=DIRECTION('ref_axis',(0.,0.,-1.));
#30969=DIRECTION('',(1.,0.,0.));
#30970=DIRECTION('center_axis',(1.,0.,0.));
#30971=DIRECTION('ref_axis',(0.,0.,-1.));
#30972=DIRECTION('center_axis',(1.,0.,0.));
#30973=DIRECTION('ref_axis',(0.,0.,-1.));
#30974=DIRECTION('center_axis',(1.,0.,0.));
#30975=DIRECTION('ref_axis',(0.,0.,-1.));
#30976=DIRECTION('',(1.,0.,0.));
#30977=DIRECTION('center_axis',(1.,0.,0.));
#30978=DIRECTION('ref_axis',(0.,0.,-1.));
#30979=DIRECTION('center_axis',(1.,0.,0.));
#30980=DIRECTION('ref_axis',(0.,0.,-1.));
#30981=DIRECTION('center_axis',(1.,0.,0.));
#30982=DIRECTION('ref_axis',(0.,0.,-1.));
#30983=DIRECTION('',(1.,0.,0.));
#30984=DIRECTION('center_axis',(1.,0.,0.));
#30985=DIRECTION('ref_axis',(0.,0.,-1.));
#30986=DIRECTION('center_axis',(1.,0.,0.));
#30987=DIRECTION('ref_axis',(0.,0.,-1.));
#30988=DIRECTION('center_axis',(1.,0.,0.));
#30989=DIRECTION('ref_axis',(0.,0.,-1.));
#30990=DIRECTION('',(1.,0.,0.));
#30991=DIRECTION('center_axis',(1.,0.,0.));
#30992=DIRECTION('ref_axis',(0.,0.,-1.));
#30993=DIRECTION('center_axis',(1.,0.,0.));
#30994=DIRECTION('ref_axis',(0.,0.,-1.));
#30995=DIRECTION('center_axis',(1.,0.,0.));
#30996=DIRECTION('ref_axis',(0.,0.,-1.));
#30997=DIRECTION('',(1.,0.,0.));
#30998=DIRECTION('center_axis',(1.,0.,0.));
#30999=DIRECTION('ref_axis',(0.,0.,-1.));
#31000=DIRECTION('center_axis',(1.,0.,0.));
#31001=DIRECTION('ref_axis',(0.,0.,-1.));
#31002=DIRECTION('center_axis',(1.,0.,0.));
#31003=DIRECTION('ref_axis',(0.,0.,-1.));
#31004=DIRECTION('',(1.,0.,0.));
#31005=DIRECTION('center_axis',(1.,0.,0.));
#31006=DIRECTION('ref_axis',(0.,0.,-1.));
#31007=DIRECTION('center_axis',(1.,0.,0.));
#31008=DIRECTION('ref_axis',(0.,0.,-1.));
#31009=DIRECTION('center_axis',(1.,0.,0.));
#31010=DIRECTION('ref_axis',(0.,0.,-1.));
#31011=DIRECTION('',(1.,0.,0.));
#31012=DIRECTION('center_axis',(1.,0.,0.));
#31013=DIRECTION('ref_axis',(0.,0.,-1.));
#31014=DIRECTION('center_axis',(1.,0.,0.));
#31015=DIRECTION('ref_axis',(0.,0.,-1.));
#31016=DIRECTION('center_axis',(1.,0.,0.));
#31017=DIRECTION('ref_axis',(0.,0.,-1.));
#31018=DIRECTION('',(1.,0.,0.));
#31019=DIRECTION('center_axis',(1.,0.,0.));
#31020=DIRECTION('ref_axis',(0.,0.,-1.));
#31021=DIRECTION('center_axis',(1.,0.,0.));
#31022=DIRECTION('ref_axis',(0.,0.,-1.));
#31023=DIRECTION('center_axis',(1.,0.,0.));
#31024=DIRECTION('ref_axis',(0.,0.,-1.));
#31025=DIRECTION('',(1.,0.,0.));
#31026=DIRECTION('center_axis',(1.,0.,0.));
#31027=DIRECTION('ref_axis',(0.,0.,-1.));
#31028=DIRECTION('center_axis',(1.,0.,0.));
#31029=DIRECTION('ref_axis',(0.,0.,-1.));
#31030=DIRECTION('center_axis',(1.,0.,0.));
#31031=DIRECTION('ref_axis',(0.,0.,-1.));
#31032=DIRECTION('',(1.,0.,0.));
#31033=DIRECTION('center_axis',(1.,0.,0.));
#31034=DIRECTION('ref_axis',(0.,0.,-1.));
#31035=DIRECTION('center_axis',(-1.,-1.73472347597681E-16,0.));
#31036=DIRECTION('ref_axis',(1.73472347597681E-16,-1.,0.));
#31037=DIRECTION('',(0.,1.,1.18952466924124E-16));
#31038=DIRECTION('',(1.2266347333467E-16,-0.707106781186546,0.707106781186549));
#31039=DIRECTION('',(0.,1.26161707343768E-16,-1.));
#31040=DIRECTION('',(-1.2266347333467E-16,0.70710678118655,0.707106781186545));
#31041=DIRECTION('',(0.,-1.,-1.58603289232165E-16));
#31042=DIRECTION('',(-1.2266347333467E-16,0.707106781186546,-0.707106781186548));
#31043=DIRECTION('',(0.,0.,1.));
#31044=DIRECTION('',(1.2266347333467E-16,-0.70710678118655,-0.707106781186545));
#31045=DIRECTION('center_axis',(0.,1.,0.));
#31046=DIRECTION('ref_axis',(0.,0.,1.));
#31047=DIRECTION('',(1.,0.,0.));
#31048=DIRECTION('',(0.,0.,1.));
#31049=DIRECTION('',(1.,0.,0.));
#31050=DIRECTION('',(0.,0.,-1.));
#31051=DIRECTION('center_axis',(-1.,0.,0.));
#31052=DIRECTION('ref_axis',(0.,0.,1.));
#31053=DIRECTION('',(0.,1.,0.));
#31054=DIRECTION('',(0.,0.,-1.));
#31055=DIRECTION('',(0.,1.,0.));
#31056=DIRECTION('',(0.,0.,1.));
#31057=DIRECTION('center_axis',(0.,1.,0.));
#31058=DIRECTION('ref_axis',(0.,0.,1.));
#31059=DIRECTION('',(1.,0.,0.));
#31060=DIRECTION('',(0.,0.,-1.));
#31061=DIRECTION('',(1.,0.,0.));
#31062=DIRECTION('',(0.,0.,-1.));
#31063=DIRECTION('center_axis',(0.,0.,-1.));
#31064=DIRECTION('ref_axis',(-1.,0.,0.));
#31065=DIRECTION('',(0.707106781186548,0.707106781186547,0.));
#31066=DIRECTION('',(-0.707106781186546,0.707106781186549,0.));
#31067=DIRECTION('',(0.,-1.,0.));
#31068=DIRECTION('',(1.,0.,0.));
#31069=DIRECTION('',(-1.,0.,0.));
#31070=DIRECTION('center_axis',(0.,0.,1.));
#31071=DIRECTION('ref_axis',(-1.,0.,0.));
#31072=DIRECTION('center_axis',(0.,0.,-1.));
#31073=DIRECTION('ref_axis',(-1.,0.,0.));
#31074=DIRECTION('',(-0.707106781186548,-0.707106781186547,0.));
#31075=DIRECTION('',(0.,-1.,0.));
#31076=DIRECTION('',(0.707106781186546,-0.707106781186549,0.));
#31077=DIRECTION('',(-1.,0.,0.));
#31078=DIRECTION('center_axis',(0.,0.,-1.));
#31079=DIRECTION('ref_axis',(-1.,0.,0.));
#31080=DIRECTION('',(1.,0.,0.));
#31081=DIRECTION('center_axis',(1.,0.,0.));
#31082=DIRECTION('ref_axis',(0.,0.,-1.));
#31083=DIRECTION('',(0.,1.26161707343768E-16,-1.));
#31084=DIRECTION('',(0.,0.707106781186546,-0.707106781186549));
#31085=DIRECTION('',(0.,1.,1.18952466924124E-16));
#31086=DIRECTION('',(0.,0.70710678118655,0.707106781186545));
#31087=DIRECTION('',(0.,0.,1.));
#31088=DIRECTION('',(0.,-0.707106781186546,0.707106781186548));
#31089=DIRECTION('',(0.,-1.,-1.58603289232165E-16));
#31090=DIRECTION('',(0.,-0.70710678118655,-0.707106781186545));
#31091=DIRECTION('center_axis',(0.,-1.18952466924124E-16,1.));
#31092=DIRECTION('ref_axis',(0.,-1.,-1.18952466924124E-16));
#31093=DIRECTION('',(-1.,0.,0.));
#31094=DIRECTION('',(1.,0.,0.));
#31095=DIRECTION('center_axis',(0.,-1.,0.));
#31096=DIRECTION('ref_axis',(0.,0.,-1.));
#31097=DIRECTION('',(1.,0.,0.));
#31098=DIRECTION('',(-1.,0.,0.));
#31099=DIRECTION('center_axis',(0.,1.58603289232165E-16,-1.));
#31100=DIRECTION('ref_axis',(0.,1.,1.58603289232165E-16));
#31101=DIRECTION('',(1.,0.,0.));
#31102=DIRECTION('',(-1.,0.,0.));
#31103=DIRECTION('center_axis',(0.,1.,1.26161707343768E-16));
#31104=DIRECTION('ref_axis',(0.,-1.26161707343768E-16,1.));
#31105=DIRECTION('',(1.,0.,0.));
#31106=DIRECTION('',(-1.,0.,0.));
#31107=DIRECTION('center_axis',(-1.,0.,0.));
#31108=DIRECTION('ref_axis',(0.,0.,1.));
#31109=DIRECTION('center_axis',(-1.,0.,0.));
#31110=DIRECTION('ref_axis',(0.,0.,1.));
#31111=DIRECTION('center_axis',(-1.,0.,0.));
#31112=DIRECTION('ref_axis',(0.,0.,1.));
#31113=DIRECTION('center_axis',(-1.,0.,0.));
#31114=DIRECTION('ref_axis',(0.,0.,1.));
#31115=DIRECTION('center_axis',(-1.,0.,0.));
#31116=DIRECTION('ref_axis',(0.,0.,1.));
#31117=DIRECTION('center_axis',(-1.,0.,0.));
#31118=DIRECTION('ref_axis',(0.,0.,1.));
#31119=DIRECTION('center_axis',(-1.,0.,0.));
#31120=DIRECTION('ref_axis',(0.,0.,1.));
#31121=DIRECTION('center_axis',(-1.,0.,0.));
#31122=DIRECTION('ref_axis',(0.,0.,1.));
#31123=DIRECTION('center_axis',(-1.,0.,0.));
#31124=DIRECTION('ref_axis',(0.,0.,1.));
#31125=DIRECTION('center_axis',(-1.,0.,0.));
#31126=DIRECTION('ref_axis',(0.,0.,1.));
#31127=DIRECTION('center_axis',(-1.,0.,0.));
#31128=DIRECTION('ref_axis',(0.,0.,1.));
#31129=DIRECTION('center_axis',(-1.,0.,0.));
#31130=DIRECTION('ref_axis',(0.,0.,1.));
#31131=DIRECTION('center_axis',(-1.,0.,0.));
#31132=DIRECTION('ref_axis',(0.,0.,1.));
#31133=DIRECTION('center_axis',(-1.,0.,0.));
#31134=DIRECTION('ref_axis',(0.,0.,1.));
#31135=DIRECTION('center_axis',(-1.,0.,0.));
#31136=DIRECTION('ref_axis',(0.,0.,1.));
#31137=DIRECTION('center_axis',(-1.,0.,0.));
#31138=DIRECTION('ref_axis',(0.,0.,1.));
#31139=DIRECTION('center_axis',(0.,0.,1.));
#31140=DIRECTION('ref_axis',(1.,0.,0.));
#31141=DIRECTION('center_axis',(-0.707106781186547,0.707106781186548,0.));
#31142=DIRECTION('ref_axis',(0.,0.,-1.));
#31143=DIRECTION('center_axis',(0.707106781186549,0.707106781186546,0.));
#31144=DIRECTION('ref_axis',(0.,0.,1.));
#31145=DIRECTION('center_axis',(0.,-1.,0.));
#31146=DIRECTION('ref_axis',(0.,0.,-1.));
#31147=DIRECTION('',(0.,0.,-1.));
#31148=DIRECTION('center_axis',(0.,1.,0.));
#31149=DIRECTION('ref_axis',(0.,0.,1.));
#31150=DIRECTION('',(0.,0.,-1.));
#31151=DIRECTION('center_axis',(0.,0.,-1.));
#31152=DIRECTION('ref_axis',(1.,1.22464679914735E-16,0.));
#31153=DIRECTION('center_axis',(0.,0.707106781186549,0.707106781186546));
#31154=DIRECTION('ref_axis',(-1.,0.,0.));
#31155=DIRECTION('center_axis',(0.,0.707106781186545,-0.70710678118655));
#31156=DIRECTION('ref_axis',(-1.,0.,0.));
#31157=DIRECTION('center_axis',(0.,-0.707106781186549,-0.707106781186547));
#31158=DIRECTION('ref_axis',(-1.,0.,0.));
#31159=DIRECTION('center_axis',(0.,-0.707106781186545,0.70710678118655));
#31160=DIRECTION('ref_axis',(-1.,0.,0.));
#31161=DIRECTION('axis',(0.,0.,1.));
#31162=DIRECTION('refdir',(1.,0.,0.));
#31163=DIRECTION('axis',(0.,0.,1.));
#31164=DIRECTION('refdir',(1.,0.,0.));
#31165=DIRECTION('center_axis',(0.,1.,0.));
#31166=DIRECTION('ref_axis',(0.,0.,1.));
#31167=DIRECTION('center_axis',(0.,1.,0.));
#31168=DIRECTION('ref_axis',(0.,0.,1.));
#31169=DIRECTION('',(0.,1.,0.));
#31170=DIRECTION('center_axis',(0.,1.,0.));
#31171=DIRECTION('ref_axis',(0.,0.,1.));
#31172=DIRECTION('center_axis',(0.,1.,0.));
#31173=DIRECTION('ref_axis',(0.,0.,1.));
#31174=DIRECTION('center_axis',(6.19544098563146E-17,1.,0.));
#31175=DIRECTION('ref_axis',(-1.,6.19544098563145E-17,0.));
#31176=DIRECTION('center_axis',(-0.707106781186515,0.70710678118658,-8.91973620485813E-14));
#31177=DIRECTION('ref_axis',(0.70710678118658,0.707106781186515,-4.06869792218931E-9));
#31178=DIRECTION('center_axis',(0.,1.,0.));
#31179=DIRECTION('ref_axis',(0.,0.,1.));
#31180=DIRECTION('center_axis',(-0.707106781186512,0.707106781186583,1.02279641815266E-13));
#31181=DIRECTION('ref_axis',(0.707106781186583,0.707106781186512,-1.02741687219779E-8));
#31182=DIRECTION('center_axis',(6.19544098563146E-17,1.,0.));
#31183=DIRECTION('ref_axis',(-1.,6.19544098563145E-17,0.));
#31184=DIRECTION('',(0.,1.,0.));
#31185=DIRECTION('center_axis',(0.,1.,0.));
#31186=DIRECTION('ref_axis',(0.,0.,1.));
#31187=DIRECTION('center_axis',(6.19544098563146E-17,1.,0.));
#31188=DIRECTION('ref_axis',(-1.,6.19544098563145E-17,0.));
#31189=DIRECTION('center_axis',(0.707106781186576,0.707106781186519,-7.49257841204838E-14));
#31190=DIRECTION('ref_axis',(0.707106781186519,-0.707106781186576,-8.08586735251008E-9));
#31191=DIRECTION('center_axis',(0.,1.,0.));
#31192=DIRECTION('ref_axis',(0.,0.,1.));
#31193=DIRECTION('center_axis',(0.707106781186584,0.707106781186511,9.99010454948653E-14));
#31194=DIRECTION('ref_axis',(0.707106781186511,-0.707106781186585,-3.84531478187653E-9));
#31195=DIRECTION('center_axis',(0.,1.,0.));
#31196=DIRECTION('ref_axis',(0.,0.,1.));
#31197=DIRECTION('center_axis',(0.,1.,0.));
#31198=DIRECTION('ref_axis',(0.,0.,1.));
#31199=DIRECTION('',(0.,1.,0.));
#31200=DIRECTION('center_axis',(0.,1.,0.));
#31201=DIRECTION('ref_axis',(0.,0.,1.));
#31202=DIRECTION('center_axis',(0.,1.,0.));
#31203=DIRECTION('ref_axis',(0.,0.,1.));
#31204=DIRECTION('center_axis',(6.19544098563146E-17,1.,0.));
#31205=DIRECTION('ref_axis',(-1.,6.19544098563145E-17,0.));
#31206=DIRECTION('center_axis',(-0.707106781186517,0.707106781186578,-8.56294675662794E-14));
#31207=DIRECTION('ref_axis',(0.707106781186578,0.707106781186517,6.04191337821136E-9));
#31208=DIRECTION('center_axis',(0.,1.,0.));
#31209=DIRECTION('ref_axis',(0.,0.,1.));
#31210=DIRECTION('center_axis',(-0.707106781186516,0.707106781186579,8.80080638879547E-14));
#31211=DIRECTION('ref_axis',(0.707106781186579,0.707106781186516,-1.3593282001024E-10));
#31212=DIRECTION('center_axis',(6.19544098563146E-17,1.,0.));
#31213=DIRECTION('ref_axis',(-1.,6.19544098563145E-17,0.));
#31214=DIRECTION('',(0.,1.,0.));
#31215=DIRECTION('center_axis',(0.,1.,0.));
#31216=DIRECTION('ref_axis',(0.,0.,1.));
#31217=DIRECTION('center_axis',(6.19544098563146E-17,1.,0.));
#31218=DIRECTION('ref_axis',(-1.,6.19544098563145E-17,0.));
#31219=DIRECTION('center_axis',(0.707106781186558,0.707106781186537,-1.42715779277089E-14));
#31220=DIRECTION('ref_axis',(0.707106781186537,-0.707106781186558,-6.58917923406118E-10));
#31221=DIRECTION('center_axis',(0.,1.,0.));
#31222=DIRECTION('ref_axis',(0.,0.,1.));
#31223=DIRECTION('center_axis',(0.70710678118656,0.707106781186535,2.37859632128526E-14));
#31224=DIRECTION('ref_axis',(0.707106781186535,-0.70710678118656,1.32329140713553E-8));
#31225=DIRECTION('center_axis',(0.,1.,0.));
#31226=DIRECTION('ref_axis',(0.,0.,1.));
#31227=DIRECTION('center_axis',(0.,1.,0.));
#31228=DIRECTION('ref_axis',(0.,0.,1.));
#31229=DIRECTION('',(0.,1.,0.));
#31230=DIRECTION('center_axis',(0.,1.,0.));
#31231=DIRECTION('ref_axis',(0.,0.,1.));
#31232=DIRECTION('center_axis',(0.,1.,0.));
#31233=DIRECTION('ref_axis',(0.,0.,1.));
#31234=DIRECTION('center_axis',(6.19544098563146E-17,1.,0.));
#31235=DIRECTION('ref_axis',(-1.,6.19544098563145E-17,0.));
#31236=DIRECTION('center_axis',(-0.707106781186517,0.707106781186578,-8.56294675664632E-14));
#31237=DIRECTION('ref_axis',(0.707106781186578,0.707106781186517,2.05409793046914E-10));
#31238=DIRECTION('center_axis',(0.,1.,0.));
#31239=DIRECTION('ref_axis',(0.,0.,1.));
#31240=DIRECTION('center_axis',(-0.707106781186514,0.707106781186581,9.51438528521397E-14));
#31241=DIRECTION('ref_axis',(0.707106781186581,0.707106781186514,-1.68463230688698E-9));
#31242=DIRECTION('center_axis',(6.19544098563146E-17,1.,0.));
#31243=DIRECTION('ref_axis',(-1.,6.19544098563145E-17,0.));
#31244=DIRECTION('',(0.,1.,0.));
#31245=DIRECTION('center_axis',(0.,1.,0.));
#31246=DIRECTION('ref_axis',(0.,0.,1.));
#31247=DIRECTION('center_axis',(6.19544098563146E-17,1.,0.));
#31248=DIRECTION('ref_axis',(-1.,6.19544098563145E-17,0.));
#31249=DIRECTION('center_axis',(0.707106781186562,0.707106781186533,-2.7353857695029E-14));
#31250=DIRECTION('ref_axis',(0.707106781186533,-0.707106781186562,3.81701637658264E-9));
#31251=DIRECTION('center_axis',(0.,1.,0.));
#31252=DIRECTION('ref_axis',(0.,0.,1.));
#31253=DIRECTION('center_axis',(0.707106781186559,0.707106781186536,1.90287705704185E-14));
#31254=DIRECTION('ref_axis',(0.707106781186536,-0.707106781186559,-1.36144986195536E-8));
#31255=DIRECTION('center_axis',(0.,1.,0.));
#31256=DIRECTION('ref_axis',(0.,0.,1.));
#31257=DIRECTION('center_axis',(0.,1.,0.));
#31258=DIRECTION('ref_axis',(0.,0.,1.));
#31259=DIRECTION('',(0.,1.,0.));
#31260=DIRECTION('center_axis',(0.,1.,0.));
#31261=DIRECTION('ref_axis',(0.,0.,1.));
#31262=DIRECTION('center_axis',(0.,1.,0.));
#31263=DIRECTION('ref_axis',(0.,0.,1.));
#31264=DIRECTION('center_axis',(6.19544098563146E-17,1.,0.));
#31265=DIRECTION('ref_axis',(-1.,6.19544098563145E-17,0.));
#31266=DIRECTION('center_axis',(-0.707106781186512,0.707106781186583,-1.01090343655035E-13));
#31267=DIRECTION('ref_axis',(0.707106781186583,0.707106781186512,-6.95106205771872E-9));
#31268=DIRECTION('center_axis',(0.,1.,0.));
#31269=DIRECTION('ref_axis',(0.,0.,1.));
#31270=DIRECTION('center_axis',(-0.707106781186507,0.707106781186588,1.11794027100389E-13));
#31271=DIRECTION('ref_axis',(0.707106781186588,0.707106781186507,-1.20597831914651E-9));
#31272=DIRECTION('center_axis',(6.19544098563146E-17,1.,0.));
#31273=DIRECTION('ref_axis',(-1.,6.19544098563145E-17,0.));
#31274=DIRECTION('',(0.,1.,0.));
#31275=DIRECTION('center_axis',(0.,1.,0.));
#31276=DIRECTION('ref_axis',(0.,0.,1.));
#31277=DIRECTION('center_axis',(6.19544098563146E-17,1.,0.));
#31278=DIRECTION('ref_axis',(-1.,6.19544098563145E-17,0.));
#31279=DIRECTION('center_axis',(0.707106781186587,0.707106781186508,-1.03468939976327E-13));
#31280=DIRECTION('ref_axis',(0.707106781186508,-0.707106781186587,-1.2458919406139E-9));
#31281=DIRECTION('center_axis',(0.,1.,0.));
#31282=DIRECTION('ref_axis',(0.,0.,1.));
#31283=DIRECTION('center_axis',(0.707106781186591,0.707106781186504,1.21308412386573E-13));
#31284=DIRECTION('ref_axis',(0.707106781186504,-0.707106781186591,-3.13413565581154E-9));
#31285=DIRECTION('center_axis',(0.,1.,0.));
#31286=DIRECTION('ref_axis',(0.,0.,1.));
#31287=DIRECTION('center_axis',(0.,1.,0.));
#31288=DIRECTION('ref_axis',(0.,0.,1.));
#31289=DIRECTION('',(0.,1.,0.));
#31290=DIRECTION('center_axis',(0.,1.,0.));
#31291=DIRECTION('ref_axis',(0.,0.,1.));
#31292=DIRECTION('center_axis',(0.,1.,0.));
#31293=DIRECTION('ref_axis',(0.,0.,1.));
#31294=DIRECTION('center_axis',(6.19544098563146E-17,1.,0.));
#31295=DIRECTION('ref_axis',(-1.,6.19544098563145E-17,0.));
#31296=DIRECTION('center_axis',(-0.707106781186512,0.707106781186583,-1.01090343655035E-13));
#31297=DIRECTION('ref_axis',(0.707106781186583,0.707106781186512,-4.84274768749914E-9));
#31298=DIRECTION('center_axis',(0.,1.,0.));
#31299=DIRECTION('ref_axis',(0.,0.,1.));
#31300=DIRECTION('center_axis',(-0.707106781186507,0.707106781186588,1.11794027100512E-13));
#31301=DIRECTION('ref_axis',(0.707106781186588,0.707106781186507,-5.79440054969364E-10));
#31302=DIRECTION('center_axis',(6.19544098563146E-17,1.,0.));
#31303=DIRECTION('ref_axis',(-1.,6.19544098563145E-17,0.));
#31304=DIRECTION('',(0.,1.,0.));
#31305=DIRECTION('center_axis',(0.,1.,0.));
#31306=DIRECTION('ref_axis',(0.,0.,1.));
#31307=DIRECTION('center_axis',(6.19544098563146E-17,1.,0.));
#31308=DIRECTION('ref_axis',(-1.,6.19544098563145E-17,0.));
#31309=DIRECTION('center_axis',(0.707106781186572,0.707106781186523,-6.06542061931958E-14));
#31310=DIRECTION('ref_axis',(0.707106781186523,-0.707106781186572,-4.16681478047922E-10));
#31311=DIRECTION('center_axis',(0.,1.,0.));
#31312=DIRECTION('ref_axis',(0.,0.,1.));
#31313=DIRECTION('center_axis',(0.707106781186573,0.707106781186523,5.94649080322994E-14));
#31314=DIRECTION('ref_axis',(0.707106781186522,-0.707106781186572,-7.07966748929713E-9));
#31315=DIRECTION('center_axis',(0.,1.,0.));
#31316=DIRECTION('ref_axis',(0.,0.,1.));
#31317=DIRECTION('center_axis',(0.,1.,0.));
#31318=DIRECTION('ref_axis',(0.,0.,1.));
#31319=DIRECTION('',(0.,1.,0.));
#31320=DIRECTION('center_axis',(0.,1.,0.));
#31321=DIRECTION('ref_axis',(0.,0.,1.));
#31322=DIRECTION('center_axis',(0.,1.,0.));
#31323=DIRECTION('ref_axis',(0.,0.,1.));
#31324=DIRECTION('center_axis',(6.19544098563146E-17,1.,0.));
#31325=DIRECTION('ref_axis',(-1.,6.19544098563145E-17,0.));
#31326=DIRECTION('center_axis',(-0.707106781186512,0.707106781186583,-9.75224491731711E-14));
#31327=DIRECTION('ref_axis',(0.707106781186583,0.707106781186512,8.28098005345847E-10));
#31328=DIRECTION('center_axis',(0.,1.,0.));
#31329=DIRECTION('ref_axis',(0.,0.,1.));
#31330=DIRECTION('center_axis',(-0.707106781186517,0.707106781186578,8.80080638877943E-14));
#31331=DIRECTION('ref_axis',(0.707106781186578,0.707106781186517,2.21337779031319E-9));
#31332=DIRECTION('center_axis',(6.19544098563146E-17,1.,0.));
#31333=DIRECTION('ref_axis',(-1.,6.19544098563145E-17,0.));
#31334=DIRECTION('',(0.,1.,0.));
#31335=DIRECTION('center_axis',(0.,1.,0.));
#31336=DIRECTION('ref_axis',(0.,0.,1.));
#31337=DIRECTION('center_axis',(6.19544098563146E-17,1.,0.));
#31338=DIRECTION('ref_axis',(-1.,6.19544098563145E-17,0.));
#31339=DIRECTION('center_axis',(0.707106781186559,0.707106781186536,-1.54608760884523E-14));
#31340=DIRECTION('ref_axis',(0.707106781186536,-0.707106781186559,-3.73251907398984E-10));
#31341=DIRECTION('center_axis',(0.,1.,0.));
#31342=DIRECTION('ref_axis',(0.,0.,1.));
#31343=DIRECTION('center_axis',(0.707106781186559,0.707106781186536,2.14073668916763E-14));
#31344=DIRECTION('ref_axis',(0.707106781186536,-0.707106781186559,-2.78541967759128E-9));
#31345=DIRECTION('center_axis',(0.,1.,0.));
#31346=DIRECTION('ref_axis',(0.,0.,1.));
#31347=DIRECTION('center_axis',(0.,1.,0.));
#31348=DIRECTION('ref_axis',(0.,0.,1.));
#31349=DIRECTION('',(0.,1.,0.));
#31350=DIRECTION('center_axis',(0.,1.,0.));
#31351=DIRECTION('ref_axis',(0.,0.,1.));
#31352=DIRECTION('center_axis',(0.,1.,0.));
#31353=DIRECTION('ref_axis',(0.,0.,1.));
#31354=DIRECTION('center_axis',(6.19544098563146E-17,1.,0.));
#31355=DIRECTION('ref_axis',(-1.,6.19544098563145E-17,0.));
#31356=DIRECTION('center_axis',(-0.707106781186531,0.707106781186564,-3.68682429800858E-14));
#31357=DIRECTION('ref_axis',(0.707106781186564,0.707106781186531,1.74894276284856E-9));
#31358=DIRECTION('center_axis',(0.,1.,0.));
#31359=DIRECTION('ref_axis',(0.,0.,1.));
#31360=DIRECTION('center_axis',(-0.707106781186539,0.707106781186556,1.90287705703503E-14));
#31361=DIRECTION('ref_axis',(0.707106781186556,0.707106781186538,1.53190884165236E-9));
#31362=DIRECTION('center_axis',(6.19544098563146E-17,1.,0.));
#31363=DIRECTION('ref_axis',(-1.,6.19544098563145E-17,0.));
#31364=DIRECTION('',(0.,1.,0.));
#31365=DIRECTION('center_axis',(0.,1.,0.));
#31366=DIRECTION('ref_axis',(0.,0.,1.));
#31367=DIRECTION('center_axis',(6.19544098563146E-17,1.,0.));
#31368=DIRECTION('ref_axis',(-1.,6.19544098563145E-17,0.));
#31369=DIRECTION('center_axis',(0.707106781186565,0.70710678118653,-3.68682429801788E-14));
#31370=DIRECTION('ref_axis',(0.70710678118653,-0.707106781186565,-1.95898017545691E-10));
#31371=DIRECTION('center_axis',(0.,1.,0.));
#31372=DIRECTION('ref_axis',(0.,0.,1.));
#31373=DIRECTION('center_axis',(0.707106781186568,0.707106781186527,4.28147337832366E-14));
#31374=DIRECTION('ref_axis',(0.707106781186527,-0.707106781186568,-6.13326237593097E-11));
#31375=DIRECTION('center_axis',(0.,1.,0.));
#31376=DIRECTION('ref_axis',(0.,0.,1.));
#31377=DIRECTION('center_axis',(0.,1.,0.));
#31378=DIRECTION('ref_axis',(0.,0.,1.));
#31379=DIRECTION('',(0.,1.,0.));
#31380=DIRECTION('center_axis',(0.,1.,0.));
#31381=DIRECTION('ref_axis',(0.,0.,1.));
#31382=DIRECTION('center_axis',(0.,1.,0.));
#31383=DIRECTION('ref_axis',(0.,0.,1.));
#31384=DIRECTION('center_axis',(6.19544098563146E-17,1.,0.));
#31385=DIRECTION('ref_axis',(-1.,6.19544098563145E-17,0.));
#31386=DIRECTION('center_axis',(-0.707106781186525,0.70710678118657,-5.58970135504356E-14));
#31387=DIRECTION('ref_axis',(0.70710678118657,0.707106781186525,-2.27753512105411E-11));
#31388=DIRECTION('center_axis',(0.,1.,0.));
#31389=DIRECTION('ref_axis',(0.,0.,1.));
#31390=DIRECTION('center_axis',(-0.707106781186534,0.707106781186561,3.09217521768369E-14));
#31391=DIRECTION('ref_axis',(0.707106781186561,0.707106781186534,4.69170049623784E-11));
#31392=DIRECTION('center_axis',(6.19544098563146E-17,1.,0.));
#31393=DIRECTION('ref_axis',(-1.,6.19544098563145E-17,0.));
#31394=DIRECTION('',(0.,1.,0.));
#31395=DIRECTION('center_axis',(0.,1.,0.));
#31396=DIRECTION('ref_axis',(0.,0.,1.));
#31397=DIRECTION('center_axis',(6.19544098563146E-17,1.,0.));
#31398=DIRECTION('ref_axis',(-1.,6.19544098563145E-17,0.));
#31399=DIRECTION('center_axis',(0.707106781186567,0.707106781186528,-3.8057541140834E-14));
#31400=DIRECTION('ref_axis',(0.707106781186528,-0.707106781186567,-3.28609365367872E-11));
#31401=DIRECTION('center_axis',(0.,1.,0.));
#31402=DIRECTION('ref_axis',(0.,0.,1.));
#31403=DIRECTION('center_axis',(0.707106781186564,0.707106781186531,3.3300348498065E-14));
#31404=DIRECTION('ref_axis',(0.707106781186531,-0.707106781186564,-8.01952541386524E-13));
#31405=DIRECTION('center_axis',(-0.707106781186544,0.707106781186551,0.));
#31406=DIRECTION('ref_axis',(-0.707106781186551,-0.707106781186544,0.));
#31407=DIRECTION('',(0.,0.,1.));
#31408=DIRECTION('',(0.,0.,1.));
#31409=DIRECTION('',(-0.707106781186551,-0.707106781186544,0.));
#31410=DIRECTION('center_axis',(6.19544098563146E-17,1.,0.));
#31411=DIRECTION('ref_axis',(-1.,6.19544098563146E-17,0.));
#31412=DIRECTION('',(0.,0.,1.));
#31413=DIRECTION('',(0.,0.,1.));
#31414=DIRECTION('center_axis',(0.707106781186551,0.707106781186544,0.));
#31415=DIRECTION('ref_axis',(-0.707106781186544,0.707106781186551,0.));
#31416=DIRECTION('',(0.,0.,1.));
#31417=DIRECTION('center_axis',(1.22464679914735E-16,-1.,0.));
#31418=DIRECTION('ref_axis',(1.,1.22464679914735E-16,0.));
#31419=DIRECTION('',(0.,0.,1.));
#31420=DIRECTION('',(0.,0.,1.));
#31421=DIRECTION('',(0.,0.,1.));
#31422=DIRECTION('',(0.,0.,1.));
#31423=DIRECTION('',(0.,0.,1.));
#31424=DIRECTION('',(0.,0.,1.));
#31425=DIRECTION('',(0.,0.,1.));
#31426=DIRECTION('',(0.,0.,1.));
#31427=DIRECTION('',(1.,1.22464679914735E-16,0.));
#31428=DIRECTION('',(0.,0.,1.));
#31429=DIRECTION('',(1.,1.22464679914735E-16,0.));
#31430=DIRECTION('center_axis',(1.22464679914735E-16,-1.,0.));
#31431=DIRECTION('ref_axis',(1.,1.22464679914735E-16,0.));
#31432=DIRECTION('',(0.,0.,1.));
#31433=DIRECTION('',(1.,1.22464679914735E-16,0.));
#31434=DIRECTION('',(0.,0.,1.));
#31435=DIRECTION('',(1.,1.22464679914735E-16,0.));
#31436=DIRECTION('',(0.,0.,1.));
#31437=DIRECTION('',(0.,0.,1.));
#31438=DIRECTION('',(0.,0.,1.));
#31439=DIRECTION('',(0.,0.,1.));
#31440=DIRECTION('',(0.,0.,1.));
#31441=DIRECTION('',(0.,0.,1.));
#31442=DIRECTION('',(0.,0.,1.));
#31443=DIRECTION('center_axis',(-0.707106781186544,0.707106781186551,0.));
#31444=DIRECTION('ref_axis',(-0.707106781186551,-0.707106781186544,0.));
#31445=DIRECTION('center_axis',(6.19544098563146E-17,1.,0.));
#31446=DIRECTION('ref_axis',(-1.,6.19544098563146E-17,0.));
#31447=DIRECTION('',(0.,0.,1.));
#31448=DIRECTION('',(0.,0.,1.));
#31449=DIRECTION('center_axis',(0.707106781186551,0.707106781186544,0.));
#31450=DIRECTION('ref_axis',(-0.707106781186544,0.707106781186551,0.));
#31451=DIRECTION('center_axis',(-0.707106781186544,0.707106781186551,0.));
#31452=DIRECTION('ref_axis',(-0.707106781186551,-0.707106781186544,0.));
#31453=DIRECTION('center_axis',(6.19544098563146E-17,1.,0.));
#31454=DIRECTION('ref_axis',(-1.,6.19544098563146E-17,0.));
#31455=DIRECTION('',(0.,0.,1.));
#31456=DIRECTION('',(0.,0.,1.));
#31457=DIRECTION('center_axis',(0.707106781186551,0.707106781186544,0.));
#31458=DIRECTION('ref_axis',(-0.707106781186544,0.707106781186551,0.));
#31459=DIRECTION('center_axis',(-0.707106781186544,0.707106781186551,0.));
#31460=DIRECTION('ref_axis',(-0.707106781186551,-0.707106781186544,0.));
#31461=DIRECTION('center_axis',(0.707106781186551,0.707106781186544,0.));
#31462=DIRECTION('ref_axis',(-0.707106781186544,0.707106781186551,0.));
#31463=DIRECTION('',(0.,0.,1.));
#31464=DIRECTION('center_axis',(6.19544098563146E-17,1.,0.));
#31465=DIRECTION('ref_axis',(-1.,6.19544098563146E-17,0.));
#31466=DIRECTION('',(0.,0.,1.));
#31467=DIRECTION('center_axis',(-0.707106781186544,0.707106781186551,0.));
#31468=DIRECTION('ref_axis',(-0.707106781186551,-0.707106781186544,0.));
#31469=DIRECTION('center_axis',(6.19544098563146E-17,1.,0.));
#31470=DIRECTION('ref_axis',(-1.,6.19544098563146E-17,0.));
#31471=DIRECTION('',(0.,0.,1.));
#31472=DIRECTION('',(0.,0.,1.));
#31473=DIRECTION('center_axis',(0.707106781186551,0.707106781186544,0.));
#31474=DIRECTION('ref_axis',(-0.707106781186544,0.707106781186551,0.));
#31475=DIRECTION('center_axis',(-0.707106781186544,0.707106781186551,0.));
#31476=DIRECTION('ref_axis',(-0.707106781186551,-0.707106781186544,0.));
#31477=DIRECTION('center_axis',(6.19544098563146E-17,1.,0.));
#31478=DIRECTION('ref_axis',(-1.,6.19544098563146E-17,0.));
#31479=DIRECTION('',(0.,0.,1.));
#31480=DIRECTION('',(0.,0.,1.));
#31481=DIRECTION('center_axis',(0.707106781186551,0.707106781186544,0.));
#31482=DIRECTION('ref_axis',(-0.707106781186544,0.707106781186551,0.));
#31483=DIRECTION('center_axis',(-0.707106781186544,0.707106781186551,0.));
#31484=DIRECTION('ref_axis',(-0.707106781186551,-0.707106781186544,0.));
#31485=DIRECTION('center_axis',(6.19544098563146E-17,1.,0.));
#31486=DIRECTION('ref_axis',(-1.,6.19544098563146E-17,0.));
#31487=DIRECTION('',(0.,0.,1.));
#31488=DIRECTION('',(0.,0.,1.));
#31489=DIRECTION('center_axis',(0.707106781186551,0.707106781186544,0.));
#31490=DIRECTION('ref_axis',(-0.707106781186544,0.707106781186551,0.));
#31491=DIRECTION('center_axis',(-0.707106781186544,0.707106781186551,0.));
#31492=DIRECTION('ref_axis',(-0.707106781186551,-0.707106781186544,0.));
#31493=DIRECTION('center_axis',(6.19544098563146E-17,1.,0.));
#31494=DIRECTION('ref_axis',(-1.,6.19544098563146E-17,0.));
#31495=DIRECTION('',(0.,0.,1.));
#31496=DIRECTION('',(0.,0.,1.));
#31497=DIRECTION('',(-1.,6.19544098563146E-17,0.));
#31498=DIRECTION('center_axis',(0.707106781186551,0.707106781186544,0.));
#31499=DIRECTION('ref_axis',(-0.707106781186544,0.707106781186551,0.));
#31500=DIRECTION('',(-0.707106781186544,0.707106781186551,0.));
#31501=DIRECTION('center_axis',(0.,0.,-1.));
#31502=DIRECTION('ref_axis',(-1.,0.,0.));
#31503=DIRECTION('',(0.707106781186544,-0.707106781186551,0.));
#31504=DIRECTION('',(0.,-1.,0.));
#31505=DIRECTION('center_axis',(0.,0.,-1.));
#31506=DIRECTION('ref_axis',(-1.,0.,0.));
#31507=DIRECTION('',(-0.707106781186551,-0.707106781186544,0.));
#31508=DIRECTION('center_axis',(0.,0.,1.));
#31509=DIRECTION('ref_axis',(-1.,0.,0.));
#31510=DIRECTION('',(0.,-1.,0.));
#31511=DIRECTION('center_axis',(0.,0.,1.));
#31512=DIRECTION('ref_axis',(-1.,0.,0.));
#31513=DIRECTION('',(0.707106781186544,-0.707106781186551,0.));
#31514=DIRECTION('center_axis',(0.,0.,-1.));
#31515=DIRECTION('ref_axis',(-1.,0.,0.));
#31516=DIRECTION('center_axis',(0.,0.,1.));
#31517=DIRECTION('ref_axis',(1.,0.,0.));
#31518=DIRECTION('center_axis',(0.,0.,-1.));
#31519=DIRECTION('ref_axis',(-1.,0.,0.));
#31520=DIRECTION('',(0.707106781186544,-0.707106781186551,0.));
#31521=DIRECTION('center_axis',(0.,0.,-1.));
#31522=DIRECTION('ref_axis',(-1.,0.,0.));
#31523=DIRECTION('',(0.,-1.,0.));
#31524=DIRECTION('center_axis',(0.,0.,-1.));
#31525=DIRECTION('ref_axis',(-1.,0.,0.));
#31526=DIRECTION('',(-0.70710678118655,-0.707106781186545,0.));
#31527=DIRECTION('center_axis',(0.,0.,-1.));
#31528=DIRECTION('ref_axis',(-1.,0.,0.));
#31529=DIRECTION('center_axis',(0.,0.,1.));
#31530=DIRECTION('ref_axis',(1.,0.,0.));
#31531=DIRECTION('center_axis',(0.,0.,-1.));
#31532=DIRECTION('ref_axis',(-1.,0.,0.));
#31533=DIRECTION('',(-0.70710678118655,-0.707106781186545,0.));
#31534=DIRECTION('',(-1.,0.,0.));
#31535=DIRECTION('',(0.70710678118655,-0.707106781186545,0.));
#31536=DIRECTION('center_axis',(0.,0.,-1.));
#31537=DIRECTION('ref_axis',(-1.,0.,0.));
#31538=DIRECTION('center_axis',(0.,0.,-1.));
#31539=DIRECTION('ref_axis',(-1.,0.,0.));
#31540=DIRECTION('center_axis',(0.,0.,-1.));
#31541=DIRECTION('ref_axis',(-1.,0.,0.));
#31542=DIRECTION('',(0.70710678118655,-0.707106781186545,0.));
#31543=DIRECTION('center_axis',(0.,0.,-1.));
#31544=DIRECTION('ref_axis',(-1.,0.,0.));
#31545=DIRECTION('',(0.,-1.,0.));
#31546=DIRECTION('center_axis',(0.,0.,-1.));
#31547=DIRECTION('ref_axis',(-1.,0.,0.));
#31548=DIRECTION('',(-0.707106781186544,-0.707106781186551,0.));
#31549=DIRECTION('center_axis',(0.,0.,-1.));
#31550=DIRECTION('ref_axis',(-1.,0.,0.));
#31551=DIRECTION('center_axis',(0.,0.,-1.));
#31552=DIRECTION('ref_axis',(-1.,0.,0.));
#31553=DIRECTION('center_axis',(0.,0.,-1.));
#31554=DIRECTION('ref_axis',(-1.,0.,0.));
#31555=DIRECTION('',(-0.707106781186544,-0.707106781186551,0.));
#31556=DIRECTION('center_axis',(0.,0.,1.));
#31557=DIRECTION('ref_axis',(-1.,-3.46944695195361E-15,0.));
#31558=DIRECTION('',(0.,-1.,0.));
#31559=DIRECTION('center_axis',(0.,0.,1.));
#31560=DIRECTION('ref_axis',(-1.,0.,0.));
#31561=DIRECTION('',(0.707106781186551,-0.707106781186544,0.));
#31562=DIRECTION('center_axis',(0.,0.,-1.));
#31563=DIRECTION('ref_axis',(-1.,0.,0.));
#31564=DIRECTION('',(0.,-1.,0.));
#31565=DIRECTION('',(-0.707106781186544,-0.707106781186551,0.));
#31566=DIRECTION('',(-0.707106781186544,0.707106781186551,0.));
#31567=DIRECTION('',(-1.,6.19544098563146E-17,0.));
#31568=DIRECTION('center_axis',(0.,0.,-1.));
#31569=DIRECTION('ref_axis',(-1.,0.,0.));
#31570=DIRECTION('',(-0.707106781186551,-0.707106781186544,0.));
#31571=DIRECTION('',(-0.707106781186544,-0.707106781186551,0.));
#31572=DIRECTION('',(0.,-1.,0.));
#31573=DIRECTION('center_axis',(0.,0.,1.));
#31574=DIRECTION('ref_axis',(-1.,1.73472347597681E-15,0.));
#31575=DIRECTION('',(0.707106781186551,-0.707106781186544,0.));
#31576=DIRECTION('center_axis',(0.,0.,-1.));
#31577=DIRECTION('ref_axis',(-1.,0.,0.));
#31578=DIRECTION('',(0.,-1.,0.));
#31579=DIRECTION('center_axis',(0.,0.,-1.));
#31580=DIRECTION('ref_axis',(-1.,0.,0.));
#31581=DIRECTION('',(-0.707106781186544,-0.707106781186551,0.));
#31582=DIRECTION('center_axis',(0.,0.,1.));
#31583=DIRECTION('ref_axis',(-1.,0.,0.));
#31584=DIRECTION('center_axis',(0.,0.,-1.));
#31585=DIRECTION('ref_axis',(-1.,0.,0.));
#31586=DIRECTION('center_axis',(0.,0.,1.));
#31587=DIRECTION('ref_axis',(-1.,-6.93889390390722E-15,0.));
#31588=DIRECTION('',(-0.707106781186544,-0.707106781186551,0.));
#31589=DIRECTION('center_axis',(0.,0.,1.));
#31590=DIRECTION('ref_axis',(-1.,0.,0.));
#31591=DIRECTION('',(0.,-1.,0.));
#31592=DIRECTION('center_axis',(0.,0.,1.));
#31593=DIRECTION('ref_axis',(-1.,0.,0.));
#31594=DIRECTION('',(0.70710678118655,-0.707106781186545,0.));
#31595=DIRECTION('center_axis',(0.,0.,1.));
#31596=DIRECTION('ref_axis',(-1.,0.,0.));
#31597=DIRECTION('center_axis',(0.,0.,-1.));
#31598=DIRECTION('ref_axis',(-1.,0.,0.));
#31599=DIRECTION('center_axis',(0.,0.,1.));
#31600=DIRECTION('ref_axis',(-1.,0.,0.));
#31601=DIRECTION('',(0.70710678118655,-0.707106781186545,0.));
#31602=DIRECTION('',(-1.,0.,0.));
#31603=DIRECTION('',(-0.70710678118655,-0.707106781186545,0.));
#31604=DIRECTION('center_axis',(0.,0.,1.));
#31605=DIRECTION('ref_axis',(-1.,0.,0.));
#31606=DIRECTION('center_axis',(0.,0.,1.));
#31607=DIRECTION('ref_axis',(1.,0.,0.));
#31608=DIRECTION('center_axis',(0.,0.,1.));
#31609=DIRECTION('ref_axis',(-1.,-6.93889390390722E-15,0.));
#31610=DIRECTION('',(-0.70710678118655,-0.707106781186545,0.));
#31611=DIRECTION('center_axis',(0.,0.,1.));
#31612=DIRECTION('ref_axis',(-1.,6.93889390390722E-15,0.));
#31613=DIRECTION('',(0.,-1.,0.));
#31614=DIRECTION('center_axis',(0.,0.,1.));
#31615=DIRECTION('ref_axis',(-1.,0.,0.));
#31616=DIRECTION('',(0.707106781186544,-0.707106781186551,0.));
#31617=DIRECTION('center_axis',(0.,0.,1.));
#31618=DIRECTION('ref_axis',(-1.,0.,0.));
#31619=DIRECTION('center_axis',(0.,0.,1.));
#31620=DIRECTION('ref_axis',(1.,0.,0.));
#31621=DIRECTION('center_axis',(0.,0.,1.));
#31622=DIRECTION('ref_axis',(-1.,0.,0.));
#31623=DIRECTION('',(0.707106781186544,-0.707106781186551,0.));
#31624=DIRECTION('center_axis',(0.,0.,-1.));
#31625=DIRECTION('ref_axis',(-1.,0.,0.));
#31626=DIRECTION('',(0.,-1.,0.));
#31627=DIRECTION('center_axis',(0.,0.,-1.));
#31628=DIRECTION('ref_axis',(-1.,0.,0.));
#31629=DIRECTION('',(-0.707106781186551,-0.707106781186544,0.));
#31630=DIRECTION('center_axis',(0.,0.,1.));
#31631=DIRECTION('ref_axis',(-1.,1.12757025938493E-14,0.));
#31632=DIRECTION('',(0.,-1.,0.));
#31633=DIRECTION('',(0.707106781186544,-0.707106781186551,0.));
#31634=DIRECTION('center_axis',(-0.707106781186551,0.707106781186544,0.));
#31635=DIRECTION('ref_axis',(-0.707106781186544,-0.707106781186551,0.));
#31636=DIRECTION('',(0.,0.,-1.));
#31637=DIRECTION('',(0.,0.,1.));
#31638=DIRECTION('center_axis',(-0.707106781186551,0.707106781186544,0.));
#31639=DIRECTION('ref_axis',(-0.707106781186544,-0.707106781186551,0.));
#31640=DIRECTION('',(0.,0.,1.));
#31641=DIRECTION('',(0.,0.,-1.));
#31642=DIRECTION('center_axis',(-0.707106781186545,-0.70710678118655,0.));
#31643=DIRECTION('ref_axis',(0.70710678118655,-0.707106781186545,0.));
#31644=DIRECTION('',(0.,0.,1.));
#31645=DIRECTION('',(0.,0.,-1.));
#31646=DIRECTION('center_axis',(-0.707106781186545,-0.70710678118655,0.));
#31647=DIRECTION('ref_axis',(0.70710678118655,-0.707106781186545,0.));
#31648=DIRECTION('',(0.,0.,-1.));
#31649=DIRECTION('',(0.,0.,1.));
#31650=DIRECTION('center_axis',(-0.707106781186551,-0.707106781186544,0.));
#31651=DIRECTION('ref_axis',(0.707106781186544,-0.707106781186551,0.));
#31652=DIRECTION('',(0.,0.,1.));
#31653=DIRECTION('',(0.,0.,-1.));
#31654=DIRECTION('center_axis',(-0.707106781186545,0.70710678118655,0.));
#31655=DIRECTION('ref_axis',(-0.70710678118655,-0.707106781186545,0.));
#31656=DIRECTION('',(0.,0.,-1.));
#31657=DIRECTION('',(0.,0.,1.));
#31658=DIRECTION('center_axis',(0.,1.,0.));
#31659=DIRECTION('ref_axis',(0.,0.,1.));
#31660=DIRECTION('',(0.,0.,1.));
#31661=DIRECTION('center_axis',(-0.707106781186551,-0.707106781186544,0.));
#31662=DIRECTION('ref_axis',(0.707106781186544,-0.707106781186551,0.));
#31663=DIRECTION('',(0.,0.,1.));
#31664=DIRECTION('center_axis',(-1.,0.,0.));
#31665=DIRECTION('ref_axis',(0.,0.,1.));
#31666=DIRECTION('',(0.,0.,-1.));
#31667=DIRECTION('center_axis',(-0.707106781186544,0.707106781186551,0.));
#31668=DIRECTION('ref_axis',(-0.707106781186551,-0.707106781186544,0.));
#31669=DIRECTION('',(0.,0.,1.));
#31670=DIRECTION('',(0.,0.,-1.));
#31671=DIRECTION('center_axis',(-1.,0.,0.));
#31672=DIRECTION('ref_axis',(0.,0.,1.));
#31673=DIRECTION('',(0.,0.,1.));
#31674=DIRECTION('',(0.,0.,-1.));
#31675=DIRECTION('center_axis',(-0.707106781186551,-0.707106781186544,0.));
#31676=DIRECTION('ref_axis',(0.707106781186544,-0.707106781186551,0.));
#31677=DIRECTION('',(0.,0.,-1.));
#31678=DIRECTION('',(0.,0.,1.));
#31679=DIRECTION('center_axis',(-1.,0.,0.));
#31680=DIRECTION('ref_axis',(0.,0.,1.));
#31681=DIRECTION('',(0.,0.,-1.));
#31682=DIRECTION('',(0.,0.,1.));
#31683=DIRECTION('center_axis',(-0.707106781186545,0.70710678118655,0.));
#31684=DIRECTION('ref_axis',(-0.70710678118655,-0.707106781186545,0.));
#31685=DIRECTION('',(0.,0.,1.));
#31686=DIRECTION('center_axis',(0.,0.,1.));
#31687=DIRECTION('ref_axis',(1.,0.,0.));
#31688=DIRECTION('',(0.,0.,1.));
#31689=DIRECTION('',(0.,0.,-1.));
#31690=DIRECTION('center_axis',(0.,0.,1.));
#31691=DIRECTION('ref_axis',(1.,0.,0.));
#31692=DIRECTION('',(0.,0.,-1.));
#31693=DIRECTION('',(0.,0.,1.));
#31694=DIRECTION('center_axis',(0.,0.,1.));
#31695=DIRECTION('ref_axis',(1.,0.,0.));
#31696=DIRECTION('center_axis',(0.,0.,1.));
#31697=DIRECTION('ref_axis',(1.,0.,0.));
#31698=DIRECTION('center_axis',(0.,0.,1.));
#31699=DIRECTION('ref_axis',(1.,0.,0.));
#31700=DIRECTION('center_axis',(0.,0.,1.));
#31701=DIRECTION('ref_axis',(1.,0.,0.));
#31702=DIRECTION('center_axis',(0.,0.,-1.));
#31703=DIRECTION('ref_axis',(-1.,0.,0.));
#31704=DIRECTION('center_axis',(0.,0.,-1.));
#31705=DIRECTION('ref_axis',(-1.,0.,0.));
#31706=DIRECTION('center_axis',(0.,0.,1.));
#31707=DIRECTION('ref_axis',(1.,0.,0.));
#31708=DIRECTION('center_axis',(0.,0.,1.));
#31709=DIRECTION('ref_axis',(1.,0.,0.));
#31710=DIRECTION('center_axis',(0.,0.,1.));
#31711=DIRECTION('ref_axis',(1.,0.,0.));
#31712=DIRECTION('center_axis',(-1.,0.,0.));
#31713=DIRECTION('ref_axis',(0.,0.,1.));
#31714=DIRECTION('',(0.,0.,1.));
#31715=DIRECTION('',(0.,0.,-1.));
#31716=DIRECTION('center_axis',(-1.,0.,0.));
#31717=DIRECTION('ref_axis',(0.,0.,1.));
#31718=DIRECTION('',(0.,0.,-1.));
#31719=DIRECTION('',(0.,0.,1.));
#31720=DIRECTION('center_axis',(-0.707106781186544,-0.707106781186551,0.));
#31721=DIRECTION('ref_axis',(0.707106781186551,-0.707106781186544,0.));
#31722=DIRECTION('',(0.,0.,-1.));
#31723=DIRECTION('',(0.,0.,1.));
#31724=DIRECTION('center_axis',(-1.,0.,0.));
#31725=DIRECTION('ref_axis',(0.,0.,1.));
#31726=DIRECTION('',(0.,0.,1.));
#31727=DIRECTION('',(0.,0.,1.));
#31728=DIRECTION('center_axis',(-0.707106781186551,0.707106781186544,0.));
#31729=DIRECTION('ref_axis',(-0.707106781186544,-0.707106781186551,0.));
#31730=DIRECTION('center_axis',(0.,0.,1.));
#31731=DIRECTION('ref_axis',(1.,0.,0.));
#31732=DIRECTION('',(0.,0.,-1.));
#31733=DIRECTION('',(0.,0.,1.));
#31734=DIRECTION('center_axis',(0.,0.,1.));
#31735=DIRECTION('ref_axis',(1.,0.,0.));
#31736=DIRECTION('',(0.,0.,1.));
#31737=DIRECTION('',(0.,0.,-1.));
#31738=DIRECTION('center_axis',(0.,0.,1.));
#31739=DIRECTION('ref_axis',(1.,0.,0.));
#31740=DIRECTION('center_axis',(0.,0.,1.));
#31741=DIRECTION('ref_axis',(1.,0.,0.));
#31742=DIRECTION('center_axis',(0.,0.,1.));
#31743=DIRECTION('ref_axis',(1.,0.,0.));
#31744=DIRECTION('center_axis',(0.,0.,1.));
#31745=DIRECTION('ref_axis',(1.,0.,0.));
#31746=DIRECTION('center_axis',(0.,0.,-1.));
#31747=DIRECTION('ref_axis',(-1.,0.,0.));
#31748=DIRECTION('center_axis',(0.,0.,-1.));
#31749=DIRECTION('ref_axis',(-1.,0.,0.));
#31750=DIRECTION('center_axis',(0.,0.,1.));
#31751=DIRECTION('ref_axis',(1.,0.,0.));
#31752=DIRECTION('center_axis',(0.,0.,1.));
#31753=DIRECTION('ref_axis',(1.,0.,0.));
#31754=DIRECTION('center_axis',(0.,0.,1.));
#31755=DIRECTION('ref_axis',(1.,0.,0.));
#31756=DIRECTION('center_axis',(-0.707106781186544,0.707106781186551,0.));
#31757=DIRECTION('ref_axis',(-0.707106781186551,-0.707106781186544,0.));
#31758=DIRECTION('center_axis',(6.19544098563146E-17,1.,0.));
#31759=DIRECTION('ref_axis',(-1.,6.19544098563146E-17,0.));
#31760=DIRECTION('',(0.,0.,1.));
#31761=DIRECTION('center_axis',(0.707106781186551,0.707106781186544,0.));
#31762=DIRECTION('ref_axis',(-0.707106781186544,0.707106781186551,0.));
#31763=DIRECTION('center_axis',(0.,-1.,0.));
#31764=DIRECTION('ref_axis',(0.,0.,-1.));
#31765=DIRECTION('center_axis',(0.,-1.,0.));
#31766=DIRECTION('ref_axis',(0.,0.,-1.));
#31767=DIRECTION('center_axis',(0.,-1.,0.));
#31768=DIRECTION('ref_axis',(0.,0.,-1.));
#31769=DIRECTION('center_axis',(0.,-1.,0.));
#31770=DIRECTION('ref_axis',(0.,0.,-1.));
#31771=DIRECTION('center_axis',(0.,-1.,0.));
#31772=DIRECTION('ref_axis',(0.,0.,-1.));
#31773=DIRECTION('center_axis',(0.,-1.,0.));
#31774=DIRECTION('ref_axis',(0.,0.,-1.));
#31775=DIRECTION('center_axis',(0.,-1.,0.));
#31776=DIRECTION('ref_axis',(0.,0.,-1.));
#31777=DIRECTION('center_axis',(0.,-1.,0.));
#31778=DIRECTION('ref_axis',(0.,0.,-1.));
#31779=DIRECTION('axis',(0.,0.,1.));
#31780=DIRECTION('refdir',(1.,0.,0.));
#31781=DIRECTION('center_axis',(1.,0.,0.));
#31782=DIRECTION('ref_axis',(0.,0.,-1.));
#31783=DIRECTION('center_axis',(1.,0.,0.));
#31784=DIRECTION('ref_axis',(0.,0.,-1.));
#31785=DIRECTION('',(1.,0.,0.));
#31786=DIRECTION('center_axis',(1.,0.,0.));
#31787=DIRECTION('ref_axis',(0.,0.,-1.));
#31788=DIRECTION('center_axis',(-1.,0.,0.));
#31789=DIRECTION('ref_axis',(0.,0.,1.));
#31790=DIRECTION('center_axis',(-1.,0.,0.));
#31791=DIRECTION('ref_axis',(0.,0.,1.));
#31792=DIRECTION('',(-1.,0.,0.));
#31793=DIRECTION('center_axis',(-1.,0.,0.));
#31794=DIRECTION('ref_axis',(0.,0.,1.));
#31795=DIRECTION('center_axis',(-1.30104260698261E-15,1.,-1.73611473352215E-31));
#31796=DIRECTION('ref_axis',(-1.,-1.30104260698261E-15,-2.16593351677506E-47));
#31797=DIRECTION('center_axis',(-1.30104260698261E-15,1.,-1.73611473352215E-31));
#31798=DIRECTION('ref_axis',(-1.,-1.30104260698261E-15,-2.16593351677507E-47));
#31799=DIRECTION('',(-1.30104260698261E-15,1.,-1.73611473352215E-31));
#31800=DIRECTION('center_axis',(-1.30104260698261E-15,1.,-1.73611473352215E-31));
#31801=DIRECTION('ref_axis',(-1.,-1.30104260698261E-15,-2.16593351677507E-47));
#31802=DIRECTION('center_axis',(1.,0.,0.));
#31803=DIRECTION('ref_axis',(0.,0.,-1.));
#31804=DIRECTION('',(0.515038074910055,-1.04972719113862E-16,0.857167300702112));
#31805=DIRECTION('center_axis',(-1.,0.,0.));
#31806=DIRECTION('ref_axis',(0.,0.,1.));
#31807=DIRECTION('',(-0.515038074910054,-1.04972719113862E-16,-0.857167300702112));
#31808=DIRECTION('center_axis',(0.,1.,0.));
#31809=DIRECTION('ref_axis',(0.,0.,1.));
#31810=DIRECTION('center_axis',(-1.2823896663807E-16,1.,0.));
#31811=DIRECTION('ref_axis',(-1.,-1.2823896663807E-16,0.));
#31812=DIRECTION('',(0.,1.,0.));
#31813=DIRECTION('center_axis',(0.,1.,0.));
#31814=DIRECTION('ref_axis',(0.,0.,1.));
#31815=DIRECTION('center_axis',(0.,1.,0.));
#31816=DIRECTION('ref_axis',(0.,0.,1.));
#31817=DIRECTION('center_axis',(-1.2823896663807E-16,1.,0.));
#31818=DIRECTION('ref_axis',(-1.,-1.2823896663807E-16,0.));
#31819=DIRECTION('',(0.,1.,0.));
#31820=DIRECTION('center_axis',(0.,1.,0.));
#31821=DIRECTION('ref_axis',(0.,0.,1.));
#31822=DIRECTION('center_axis',(0.,1.,0.));
#31823=DIRECTION('ref_axis',(0.,0.,1.));
#31824=DIRECTION('center_axis',(1.2823896663807E-16,1.,0.));
#31825=DIRECTION('ref_axis',(-1.,1.2823896663807E-16,0.));
#31826=DIRECTION('',(0.,1.,0.));
#31827=DIRECTION('center_axis',(0.,1.,0.));
#31828=DIRECTION('ref_axis',(0.,0.,1.));
#31829=DIRECTION('center_axis',(0.,1.,0.));
#31830=DIRECTION('ref_axis',(0.,0.,1.));
#31831=DIRECTION('center_axis',(1.2823896663807E-16,1.,0.));
#31832=DIRECTION('ref_axis',(-1.,1.2823896663807E-16,0.));
#31833=DIRECTION('',(0.,1.,0.));
#31834=DIRECTION('center_axis',(0.,1.,0.));
#31835=DIRECTION('ref_axis',(0.,0.,1.));
#31836=DIRECTION('center_axis',(-1.,0.,0.));
#31837=DIRECTION('ref_axis',(0.,0.,1.));
#31838=DIRECTION('center_axis',(-1.,0.,0.));
#31839=DIRECTION('ref_axis',(0.,0.,1.));
#31840=DIRECTION('',(-1.,0.,0.));
#31841=DIRECTION('center_axis',(-1.,0.,0.));
#31842=DIRECTION('ref_axis',(0.,0.,1.));
#31843=DIRECTION('center_axis',(1.,0.,0.));
#31844=DIRECTION('ref_axis',(0.,0.,-1.));
#31845=DIRECTION('center_axis',(1.,0.,0.));
#31846=DIRECTION('ref_axis',(0.,0.,-1.));
#31847=DIRECTION('',(1.,0.,0.));
#31848=DIRECTION('center_axis',(1.,0.,0.));
#31849=DIRECTION('ref_axis',(0.,0.,-1.));
#31850=DIRECTION('center_axis',(-1.30104260698261E-15,1.,-1.73611473352215E-31));
#31851=DIRECTION('ref_axis',(-1.,-1.30104260698261E-15,-2.16593351677506E-47));
#31852=DIRECTION('center_axis',(-1.30104260698261E-15,1.,-1.73611473352215E-31));
#31853=DIRECTION('ref_axis',(-1.,-1.30104260698261E-15,-2.16593351677507E-47));
#31854=DIRECTION('',(-1.30104260698261E-15,1.,-1.73611473352215E-31));
#31855=DIRECTION('center_axis',(-1.30104260698261E-15,1.,-1.73611473352215E-31));
#31856=DIRECTION('ref_axis',(-1.,-1.30104260698261E-15,-2.16593351677507E-47));
#31857=DIRECTION('center_axis',(-1.30104260698261E-15,1.,-1.73611473352215E-31));
#31858=DIRECTION('ref_axis',(-1.,-1.30104260698261E-15,2.25875923892257E-46));
#31859=DIRECTION('center_axis',(-1.30104260698261E-15,1.,-1.73611473352215E-31));
#31860=DIRECTION('ref_axis',(-1.,-1.30104260698261E-15,2.25875923892257E-46));
#31861=DIRECTION('',(-1.30104260698261E-15,1.,-1.73611473352215E-31));
#31862=DIRECTION('center_axis',(-1.30104260698261E-15,1.,-1.73611473352215E-31));
#31863=DIRECTION('ref_axis',(-1.,-1.30104260698261E-15,2.25875923892257E-46));
#31864=DIRECTION('',(-1.30104260698261E-15,1.,-1.73611473352215E-31));
#31865=DIRECTION('center_axis',(-1.30104260698261E-15,1.,-1.73611473352215E-31));
#31866=DIRECTION('ref_axis',(-1.,-1.30104260698261E-15,2.25875923892257E-46));
#31867=DIRECTION('',(-1.30104260698261E-15,1.,-1.73611473352215E-31));
#31868=DIRECTION('center_axis',(-1.,0.,0.));
#31869=DIRECTION('ref_axis',(0.,0.,1.));
#31870=DIRECTION('',(-0.515038074910054,-1.04972719113862E-16,-0.857167300702112));
#31871=DIRECTION('center_axis',(1.,0.,0.));
#31872=DIRECTION('ref_axis',(0.,0.,-1.));
#31873=DIRECTION('',(0.515038074910055,-1.04972719113862E-16,0.857167300702112));
#31874=DIRECTION('center_axis',(-1.30104260698261E-15,1.,-1.73611473352215E-31));
#31875=DIRECTION('ref_axis',(-1.,-1.30104260698261E-15,2.25875923892257E-46));
#31876=DIRECTION('center_axis',(-1.30104260698261E-15,1.,-1.73611473352215E-31));
#31877=DIRECTION('ref_axis',(-1.,-1.30104260698261E-15,2.25875923892257E-46));
#31878=DIRECTION('',(-1.30104260698261E-15,1.,-1.73611473352215E-31));
#31879=DIRECTION('',(-1.30104260698261E-15,1.,-1.73611473352215E-31));
#31880=DIRECTION('center_axis',(-1.30104260698261E-15,1.,-1.73611473352215E-31));
#31881=DIRECTION('ref_axis',(-1.,-1.30104260698261E-15,2.25875923892257E-46));
#31882=DIRECTION('',(-1.30104260698261E-15,1.,-1.73611473352215E-31));
#31883=DIRECTION('center_axis',(-1.30104260698261E-15,1.,-1.73611473352215E-31));
#31884=DIRECTION('ref_axis',(-1.,-1.30104260698261E-15,2.25875923892257E-46));
#31885=DIRECTION('center_axis',(0.,0.,1.));
#31886=DIRECTION('ref_axis',(-1.,0.,0.));
#31887=DIRECTION('center_axis',(0.,0.,1.));
#31888=DIRECTION('ref_axis',(-1.,0.,0.));
#31889=DIRECTION('center_axis',(0.,0.,1.));
#31890=DIRECTION('ref_axis',(1.,0.,0.));
#31891=DIRECTION('center_axis',(0.,0.,-1.));
#31892=DIRECTION('ref_axis',(-1.,0.,0.));
#31893=DIRECTION('',(0.,0.,-1.));
#31894=DIRECTION('center_axis',(0.,0.,-1.));
#31895=DIRECTION('ref_axis',(-1.,0.,0.));
#31896=DIRECTION('center_axis',(0.,0.,-1.));
#31897=DIRECTION('ref_axis',(-1.,0.,0.));
#31898=DIRECTION('',(0.,0.,-1.));
#31899=DIRECTION('center_axis',(0.,0.,-1.));
#31900=DIRECTION('ref_axis',(-1.,0.,0.));
#31901=DIRECTION('center_axis',(0.61566147532566,-0.788010753606721,0.));
#31902=DIRECTION('ref_axis',(0.78801075360672,0.61566147532566,0.));
#31903=DIRECTION('center_axis',(0.615661475325656,-0.788010753606724,-5.22755357805913E-15));
#31904=DIRECTION('ref_axis',(0.788010753606724,0.615661475325656,-5.17730530723809E-13));
#31905=DIRECTION('',(0.,0.,1.));
#31906=DIRECTION('',(0.78801075360672,0.61566147532566,0.));
#31907=DIRECTION('',(0.,0.,1.));
#31908=DIRECTION('center_axis',(0.61566147532566,-0.788010753606721,0.));
#31909=DIRECTION('ref_axis',(0.78801075360672,0.61566147532566,0.));
#31910=DIRECTION('center_axis',(0.615661475325656,-0.788010753606724,5.27148259972344E-15));
#31911=DIRECTION('ref_axis',(0.788010753606724,0.615661475325656,-9.16833363821094E-14));
#31912=DIRECTION('',(0.,0.,1.));
#31913=DIRECTION('center_axis',(0.615661475325662,-0.788010753606719,1.40572869325959E-15));
#31914=DIRECTION('ref_axis',(0.788010753606719,0.615661475325662,-7.1472163446861E-13));
#31915=DIRECTION('',(0.,0.,1.));
#31916=DIRECTION('center_axis',(-0.61566147532566,-0.788010753606721,0.));
#31917=DIRECTION('ref_axis',(0.78801075360672,-0.61566147532566,0.));
#31918=DIRECTION('center_axis',(-0.615661475325663,-0.788010753606718,-3.73396684147081E-15));
#31919=DIRECTION('ref_axis',(0.788010753606718,-0.615661475325663,1.05496270744081E-13));
#31920=DIRECTION('',(0.,0.,1.));
#31921=DIRECTION('center_axis',(-0.615661475325666,-0.788010753606716,6.32577911966821E-15));
#31922=DIRECTION('ref_axis',(0.788010753606716,-0.615661475325666,2.12834187078208E-13));
#31923=DIRECTION('',(0.,0.,1.));
#31924=DIRECTION('center_axis',(-0.61566147532566,-0.788010753606721,0.));
#31925=DIRECTION('ref_axis',(0.78801075360672,-0.61566147532566,0.));
#31926=DIRECTION('center_axis',(-0.615661475325663,-0.788010753606718,-3.64610879814206E-15));
#31927=DIRECTION('ref_axis',(0.788010753606718,-0.615661475325663,-2.42930938978673E-14));
#31928=DIRECTION('',(0.,0.,1.));
#31929=DIRECTION('',(0.78801075360672,-0.61566147532566,0.));
#31930=DIRECTION('',(0.,0.,1.));
#31931=DIRECTION('center_axis',(-0.707106781186546,0.707106781186549,0.));
#31932=DIRECTION('ref_axis',(-0.707106781186549,-0.707106781186546,0.));
#31933=DIRECTION('',(-0.707106781186549,-0.707106781186546,0.));
#31934=DIRECTION('',(0.,0.,-1.));
#31935=DIRECTION('',(-0.707106781186549,-0.707106781186546,0.));
#31936=DIRECTION('',(0.,0.,1.));
#31937=DIRECTION('center_axis',(-0.707106781186549,-0.707106781186546,0.));
#31938=DIRECTION('ref_axis',(0.707106781186546,-0.707106781186549,0.));
#31939=DIRECTION('',(0.707106781186545,-0.70710678118655,0.));
#31940=DIRECTION('',(0.,0.,-1.));
#31941=DIRECTION('',(0.707106781186546,-0.707106781186549,0.));
#31942=DIRECTION('',(0.,0.,1.));
#31943=DIRECTION('center_axis',(0.707106781186546,0.707106781186549,0.));
#31944=DIRECTION('ref_axis',(-0.707106781186549,0.707106781186546,0.));
#31945=DIRECTION('',(-0.707106781186548,0.707106781186547,0.));
#31946=DIRECTION('',(0.,0.,-1.));
#31947=DIRECTION('',(-0.707106781186549,0.707106781186546,0.));
#31948=DIRECTION('',(0.,0.,1.));
#31949=DIRECTION('center_axis',(0.707106781186549,-0.707106781186546,0.));
#31950=DIRECTION('ref_axis',(0.707106781186546,0.707106781186549,0.));
#31951=DIRECTION('',(0.707106781186546,0.707106781186549,0.));
#31952=DIRECTION('',(0.,0.,-1.));
#31953=DIRECTION('',(0.707106781186546,0.707106781186549,0.));
#31954=DIRECTION('',(0.,0.,1.));
#31955=DIRECTION('center_axis',(0.707106781186549,-0.707106781186546,0.));
#31956=DIRECTION('ref_axis',(0.707106781186546,0.707106781186549,0.));
#31957=DIRECTION('',(0.707106781186545,0.70710678118655,0.));
#31958=DIRECTION('',(0.,0.,-1.));
#31959=DIRECTION('',(0.707106781186546,0.707106781186549,0.));
#31960=DIRECTION('',(0.,0.,1.));
#31961=DIRECTION('center_axis',(1.,0.,0.));
#31962=DIRECTION('ref_axis',(0.,0.,-1.));
#31963=DIRECTION('',(0.,1.,0.));
#31964=DIRECTION('',(0.,0.,-1.));
#31965=DIRECTION('',(0.,1.,0.));
#31966=DIRECTION('',(0.,0.,1.));
#31967=DIRECTION('center_axis',(0.707106781186546,0.707106781186549,0.));
#31968=DIRECTION('ref_axis',(-0.707106781186549,0.707106781186546,0.));
#31969=DIRECTION('',(-0.707106781186549,0.707106781186546,0.));
#31970=DIRECTION('',(0.,0.,-1.));
#31971=DIRECTION('',(-0.707106781186549,0.707106781186546,0.));
#31972=DIRECTION('',(0.,0.,1.));
#31973=DIRECTION('center_axis',(1.,0.,0.));
#31974=DIRECTION('ref_axis',(0.,0.,-1.));
#31975=DIRECTION('',(0.,1.,0.));
#31976=DIRECTION('',(0.,0.,-1.));
#31977=DIRECTION('',(0.,1.,0.));
#31978=DIRECTION('',(0.,0.,1.));
#31979=DIRECTION('center_axis',(0.707106781186549,-0.707106781186546,0.));
#31980=DIRECTION('ref_axis',(0.707106781186546,0.707106781186549,0.));
#31981=DIRECTION('',(0.707106781186546,0.707106781186549,0.));
#31982=DIRECTION('',(0.,0.,1.));
#31983=DIRECTION('',(0.707106781186546,0.707106781186549,0.));
#31984=DIRECTION('',(0.,0.,1.));
#31985=DIRECTION('center_axis',(0.,-1.,0.));
#31986=DIRECTION('ref_axis',(0.,0.,-1.));
#31987=DIRECTION('',(1.,0.,0.));
#31988=DIRECTION('',(0.,0.,1.));
#31989=DIRECTION('',(1.,0.,0.));
#31990=DIRECTION('center_axis',(-6.49101394191508E-16,-1.,0.));
#31991=DIRECTION('ref_axis',(1.,-6.49101394191508E-16,0.));
#31992=DIRECTION('',(1.,-3.50803534070133E-16,0.));
#31993=DIRECTION('',(0.,0.,1.));
#31994=DIRECTION('',(1.,-6.49101394191508E-16,0.));
#31995=DIRECTION('',(0.,0.,1.));
#31996=DIRECTION('center_axis',(-0.707106781186549,-0.707106781186546,0.));
#31997=DIRECTION('ref_axis',(0.707106781186546,-0.707106781186549,0.));
#31998=DIRECTION('',(0.707106781186546,-0.707106781186549,0.));
#31999=DIRECTION('',(0.,0.,-1.));
#32000=DIRECTION('',(0.707106781186546,-0.707106781186549,0.));
#32001=DIRECTION('center_axis',(-1.,0.,0.));
#32002=DIRECTION('ref_axis',(0.,0.,1.));
#32003=DIRECTION('',(0.,-1.,0.));
#32004=DIRECTION('',(0.,0.,-1.));
#32005=DIRECTION('',(0.,-1.,0.));
#32006=DIRECTION('',(0.,0.,1.));
#32007=DIRECTION('center_axis',(-0.707106781186546,0.707106781186549,0.));
#32008=DIRECTION('ref_axis',(-0.707106781186549,-0.707106781186546,0.));
#32009=DIRECTION('',(-0.707106781186548,-0.707106781186547,0.));
#32010=DIRECTION('',(0.,0.,-1.));
#32011=DIRECTION('',(-0.707106781186549,-0.707106781186546,0.));
#32012=DIRECTION('',(0.,0.,1.));
#32013=DIRECTION('center_axis',(-1.,0.,0.));
#32014=DIRECTION('ref_axis',(0.,0.,1.));
#32015=DIRECTION('',(0.,-1.,0.));
#32016=DIRECTION('',(0.,0.,-1.));
#32017=DIRECTION('',(0.,-1.,0.));
#32018=DIRECTION('',(0.,0.,1.));
#32019=DIRECTION('center_axis',(-0.707106781186549,-0.707106781186546,0.));
#32020=DIRECTION('ref_axis',(0.707106781186546,-0.707106781186549,0.));
#32021=DIRECTION('',(0.707106781186546,-0.707106781186549,0.));
#32022=DIRECTION('',(0.,0.,1.));
#32023=DIRECTION('',(0.707106781186546,-0.707106781186549,0.));
#32024=DIRECTION('',(0.,0.,1.));
#32025=DIRECTION('center_axis',(1.22464679914735E-16,-1.,0.));
#32026=DIRECTION('ref_axis',(1.,1.22464679914735E-16,0.));
#32027=DIRECTION('',(1.,1.22464679914735E-16,0.));
#32028=DIRECTION('',(1.,1.22464679914735E-16,0.));
#32029=DIRECTION('center_axis',(0.,0.,1.));
#32030=DIRECTION('ref_axis',(1.,0.,0.));
#32031=DIRECTION('center_axis',(0.,0.,1.));
#32032=DIRECTION('ref_axis',(1.,0.,0.));
#32033=DIRECTION('',(0.,0.,-1.));
#32034=DIRECTION('center_axis',(0.,0.,1.));
#32035=DIRECTION('ref_axis',(1.,0.,0.));
#32036=DIRECTION('',(0.,0.,1.));
#32037=DIRECTION('center_axis',(0.,0.,1.));
#32038=DIRECTION('ref_axis',(1.,0.,0.));
#32039=DIRECTION('center_axis',(0.,0.,1.));
#32040=DIRECTION('ref_axis',(1.,0.,0.));
#32041=DIRECTION('',(0.,0.,-1.));
#32042=DIRECTION('center_axis',(0.,0.,1.));
#32043=DIRECTION('ref_axis',(1.,0.,0.));
#32044=DIRECTION('',(0.,0.,1.));
#32045=DIRECTION('center_axis',(0.,0.,1.));
#32046=DIRECTION('ref_axis',(1.,0.,0.));
#32047=DIRECTION('center_axis',(0.,0.,1.));
#32048=DIRECTION('ref_axis',(1.,0.,0.));
#32049=DIRECTION('',(0.,0.,-1.));
#32050=DIRECTION('center_axis',(0.,0.,1.));
#32051=DIRECTION('ref_axis',(1.,0.,0.));
#32052=DIRECTION('',(0.,0.,1.));
#32053=DIRECTION('center_axis',(0.,0.,1.));
#32054=DIRECTION('ref_axis',(1.,0.,0.));
#32055=DIRECTION('center_axis',(0.,0.,1.));
#32056=DIRECTION('ref_axis',(1.,0.,0.));
#32057=DIRECTION('',(0.,0.,-1.));
#32058=DIRECTION('center_axis',(0.,0.,1.));
#32059=DIRECTION('ref_axis',(1.,0.,0.));
#32060=DIRECTION('',(0.,0.,1.));
#32061=DIRECTION('center_axis',(0.,0.,1.));
#32062=DIRECTION('ref_axis',(1.,0.,0.));
#32063=DIRECTION('center_axis',(0.,0.,1.));
#32064=DIRECTION('ref_axis',(1.,0.,0.));
#32065=DIRECTION('center_axis',(0.,0.,-1.));
#32066=DIRECTION('ref_axis',(-1.,0.,0.));
#32067=DIRECTION('center_axis',(0.,0.,1.));
#32068=DIRECTION('ref_axis',(1.,0.,0.));
#32069=DIRECTION('center_axis',(0.,0.,1.));
#32070=DIRECTION('ref_axis',(1.,0.,0.));
#32071=DIRECTION('center_axis',(0.,0.,-1.));
#32072=DIRECTION('ref_axis',(-1.,0.,0.));
#32073=DIRECTION('center_axis',(0.,0.,-1.));
#32074=DIRECTION('ref_axis',(-1.,0.,0.));
#32075=DIRECTION('center_axis',(0.,0.,-1.));
#32076=DIRECTION('ref_axis',(1.,0.,0.));
#32077=DIRECTION('center_axis',(0.,0.,1.));
#32078=DIRECTION('ref_axis',(-1.,0.,0.));
#32079=DIRECTION('center_axis',(0.,0.,-1.));
#32080=DIRECTION('ref_axis',(-1.,0.,0.));
#32081=DIRECTION('center_axis',(0.,0.,-1.));
#32082=DIRECTION('ref_axis',(1.,0.,0.));
#32083=DIRECTION('center_axis',(0.,0.,1.));
#32084=DIRECTION('ref_axis',(-1.,-5.20417042793042E-15,0.));
#32085=DIRECTION('center_axis',(0.,0.,1.));
#32086=DIRECTION('ref_axis',(1.,0.,0.));
#32087=DIRECTION('center_axis',(0.,0.,-1.));
#32088=DIRECTION('ref_axis',(1.,0.,0.));
#32089=DIRECTION('center_axis',(0.,0.,1.));
#32090=DIRECTION('ref_axis',(-1.,-3.46944695195361E-15,0.));
#32091=DIRECTION('center_axis',(0.,0.,1.));
#32092=DIRECTION('ref_axis',(1.,0.,0.));
#32093=DIRECTION('center_axis',(0.,0.,-1.));
#32094=DIRECTION('ref_axis',(1.,0.,0.));
#32095=DIRECTION('center_axis',(0.,0.,1.));
#32096=DIRECTION('ref_axis',(-1.,5.42101086242752E-15,0.));
#32097=DIRECTION('center_axis',(0.,0.,1.));
#32098=DIRECTION('ref_axis',(1.,0.,0.));
#32099=DIRECTION('center_axis',(0.,0.,-1.));
#32100=DIRECTION('ref_axis',(1.,0.,0.));
#32101=DIRECTION('center_axis',(0.,0.,1.));
#32102=DIRECTION('ref_axis',(-1.,-1.73472347597681E-15,0.));
#32103=DIRECTION('center_axis',(0.,0.,1.));
#32104=DIRECTION('ref_axis',(1.,0.,0.));
#32105=DIRECTION('center_axis',(0.,0.,-1.));
#32106=DIRECTION('ref_axis',(1.,0.,0.));
#32107=DIRECTION('center_axis',(0.,0.,1.));
#32108=DIRECTION('ref_axis',(-1.,8.67361737988403E-15,0.));
#32109=DIRECTION('center_axis',(0.,0.,1.));
#32110=DIRECTION('ref_axis',(1.,0.,0.));
#32111=DIRECTION('center_axis',(0.,0.,1.));
#32112=DIRECTION('ref_axis',(1.,0.,0.));
#32113=DIRECTION('center_axis',(0.,0.,-1.));
#32114=DIRECTION('ref_axis',(-1.,0.,0.));
#32115=DIRECTION('center_axis',(0.,0.,1.));
#32116=DIRECTION('ref_axis',(1.,0.,0.));
#32117=DIRECTION('center_axis',(0.,0.,1.));
#32118=DIRECTION('ref_axis',(1.,0.,0.));
#32119=DIRECTION('center_axis',(0.,0.,-1.));
#32120=DIRECTION('ref_axis',(-1.,0.,0.));
#32121=DIRECTION('center_axis',(0.,0.,1.));
#32122=DIRECTION('ref_axis',(1.,0.,0.));
#32123=DIRECTION('center_axis',(0.,0.,-1.));
#32124=DIRECTION('ref_axis',(1.,0.,0.));
#32125=DIRECTION('center_axis',(0.,0.,1.));
#32126=DIRECTION('ref_axis',(-1.,1.73472347597681E-15,0.));
#32127=DIRECTION('center_axis',(0.,0.,1.));
#32128=DIRECTION('ref_axis',(1.,0.,0.));
#32129=DIRECTION('center_axis',(0.,0.,-1.));
#32130=DIRECTION('ref_axis',(1.,0.,0.));
#32131=DIRECTION('center_axis',(0.,0.,1.));
#32132=DIRECTION('ref_axis',(-1.,0.,0.));
#32133=DIRECTION('center_axis',(0.,0.,-1.));
#32134=DIRECTION('ref_axis',(-1.,0.,0.));
#32135=DIRECTION('center_axis',(0.,0.,-1.));
#32136=DIRECTION('ref_axis',(1.,0.,0.));
#32137=DIRECTION('center_axis',(0.,0.,1.));
#32138=DIRECTION('ref_axis',(-1.,0.,0.));
#32139=DIRECTION('center_axis',(0.,0.,-1.));
#32140=DIRECTION('ref_axis',(-1.,0.,0.));
#32141=DIRECTION('center_axis',(0.,0.,-1.));
#32142=DIRECTION('ref_axis',(1.,0.,0.));
#32143=DIRECTION('center_axis',(0.,0.,1.));
#32144=DIRECTION('ref_axis',(-1.,-1.64798730217797E-14,0.));
#32145=DIRECTION('center_axis',(0.,0.,1.));
#32146=DIRECTION('ref_axis',(1.,0.,0.));
#32147=DIRECTION('center_axis',(0.,0.,-1.));
#32148=DIRECTION('ref_axis',(1.,0.,0.));
#32149=DIRECTION('center_axis',(0.,0.,1.));
#32150=DIRECTION('ref_axis',(-1.,-1.73472347597681E-14,0.));
#32151=DIRECTION('center_axis',(0.,0.,1.));
#32152=DIRECTION('ref_axis',(1.,0.,0.));
#32153=DIRECTION('center_axis',(0.,0.,-1.));
#32154=DIRECTION('ref_axis',(1.,0.,0.));
#32155=DIRECTION('center_axis',(0.,0.,1.));
#32156=DIRECTION('ref_axis',(-1.,1.95156391047391E-14,0.));
#32157=DIRECTION('center_axis',(0.,0.,-1.));
#32158=DIRECTION('ref_axis',(-1.,0.,0.));
#32159=DIRECTION('center_axis',(0.,-1.,0.));
#32160=DIRECTION('ref_axis',(0.,0.,-1.));
#32161=DIRECTION('',(0.,0.,1.));
#32162=DIRECTION('',(-1.,0.,0.));
#32163=DIRECTION('',(0.,0.,1.));
#32164=DIRECTION('',(1.,0.,0.));
#32165=DIRECTION('center_axis',(0.,0.,-1.));
#32166=DIRECTION('ref_axis',(-1.,0.,0.));
#32167=DIRECTION('',(-0.707106781186547,0.707106781186548,0.));
#32168=DIRECTION('',(-1.26161707343768E-16,1.,0.));
#32169=DIRECTION('',(0.707106781186562,0.707106781186533,0.));
#32170=DIRECTION('',(0.707106781186562,-0.707106781186533,0.));
#32171=DIRECTION('',(-1.26161707343768E-16,-1.,0.));
#32172=DIRECTION('',(-0.707106781186547,-0.707106781186548,0.));
#32173=DIRECTION('center_axis',(0.707106781186533,-0.707106781186562,0.));
#32174=DIRECTION('ref_axis',(0.707106781186562,0.707106781186533,0.));
#32175=DIRECTION('',(0.,0.,1.));
#32176=DIRECTION('',(-0.707106781186562,-0.707106781186533,0.));
#32177=DIRECTION('center_axis',(1.,1.26161707343768E-16,0.));
#32178=DIRECTION('ref_axis',(-1.26161707343768E-16,1.,0.));
#32179=DIRECTION('',(0.,0.,1.));
#32180=DIRECTION('',(1.26161707343768E-16,-1.,0.));
#32181=DIRECTION('center_axis',(0.707106781186548,0.707106781186547,0.));
#32182=DIRECTION('ref_axis',(-0.707106781186547,0.707106781186548,0.));
#32183=DIRECTION('',(0.707106781186547,-0.707106781186548,0.));
#32184=DIRECTION('center_axis',(-0.707106781186548,0.707106781186547,0.));
#32185=DIRECTION('ref_axis',(-0.707106781186547,-0.707106781186548,0.));
#32186=DIRECTION('',(0.,0.,1.));
#32187=DIRECTION('',(0.707106781186547,0.707106781186548,0.));
#32188=DIRECTION('center_axis',(-1.,1.26161707343768E-16,0.));
#32189=DIRECTION('ref_axis',(-1.26161707343768E-16,-1.,0.));
#32190=DIRECTION('',(0.,0.,1.));
#32191=DIRECTION('',(1.26161707343768E-16,1.,0.));
#32192=DIRECTION('center_axis',(-0.707106781186533,-0.707106781186562,0.));
#32193=DIRECTION('ref_axis',(0.707106781186562,-0.707106781186533,0.));
#32194=DIRECTION('',(-0.707106781186562,0.707106781186533,0.));
#32195=DIRECTION('center_axis',(-0.866025403784439,0.5,0.));
#32196=DIRECTION('ref_axis',(-0.5,-0.866025403784439,0.));
#32197=DIRECTION('',(0.,0.,-1.));
#32198=DIRECTION('',(0.,0.,-1.));
#32199=DIRECTION('',(0.5,0.866025403784439,0.));
#32200=DIRECTION('center_axis',(-0.866025403784438,-0.5,0.));
#32201=DIRECTION('ref_axis',(0.5,-0.866025403784438,0.));
#32202=DIRECTION('',(-0.5,0.866025403784438,0.));
#32203=DIRECTION('',(0.,0.,-1.));
#32204=DIRECTION('center_axis',(7.51157299368579E-16,-1.,0.));
#32205=DIRECTION('ref_axis',(1.,7.5115729936858E-16,0.));
#32206=DIRECTION('',(0.,0.,-1.));
#32207=DIRECTION('',(-1.,-7.5115729936858E-16,0.));
#32208=DIRECTION('center_axis',(0.866025403784439,-0.5,0.));
#32209=DIRECTION('ref_axis',(0.5,0.866025403784439,0.));
#32210=DIRECTION('',(0.,0.,-1.));
#32211=DIRECTION('',(-0.5,-0.866025403784439,0.));
#32212=DIRECTION('center_axis',(0.866025403784439,0.5,0.));
#32213=DIRECTION('ref_axis',(-0.5,0.866025403784439,0.));
#32214=DIRECTION('',(0.,0.,-1.));
#32215=DIRECTION('',(0.5,-0.866025403784438,0.));
#32216=DIRECTION('center_axis',(0.,1.,0.));
#32217=DIRECTION('ref_axis',(0.,0.,1.));
#32218=DIRECTION('',(1.,0.,0.));
#32219=DIRECTION('center_axis',(0.,0.,-1.));
#32220=DIRECTION('ref_axis',(-1.,0.,0.));
#32221=DIRECTION('center_axis',(0.,0.,-1.));
#32222=DIRECTION('ref_axis',(1.,0.,0.));
#32223=DIRECTION('',(0.707106781186546,-0.707106781186549,0.));
#32224=DIRECTION('center_axis',(0.,0.,1.));
#32225=DIRECTION('ref_axis',(1.,0.,0.));
#32226=DIRECTION('',(0.,-1.,0.));
#32227=DIRECTION('center_axis',(0.,0.,1.));
#32228=DIRECTION('ref_axis',(1.,0.,0.));
#32229=DIRECTION('',(-0.707106781186552,-0.707106781186543,0.));
#32230=DIRECTION('center_axis',(0.,0.,-1.));
#32231=DIRECTION('ref_axis',(1.,0.,0.));
#32232=DIRECTION('center_axis',(0.,0.,1.));
#32233=DIRECTION('ref_axis',(1.,0.,0.));
#32234=DIRECTION('center_axis',(0.,0.,-1.));
#32235=DIRECTION('ref_axis',(1.,0.,0.));
#32236=DIRECTION('',(-0.707106781186552,-0.707106781186543,0.));
#32237=DIRECTION('center_axis',(0.,0.,-1.));
#32238=DIRECTION('ref_axis',(1.,0.,0.));
#32239=DIRECTION('',(0.,-1.,0.));
#32240=DIRECTION('center_axis',(0.,0.,-1.));
#32241=DIRECTION('ref_axis',(1.,0.,0.));
#32242=DIRECTION('',(0.707106781186547,-0.707106781186547,0.));
#32243=DIRECTION('center_axis',(0.,0.,-1.));
#32244=DIRECTION('ref_axis',(1.,0.,0.));
#32245=DIRECTION('center_axis',(0.,0.,1.));
#32246=DIRECTION('ref_axis',(1.,0.,0.));
#32247=DIRECTION('center_axis',(0.,0.,-1.));
#32248=DIRECTION('ref_axis',(1.,0.,0.));
#32249=DIRECTION('',(0.707106781186546,-0.707106781186549,0.));
#32250=DIRECTION('',(1.,4.61786466713945E-17,0.));
#32251=DIRECTION('',(0.707106781186547,0.707106781186548,0.));
#32252=DIRECTION('center_axis',(0.,0.,-1.));
#32253=DIRECTION('ref_axis',(1.,0.,0.));
#32254=DIRECTION('center_axis',(0.,0.,1.));
#32255=DIRECTION('ref_axis',(1.,0.,0.));
#32256=DIRECTION('center_axis',(0.,0.,-1.));
#32257=DIRECTION('ref_axis',(1.,0.,0.));
#32258=DIRECTION('',(0.707106781186546,0.707106781186549,0.));
#32259=DIRECTION('center_axis',(0.,0.,-1.));
#32260=DIRECTION('ref_axis',(1.,0.,0.));
#32261=DIRECTION('',(0.,1.,0.));
#32262=DIRECTION('center_axis',(0.,0.,-1.));
#32263=DIRECTION('ref_axis',(1.,0.,0.));
#32264=DIRECTION('',(-0.707106781186546,0.707106781186549,0.));
#32265=DIRECTION('center_axis',(0.,0.,-1.));
#32266=DIRECTION('ref_axis',(1.,0.,0.));
#32267=DIRECTION('center_axis',(0.,0.,1.));
#32268=DIRECTION('ref_axis',(1.,0.,0.));
#32269=DIRECTION('center_axis',(0.,0.,-1.));
#32270=DIRECTION('ref_axis',(1.,0.,0.));
#32271=DIRECTION('',(-0.707106781186552,0.707106781186543,0.));
#32272=DIRECTION('center_axis',(0.,0.,1.));
#32273=DIRECTION('ref_axis',(1.,0.,0.));
#32274=DIRECTION('',(0.,1.,0.));
#32275=DIRECTION('center_axis',(0.,0.,1.));
#32276=DIRECTION('ref_axis',(1.,0.,0.));
#32277=DIRECTION('',(0.707106781186546,0.707106781186549,0.));
#32278=DIRECTION('',(1.,0.,0.));
#32279=DIRECTION('',(0.707106781186547,-0.707106781186548,0.));
#32280=DIRECTION('',(1.26352022694434E-16,-1.,0.));
#32281=DIRECTION('',(-0.707106781186562,-0.707106781186533,0.));
#32282=DIRECTION('',(-1.,-1.95534159233113E-16,0.));
#32283=DIRECTION('',(-0.707106781186561,0.707106781186534,0.));
#32284=DIRECTION('',(0.,1.,0.));
#32285=DIRECTION('',(0.707106781186546,0.707106781186549,0.));
#32286=DIRECTION('',(1.,0.,0.));
#32287=DIRECTION('center_axis',(-0.707106781186549,-0.707106781186546,0.));
#32288=DIRECTION('ref_axis',(0.707106781186546,-0.707106781186549,0.));
#32289=DIRECTION('',(0.707106781186546,-0.707106781186549,0.));
#32290=DIRECTION('',(0.,0.,1.));
#32291=DIRECTION('',(0.,0.,1.));
#32292=DIRECTION('center_axis',(0.,0.,1.));
#32293=DIRECTION('ref_axis',(1.,0.,0.));
#32294=DIRECTION('center_axis',(0.,0.,1.));
#32295=DIRECTION('ref_axis',(1.,0.,0.));
#32296=DIRECTION('',(0.,0.,1.));
#32297=DIRECTION('center_axis',(-1.,0.,0.));
#32298=DIRECTION('ref_axis',(0.,0.,1.));
#32299=DIRECTION('',(0.,-1.,0.));
#32300=DIRECTION('',(0.,0.,1.));
#32301=DIRECTION('center_axis',(0.,0.,1.));
#32302=DIRECTION('ref_axis',(1.,0.,0.));
#32303=DIRECTION('center_axis',(0.,0.,1.));
#32304=DIRECTION('ref_axis',(1.,0.,0.));
#32305=DIRECTION('',(0.,0.,1.));
#32306=DIRECTION('center_axis',(-0.707106781186543,0.707106781186552,0.));
#32307=DIRECTION('ref_axis',(-0.707106781186552,-0.707106781186543,0.));
#32308=DIRECTION('',(-0.707106781186552,-0.707106781186543,0.));
#32309=DIRECTION('',(0.,0.,1.));
#32310=DIRECTION('center_axis',(0.,0.,1.));
#32311=DIRECTION('ref_axis',(1.,0.,0.));
#32312=DIRECTION('center_axis',(0.,0.,-1.));
#32313=DIRECTION('ref_axis',(1.,0.,0.));
#32314=DIRECTION('',(0.,0.,1.));
#32315=DIRECTION('center_axis',(0.,0.,1.));
#32316=DIRECTION('ref_axis',(1.,0.,0.));
#32317=DIRECTION('center_axis',(0.,0.,1.));
#32318=DIRECTION('ref_axis',(1.,0.,0.));
#32319=DIRECTION('',(0.,0.,1.));
#32320=DIRECTION('center_axis',(0.,0.,1.));
#32321=DIRECTION('ref_axis',(1.,0.,0.));
#32322=DIRECTION('center_axis',(0.,0.,-1.));
#32323=DIRECTION('ref_axis',(1.,0.,0.));
#32324=DIRECTION('',(0.,0.,1.));
#32325=DIRECTION('center_axis',(-0.707106781186543,0.707106781186552,0.));
#32326=DIRECTION('ref_axis',(-0.707106781186552,-0.707106781186543,0.));
#32327=DIRECTION('',(-0.707106781186552,-0.707106781186543,0.));
#32328=DIRECTION('',(0.,0.,1.));
#32329=DIRECTION('center_axis',(0.,0.,1.));
#32330=DIRECTION('ref_axis',(1.,0.,0.));
#32331=DIRECTION('center_axis',(0.,0.,-1.));
#32332=DIRECTION('ref_axis',(1.,0.,0.));
#32333=DIRECTION('',(0.,0.,1.));
#32334=DIRECTION('center_axis',(-1.,0.,0.));
#32335=DIRECTION('ref_axis',(0.,0.,1.));
#32336=DIRECTION('',(0.,-1.,0.));
#32337=DIRECTION('',(0.,0.,1.));
#32338=DIRECTION('center_axis',(0.,0.,1.));
#32339=DIRECTION('ref_axis',(1.,0.,0.));
#32340=DIRECTION('center_axis',(0.,0.,-1.));
#32341=DIRECTION('ref_axis',(1.,0.,0.));
#32342=DIRECTION('',(0.,0.,1.));
#32343=DIRECTION('center_axis',(-0.707106781186548,-0.707106781186548,0.));
#32344=DIRECTION('ref_axis',(0.707106781186548,-0.707106781186548,0.));
#32345=DIRECTION('',(0.707106781186547,-0.707106781186547,0.));
#32346=DIRECTION('',(0.,0.,1.));
#32347=DIRECTION('center_axis',(0.,0.,1.));
#32348=DIRECTION('ref_axis',(1.,0.,0.));
#32349=DIRECTION('center_axis',(0.,0.,-1.));
#32350=DIRECTION('ref_axis',(1.,0.,0.));
#32351=DIRECTION('',(0.,0.,1.));
#32352=DIRECTION('center_axis',(0.,0.,1.));
#32353=DIRECTION('ref_axis',(1.,0.,0.));
#32354=DIRECTION('center_axis',(0.,0.,1.));
#32355=DIRECTION('ref_axis',(1.,0.,0.));
#32356=DIRECTION('',(0.,0.,1.));
#32357=DIRECTION('center_axis',(0.,0.,1.));
#32358=DIRECTION('ref_axis',(1.,0.,0.));
#32359=DIRECTION('center_axis',(0.,0.,-1.));
#32360=DIRECTION('ref_axis',(1.,0.,0.));
#32361=DIRECTION('',(0.,0.,1.));
#32362=DIRECTION('center_axis',(-0.707106781186549,-0.707106781186546,0.));
#32363=DIRECTION('ref_axis',(0.707106781186546,-0.707106781186549,0.));
#32364=DIRECTION('',(0.707106781186546,-0.707106781186549,0.));
#32365=DIRECTION('',(0.,0.,1.));
#32366=DIRECTION('center_axis',(4.61786466713945E-17,-1.,0.));
#32367=DIRECTION('ref_axis',(1.,4.61786466713945E-17,0.));
#32368=DIRECTION('',(1.,4.61786466713945E-17,0.));
#32369=DIRECTION('',(0.,0.,1.));
#32370=DIRECTION('center_axis',(0.707106781186548,-0.707106781186547,0.));
#32371=DIRECTION('ref_axis',(0.707106781186547,0.707106781186548,0.));
#32372=DIRECTION('',(0.707106781186547,0.707106781186548,0.));
#32373=DIRECTION('',(0.,0.,1.));
#32374=DIRECTION('center_axis',(0.,0.,1.));
#32375=DIRECTION('ref_axis',(1.,0.,0.));
#32376=DIRECTION('center_axis',(0.,0.,-1.));
#32377=DIRECTION('ref_axis',(1.,0.,0.));
#32378=DIRECTION('',(0.,0.,1.));
#32379=DIRECTION('center_axis',(0.,0.,1.));
#32380=DIRECTION('ref_axis',(1.,0.,0.));
#32381=DIRECTION('center_axis',(0.,0.,1.));
#32382=DIRECTION('ref_axis',(1.,0.,0.));
#32383=DIRECTION('',(0.,0.,1.));
#32384=DIRECTION('center_axis',(0.,0.,1.));
#32385=DIRECTION('ref_axis',(1.,0.,0.));
#32386=DIRECTION('center_axis',(0.,0.,-1.));
#32387=DIRECTION('ref_axis',(1.,0.,0.));
#32388=DIRECTION('',(0.,0.,1.));
#32389=DIRECTION('center_axis',(0.70710678118655,-0.707106781186545,0.));
#32390=DIRECTION('ref_axis',(0.707106781186545,0.70710678118655,0.));
#32391=DIRECTION('',(0.707106781186546,0.707106781186549,0.));
#32392=DIRECTION('',(0.,0.,1.));
#32393=DIRECTION('center_axis',(0.,0.,1.));
#32394=DIRECTION('ref_axis',(1.,0.,0.));
#32395=DIRECTION('center_axis',(0.,0.,-1.));
#32396=DIRECTION('ref_axis',(1.,0.,0.));
#32397=DIRECTION('',(0.,0.,1.));
#32398=DIRECTION('center_axis',(1.,0.,0.));
#32399=DIRECTION('ref_axis',(0.,0.,-1.));
#32400=DIRECTION('',(0.,1.,0.));
#32401=DIRECTION('',(0.,0.,1.));
#32402=DIRECTION('center_axis',(0.,0.,1.));
#32403=DIRECTION('ref_axis',(1.,0.,0.));
#32404=DIRECTION('center_axis',(0.,0.,-1.));
#32405=DIRECTION('ref_axis',(1.,0.,0.));
#32406=DIRECTION('',(0.,0.,1.));
#32407=DIRECTION('center_axis',(0.707106781186549,0.707106781186546,0.));
#32408=DIRECTION('ref_axis',(-0.707106781186546,0.707106781186549,0.));
#32409=DIRECTION('',(-0.707106781186546,0.707106781186549,0.));
#32410=DIRECTION('',(0.,0.,1.));
#32411=DIRECTION('center_axis',(0.,0.,1.));
#32412=DIRECTION('ref_axis',(1.,0.,0.));
#32413=DIRECTION('center_axis',(0.,0.,-1.));
#32414=DIRECTION('ref_axis',(1.,0.,0.));
#32415=DIRECTION('',(0.,0.,1.));
#32416=DIRECTION('center_axis',(0.,0.,1.));
#32417=DIRECTION('ref_axis',(1.,0.,0.));
#32418=DIRECTION('center_axis',(0.,0.,1.));
#32419=DIRECTION('ref_axis',(1.,0.,0.));
#32420=DIRECTION('',(0.,0.,1.));
#32421=DIRECTION('center_axis',(0.,0.,1.));
#32422=DIRECTION('ref_axis',(1.,0.,0.));
#32423=DIRECTION('center_axis',(0.,0.,-1.));
#32424=DIRECTION('ref_axis',(1.,0.,0.));
#32425=DIRECTION('',(0.,0.,1.));
#32426=DIRECTION('center_axis',(0.707106781186543,0.707106781186552,0.));
#32427=DIRECTION('ref_axis',(-0.707106781186553,0.707106781186543,0.));
#32428=DIRECTION('',(-0.707106781186552,0.707106781186543,0.));
#32429=DIRECTION('',(0.,0.,1.));
#32430=DIRECTION('center_axis',(0.,0.,1.));
#32431=DIRECTION('ref_axis',(1.,0.,0.));
#32432=DIRECTION('center_axis',(0.,0.,1.));
#32433=DIRECTION('ref_axis',(1.,0.,0.));
#32434=DIRECTION('',(0.,0.,1.));
#32435=DIRECTION('center_axis',(1.,0.,0.));
#32436=DIRECTION('ref_axis',(0.,0.,-1.));
#32437=DIRECTION('',(0.,1.,0.));
#32438=DIRECTION('',(0.,0.,1.));
#32439=DIRECTION('center_axis',(0.,0.,1.));
#32440=DIRECTION('ref_axis',(1.,0.,0.));
#32441=DIRECTION('center_axis',(0.,0.,1.));
#32442=DIRECTION('ref_axis',(1.,0.,0.));
#32443=DIRECTION('',(0.,0.,1.));
#32444=DIRECTION('center_axis',(0.707106781186549,-0.707106781186546,0.));
#32445=DIRECTION('ref_axis',(0.707106781186546,0.707106781186549,0.));
#32446=DIRECTION('',(0.707106781186546,0.707106781186549,0.));
#32447=DIRECTION('',(0.,0.,1.));
#32448=DIRECTION('center_axis',(0.,-1.,0.));
#32449=DIRECTION('ref_axis',(0.,0.,-1.));
#32450=DIRECTION('',(1.,0.,0.));
#32451=DIRECTION('',(0.,0.,1.));
#32452=DIRECTION('center_axis',(-0.707106781186548,-0.707106781186547,0.));
#32453=DIRECTION('ref_axis',(0.707106781186547,-0.707106781186548,0.));
#32454=DIRECTION('',(0.707106781186547,-0.707106781186548,0.));
#32455=DIRECTION('',(0.,0.,1.));
#32456=DIRECTION('center_axis',(-1.,-1.26352022694434E-16,0.));
#32457=DIRECTION('ref_axis',(1.26352022694434E-16,-1.,0.));
#32458=DIRECTION('',(1.26352022694434E-16,-1.,0.));
#32459=DIRECTION('',(0.,0.,1.));
#32460=DIRECTION('center_axis',(-0.707106781186533,0.707106781186562,0.));
#32461=DIRECTION('ref_axis',(-0.707106781186562,-0.707106781186533,0.));
#32462=DIRECTION('',(-0.707106781186562,-0.707106781186533,0.));
#32463=DIRECTION('',(0.,0.,1.));
#32464=DIRECTION('center_axis',(-1.95534159233113E-16,1.,0.));
#32465=DIRECTION('ref_axis',(-1.,-1.95534159233113E-16,0.));
#32466=DIRECTION('',(-1.,-1.95534159233113E-16,0.));
#32467=DIRECTION('',(0.,0.,1.));
#32468=DIRECTION('center_axis',(0.707106781186534,0.707106781186561,0.));
#32469=DIRECTION('ref_axis',(-0.707106781186561,0.707106781186534,0.));
#32470=DIRECTION('',(-0.707106781186561,0.707106781186534,0.));
#32471=DIRECTION('',(0.,0.,1.));
#32472=DIRECTION('center_axis',(1.,0.,0.));
#32473=DIRECTION('ref_axis',(0.,0.,-1.));
#32474=DIRECTION('',(0.,1.,0.));
#32475=DIRECTION('',(0.,0.,1.));
#32476=DIRECTION('center_axis',(0.707106781186549,-0.707106781186546,0.));
#32477=DIRECTION('ref_axis',(0.707106781186546,0.707106781186549,0.));
#32478=DIRECTION('',(0.707106781186546,0.707106781186549,0.));
#32479=DIRECTION('',(0.,0.,1.));
#32480=DIRECTION('center_axis',(0.,-1.,0.));
#32481=DIRECTION('ref_axis',(0.,0.,-1.));
#32482=DIRECTION('',(1.,0.,0.));
#32483=DIRECTION('center_axis',(-1.30104260698261E-15,1.,-1.73611473352215E-31));
#32484=DIRECTION('ref_axis',(-1.,-1.30104260698261E-15,0.));
#32485=DIRECTION('center_axis',(-1.30104260698261E-15,1.,-1.73611473352215E-31));
#32486=DIRECTION('ref_axis',(-1.,-1.30104260698261E-15,0.));
#32487=DIRECTION('',(4.33680868994202E-17,0.,1.));
#32488=DIRECTION('center_axis',(-1.30104260698261E-15,1.,-1.73611473352215E-31));
#32489=DIRECTION('ref_axis',(-1.,-1.30104260698261E-15,2.25875923892257E-46));
#32490=DIRECTION('',(4.33680868994202E-17,0.,-1.));
#32491=DIRECTION('center_axis',(0.,0.,-1.));
#32492=DIRECTION('ref_axis',(-1.,0.,0.));
#32493=DIRECTION('',(1.,0.,0.));
#32494=DIRECTION('',(-1.73472347597681E-16,1.,0.));
#32495=DIRECTION('center_axis',(0.,0.,1.));
#32496=DIRECTION('ref_axis',(1.,0.,0.));
#32497=DIRECTION('',(-1.73472347597681E-16,-1.,0.));
#32498=DIRECTION('',(1.,0.,0.));
#32499=DIRECTION('',(0.707106781186562,0.707106781186533,0.));
#32500=DIRECTION('',(-1.26161707343768E-16,1.,0.));
#32501=DIRECTION('',(-0.707106781186547,0.707106781186548,0.));
#32502=DIRECTION('',(1.,0.,0.));
#32503=DIRECTION('',(0.707106781186546,0.707106781186549,0.));
#32504=DIRECTION('center_axis',(0.,0.,1.));
#32505=DIRECTION('ref_axis',(-1.,0.,0.));
#32506=DIRECTION('',(0.,1.,0.));
#32507=DIRECTION('center_axis',(0.,0.,1.));
#32508=DIRECTION('ref_axis',(-1.,0.,0.));
#32509=DIRECTION('',(-0.707106781186549,0.707106781186546,0.));
#32510=DIRECTION('center_axis',(0.,0.,-1.));
#32511=DIRECTION('ref_axis',(-1.,0.,0.));
#32512=DIRECTION('center_axis',(0.,0.,1.));
#32513=DIRECTION('ref_axis',(1.,0.,0.));
#32514=DIRECTION('center_axis',(0.,0.,-1.));
#32515=DIRECTION('ref_axis',(-1.,0.,0.));
#32516=DIRECTION('',(-0.707106781186549,0.707106781186546,0.));
#32517=DIRECTION('center_axis',(0.,0.,-1.));
#32518=DIRECTION('ref_axis',(-1.,0.,0.));
#32519=DIRECTION('',(0.,1.,0.));
#32520=DIRECTION('center_axis',(0.,0.,-1.));
#32521=DIRECTION('ref_axis',(-1.,0.,0.));
#32522=DIRECTION('',(0.707106781186546,0.707106781186549,0.));
#32523=DIRECTION('center_axis',(0.,0.,-1.));
#32524=DIRECTION('ref_axis',(-1.,0.,0.));
#32525=DIRECTION('center_axis',(0.,0.,1.));
#32526=DIRECTION('ref_axis',(1.,0.,0.));
#32527=DIRECTION('center_axis',(0.,0.,-1.));
#32528=DIRECTION('ref_axis',(-1.,0.,0.));
#32529=DIRECTION('',(0.707106781186546,0.707106781186549,0.));
#32530=DIRECTION('',(1.,1.22464679914735E-16,0.));
#32531=DIRECTION('',(0.707106781186546,-0.707106781186549,0.));
#32532=DIRECTION('center_axis',(0.,0.,-1.));
#32533=DIRECTION('ref_axis',(-1.,0.,0.));
#32534=DIRECTION('center_axis',(0.,0.,1.));
#32535=DIRECTION('ref_axis',(1.,0.,0.));
#32536=DIRECTION('center_axis',(0.,0.,-1.));
#32537=DIRECTION('ref_axis',(-1.,0.,0.));
#32538=DIRECTION('',(0.707106781186546,-0.707106781186549,0.));
#32539=DIRECTION('center_axis',(0.,0.,-1.));
#32540=DIRECTION('ref_axis',(-1.,0.,0.));
#32541=DIRECTION('',(0.,-1.,0.));
#32542=DIRECTION('center_axis',(0.,0.,-1.));
#32543=DIRECTION('ref_axis',(-1.,0.,0.));
#32544=DIRECTION('',(-0.707106781186549,-0.707106781186546,0.));
#32545=DIRECTION('center_axis',(0.,0.,-1.));
#32546=DIRECTION('ref_axis',(-1.,0.,0.));
#32547=DIRECTION('center_axis',(0.,0.,1.));
#32548=DIRECTION('ref_axis',(1.,0.,0.));
#32549=DIRECTION('center_axis',(0.,0.,-1.));
#32550=DIRECTION('ref_axis',(-1.,0.,0.));
#32551=DIRECTION('',(-0.707106781186549,-0.707106781186546,0.));
#32552=DIRECTION('center_axis',(0.,0.,1.));
#32553=DIRECTION('ref_axis',(-1.,-3.46944695195361E-15,0.));
#32554=DIRECTION('',(0.,-1.,0.));
#32555=DIRECTION('center_axis',(0.,0.,1.));
#32556=DIRECTION('ref_axis',(-1.,0.,0.));
#32557=DIRECTION('',(0.707106781186546,-0.707106781186549,0.));
#32558=DIRECTION('',(1.,-6.49101394191508E-16,0.));
#32559=DIRECTION('',(-0.707106781186547,-0.707106781186548,0.));
#32560=DIRECTION('',(-1.26161707343768E-16,-1.,0.));
#32561=DIRECTION('',(0.707106781186562,-0.707106781186533,0.));
#32562=DIRECTION('center_axis',(1.,1.30104260698261E-15,4.33680868994202E-17));
#32563=DIRECTION('ref_axis',(-1.30104260698261E-15,1.,5.08894400801554E-48));
#32564=DIRECTION('',(4.33680868994202E-17,0.,-1.));
#32565=DIRECTION('',(-1.30104260698261E-15,1.,-1.73611473352215E-31));
#32566=DIRECTION('center_axis',(-1.,-1.30104260698261E-15,4.33680868994202E-17));
#32567=DIRECTION('ref_axis',(1.30104260698261E-15,-1.,5.08894400801554E-48));
#32568=DIRECTION('',(4.33680868994202E-17,0.,1.));
#32569=DIRECTION('',(-1.30104260698261E-15,1.,-1.73611473352215E-31));
#32570=DIRECTION('center_axis',(-1.30104260698261E-15,1.,-1.73611473352215E-31));
#32571=DIRECTION('ref_axis',(-1.,-1.30104260698261E-15,2.25875923892257E-46));
#32572=DIRECTION('center_axis',(-1.30104260698261E-15,1.,-1.73611473352215E-31));
#32573=DIRECTION('ref_axis',(-1.,-1.30104260698261E-15,2.25875923892257E-46));
#32574=DIRECTION('center_axis',(-1.30104260698261E-15,1.,-1.73611473352215E-31));
#32575=DIRECTION('ref_axis',(-1.,-1.30104260698261E-15,0.));
#32576=DIRECTION('center_axis',(-1.30104260698261E-15,1.,-1.73611473352215E-31));
#32577=DIRECTION('ref_axis',(-1.,-1.30104260698261E-15,0.));
#32578=DIRECTION('',(-1.3010426069826E-16,0.,-1.));
#32579=DIRECTION('center_axis',(-1.30104260698261E-15,1.,-1.73611473352215E-31));
#32580=DIRECTION('ref_axis',(-1.,-1.30104260698261E-15,2.25875923892257E-46));
#32581=DIRECTION('',(1.3010426069826E-16,0.,1.));
#32582=DIRECTION('center_axis',(-6.49101394191508E-16,-1.,0.));
#32583=DIRECTION('ref_axis',(1.,-6.49101394191508E-16,0.));
#32584=DIRECTION('',(1.,-3.50803534070133E-16,0.));
#32585=DIRECTION('',(0.,0.,1.));
#32586=DIRECTION('',(0.,0.,1.));
#32587=DIRECTION('center_axis',(-0.707106781186548,0.707106781186547,0.));
#32588=DIRECTION('ref_axis',(-0.707106781186547,-0.707106781186548,0.));
#32589=DIRECTION('',(0.707106781186547,0.707106781186548,0.));
#32590=DIRECTION('',(0.,0.,1.));
#32591=DIRECTION('center_axis',(-1.,1.26161707343768E-16,0.));
#32592=DIRECTION('ref_axis',(-1.26161707343768E-16,-1.,0.));
#32593=DIRECTION('',(1.26161707343768E-16,1.,0.));
#32594=DIRECTION('',(0.,0.,1.));
#32595=DIRECTION('center_axis',(-0.707106781186533,-0.707106781186562,0.));
#32596=DIRECTION('ref_axis',(0.707106781186562,-0.707106781186533,0.));
#32597=DIRECTION('',(-0.707106781186562,0.707106781186533,0.));
#32598=DIRECTION('',(0.,0.,1.));
#32599=DIRECTION('center_axis',(0.,-1.,0.));
#32600=DIRECTION('ref_axis',(0.,0.,-1.));
#32601=DIRECTION('',(-1.,0.,0.));
#32602=DIRECTION('',(0.,0.,1.));
#32603=DIRECTION('',(-1.,0.,0.));
#32604=DIRECTION('',(0.,0.,1.));
#32605=DIRECTION('',(0.,0.,1.));
#32606=DIRECTION('center_axis',(0.707106781186533,-0.707106781186562,0.));
#32607=DIRECTION('ref_axis',(0.707106781186562,0.707106781186533,0.));
#32608=DIRECTION('',(-0.707106781186562,-0.707106781186533,0.));
#32609=DIRECTION('',(0.,0.,1.));
#32610=DIRECTION('center_axis',(1.,1.26161707343768E-16,0.));
#32611=DIRECTION('ref_axis',(-1.26161707343768E-16,1.,0.));
#32612=DIRECTION('',(1.26161707343768E-16,-1.,0.));
#32613=DIRECTION('',(0.,0.,1.));
#32614=DIRECTION('center_axis',(0.707106781186548,0.707106781186547,0.));
#32615=DIRECTION('ref_axis',(-0.707106781186547,0.707106781186548,0.));
#32616=DIRECTION('',(0.707106781186547,-0.707106781186548,0.));
#32617=DIRECTION('',(0.,0.,1.));
#32618=DIRECTION('center_axis',(0.,-1.,0.));
#32619=DIRECTION('ref_axis',(0.,0.,-1.));
#32620=DIRECTION('',(1.,0.,0.));
#32621=DIRECTION('',(0.,0.,1.));
#32622=DIRECTION('center_axis',(0.707106781186549,-0.707106781186546,0.));
#32623=DIRECTION('ref_axis',(0.707106781186546,0.707106781186549,0.));
#32624=DIRECTION('',(0.707106781186546,0.707106781186549,0.));
#32625=DIRECTION('',(0.,0.,1.));
#32626=DIRECTION('center_axis',(0.,0.,1.));
#32627=DIRECTION('ref_axis',(1.,0.,0.));
#32628=DIRECTION('center_axis',(0.,0.,1.));
#32629=DIRECTION('ref_axis',(1.,0.,0.));
#32630=DIRECTION('',(0.,0.,-1.));
#32631=DIRECTION('center_axis',(1.,0.,0.));
#32632=DIRECTION('ref_axis',(0.,0.,-1.));
#32633=DIRECTION('',(0.,1.,0.));
#32634=DIRECTION('',(0.,0.,1.));
#32635=DIRECTION('center_axis',(0.,0.,1.));
#32636=DIRECTION('ref_axis',(1.,0.,0.));
#32637=DIRECTION('center_axis',(0.,0.,1.));
#32638=DIRECTION('ref_axis',(1.,0.,0.));
#32639=DIRECTION('',(0.,0.,-1.));
#32640=DIRECTION('center_axis',(0.707106781186546,0.707106781186549,0.));
#32641=DIRECTION('ref_axis',(-0.707106781186549,0.707106781186546,0.));
#32642=DIRECTION('',(-0.707106781186549,0.707106781186546,0.));
#32643=DIRECTION('',(0.,0.,1.));
#32644=DIRECTION('center_axis',(0.,0.,1.));
#32645=DIRECTION('ref_axis',(1.,0.,0.));
#32646=DIRECTION('center_axis',(0.,0.,-1.));
#32647=DIRECTION('ref_axis',(1.,0.,0.));
#32648=DIRECTION('',(0.,0.,-1.));
#32649=DIRECTION('center_axis',(0.,0.,1.));
#32650=DIRECTION('ref_axis',(1.,0.,0.));
#32651=DIRECTION('center_axis',(0.,0.,1.));
#32652=DIRECTION('ref_axis',(1.,0.,0.));
#32653=DIRECTION('',(0.,0.,1.));
#32654=DIRECTION('center_axis',(0.,0.,1.));
#32655=DIRECTION('ref_axis',(1.,0.,0.));
#32656=DIRECTION('center_axis',(0.,0.,-1.));
#32657=DIRECTION('ref_axis',(1.,0.,0.));
#32658=DIRECTION('',(0.,0.,-1.));
#32659=DIRECTION('center_axis',(0.707106781186546,0.707106781186549,0.));
#32660=DIRECTION('ref_axis',(-0.707106781186549,0.707106781186546,0.));
#32661=DIRECTION('',(-0.707106781186548,0.707106781186547,0.));
#32662=DIRECTION('',(0.,0.,1.));
#32663=DIRECTION('center_axis',(0.,0.,-1.));
#32664=DIRECTION('ref_axis',(-1.,0.,0.));
#32665=DIRECTION('center_axis',(0.,0.,-1.));
#32666=DIRECTION('ref_axis',(1.,0.,0.));
#32667=DIRECTION('',(0.,0.,-1.));
#32668=DIRECTION('center_axis',(1.,0.,0.));
#32669=DIRECTION('ref_axis',(0.,0.,-1.));
#32670=DIRECTION('',(0.,1.,0.));
#32671=DIRECTION('',(0.,0.,1.));
#32672=DIRECTION('center_axis',(0.,0.,-1.));
#32673=DIRECTION('ref_axis',(-1.,0.,0.));
#32674=DIRECTION('center_axis',(0.,0.,-1.));
#32675=DIRECTION('ref_axis',(1.,0.,0.));
#32676=DIRECTION('',(0.,0.,-1.));
#32677=DIRECTION('center_axis',(0.707106781186549,-0.707106781186546,0.));
#32678=DIRECTION('ref_axis',(0.707106781186546,0.707106781186549,0.));
#32679=DIRECTION('',(0.707106781186545,0.70710678118655,0.));
#32680=DIRECTION('',(0.,0.,1.));
#32681=DIRECTION('center_axis',(0.,0.,1.));
#32682=DIRECTION('ref_axis',(1.,0.,0.));
#32683=DIRECTION('center_axis',(0.,0.,-1.));
#32684=DIRECTION('ref_axis',(1.,0.,0.));
#32685=DIRECTION('',(0.,0.,-1.));
#32686=DIRECTION('center_axis',(0.,0.,1.));
#32687=DIRECTION('ref_axis',(1.,0.,0.));
#32688=DIRECTION('center_axis',(0.,0.,1.));
#32689=DIRECTION('ref_axis',(1.,0.,0.));
#32690=DIRECTION('',(0.,0.,1.));
#32691=DIRECTION('center_axis',(0.,0.,1.));
#32692=DIRECTION('ref_axis',(1.,0.,0.));
#32693=DIRECTION('center_axis',(0.,0.,-1.));
#32694=DIRECTION('ref_axis',(1.,0.,0.));
#32695=DIRECTION('',(0.,0.,-1.));
#32696=DIRECTION('center_axis',(0.707106781186549,-0.707106781186546,0.));
#32697=DIRECTION('ref_axis',(0.707106781186546,0.707106781186549,0.));
#32698=DIRECTION('',(0.707106781186546,0.707106781186549,0.));
#32699=DIRECTION('',(0.,0.,1.));
#32700=DIRECTION('center_axis',(1.22464679914735E-16,-1.,0.));
#32701=DIRECTION('ref_axis',(1.,1.22464679914735E-16,0.));
#32702=DIRECTION('',(1.,1.22464679914735E-16,0.));
#32703=DIRECTION('',(0.,0.,1.));
#32704=DIRECTION('center_axis',(-0.707106781186549,-0.707106781186546,0.));
#32705=DIRECTION('ref_axis',(0.707106781186546,-0.707106781186549,0.));
#32706=DIRECTION('',(0.707106781186546,-0.707106781186549,0.));
#32707=DIRECTION('',(0.,0.,1.));
#32708=DIRECTION('center_axis',(0.,0.,1.));
#32709=DIRECTION('ref_axis',(1.,0.,0.));
#32710=DIRECTION('center_axis',(0.,0.,-1.));
#32711=DIRECTION('ref_axis',(1.,0.,0.));
#32712=DIRECTION('',(0.,0.,-1.));
#32713=DIRECTION('center_axis',(0.,0.,1.));
#32714=DIRECTION('ref_axis',(1.,0.,0.));
#32715=DIRECTION('center_axis',(0.,0.,1.));
#32716=DIRECTION('ref_axis',(1.,0.,0.));
#32717=DIRECTION('',(0.,0.,1.));
#32718=DIRECTION('center_axis',(0.,0.,1.));
#32719=DIRECTION('ref_axis',(1.,0.,0.));
#32720=DIRECTION('center_axis',(0.,0.,-1.));
#32721=DIRECTION('ref_axis',(1.,0.,0.));
#32722=DIRECTION('',(0.,0.,-1.));
#32723=DIRECTION('center_axis',(-0.707106781186549,-0.707106781186546,0.));
#32724=DIRECTION('ref_axis',(0.707106781186546,-0.707106781186549,0.));
#32725=DIRECTION('',(0.707106781186545,-0.70710678118655,0.));
#32726=DIRECTION('',(0.,0.,1.));
#32727=DIRECTION('center_axis',(0.,0.,-1.));
#32728=DIRECTION('ref_axis',(-1.,0.,0.));
#32729=DIRECTION('center_axis',(0.,0.,-1.));
#32730=DIRECTION('ref_axis',(1.,0.,0.));
#32731=DIRECTION('',(0.,0.,-1.));
#32732=DIRECTION('center_axis',(-1.,0.,0.));
#32733=DIRECTION('ref_axis',(0.,0.,1.));
#32734=DIRECTION('',(0.,-1.,0.));
#32735=DIRECTION('',(0.,0.,1.));
#32736=DIRECTION('center_axis',(0.,0.,-1.));
#32737=DIRECTION('ref_axis',(-1.,0.,0.));
#32738=DIRECTION('center_axis',(0.,0.,-1.));
#32739=DIRECTION('ref_axis',(1.,0.,0.));
#32740=DIRECTION('',(0.,0.,-1.));
#32741=DIRECTION('center_axis',(-0.707106781186546,0.707106781186549,0.));
#32742=DIRECTION('ref_axis',(-0.707106781186549,-0.707106781186546,0.));
#32743=DIRECTION('',(-0.707106781186548,-0.707106781186547,0.));
#32744=DIRECTION('',(0.,0.,1.));
#32745=DIRECTION('center_axis',(0.,0.,1.));
#32746=DIRECTION('ref_axis',(1.,0.,0.));
#32747=DIRECTION('center_axis',(0.,0.,-1.));
#32748=DIRECTION('ref_axis',(1.,0.,0.));
#32749=DIRECTION('',(0.,0.,-1.));
#32750=DIRECTION('center_axis',(0.,0.,1.));
#32751=DIRECTION('ref_axis',(1.,0.,0.));
#32752=DIRECTION('center_axis',(0.,0.,1.));
#32753=DIRECTION('ref_axis',(1.,0.,0.));
#32754=DIRECTION('',(0.,0.,1.));
#32755=DIRECTION('center_axis',(0.,0.,1.));
#32756=DIRECTION('ref_axis',(1.,0.,0.));
#32757=DIRECTION('center_axis',(0.,0.,-1.));
#32758=DIRECTION('ref_axis',(1.,0.,0.));
#32759=DIRECTION('',(0.,0.,-1.));
#32760=DIRECTION('center_axis',(-0.707106781186546,0.707106781186549,0.));
#32761=DIRECTION('ref_axis',(-0.707106781186549,-0.707106781186546,0.));
#32762=DIRECTION('',(-0.707106781186549,-0.707106781186546,0.));
#32763=DIRECTION('',(0.,0.,1.));
#32764=DIRECTION('center_axis',(0.,0.,1.));
#32765=DIRECTION('ref_axis',(1.,0.,0.));
#32766=DIRECTION('center_axis',(0.,0.,1.));
#32767=DIRECTION('ref_axis',(1.,0.,0.));
#32768=DIRECTION('',(0.,0.,-1.));
#32769=DIRECTION('center_axis',(-1.,0.,0.));
#32770=DIRECTION('ref_axis',(0.,0.,1.));
#32771=DIRECTION('',(0.,-1.,0.));
#32772=DIRECTION('',(0.,0.,1.));
#32773=DIRECTION('center_axis',(0.,0.,1.));
#32774=DIRECTION('ref_axis',(1.,0.,0.));
#32775=DIRECTION('center_axis',(0.,0.,1.));
#32776=DIRECTION('ref_axis',(1.,0.,0.));
#32777=DIRECTION('',(0.,0.,-1.));
#32778=DIRECTION('center_axis',(-0.707106781186549,-0.707106781186546,0.));
#32779=DIRECTION('ref_axis',(0.707106781186546,-0.707106781186549,0.));
#32780=DIRECTION('',(0.707106781186546,-0.707106781186549,0.));
#32781=DIRECTION('center_axis',(-1.30104260698261E-15,1.,-1.73611473352215E-31));
#32782=DIRECTION('ref_axis',(-1.,-1.30104260698261E-15,0.));
#32783=DIRECTION('center_axis',(-7.96355992932556E-18,-1.,0.));
#32784=DIRECTION('ref_axis',(1.,-7.96355992932556E-18,0.));
#32785=DIRECTION('',(0.,0.,1.));
#32786=DIRECTION('',(-1.,7.96355992932556E-18,0.));
#32787=DIRECTION('',(0.,0.,-1.));
#32788=DIRECTION('',(1.,-7.96355992932556E-18,0.));
#32789=DIRECTION('center_axis',(4.11015771401436E-16,-1.,0.));
#32790=DIRECTION('ref_axis',(1.,4.11015771401436E-16,0.));
#32791=DIRECTION('',(0.,0.,1.));
#32792=DIRECTION('',(-1.,-4.11015771401436E-16,0.));
#32793=DIRECTION('',(0.,0.,-1.));
#32794=DIRECTION('',(-1.,-4.11015771401436E-16,0.));
#32795=DIRECTION('center_axis',(-1.,-1.30104260698261E-15,1.3010426069826E-16));
#32796=DIRECTION('ref_axis',(1.30104260698261E-15,-1.,-3.07902494602621E-48));
#32797=DIRECTION('',(1.3010426069826E-16,0.,1.));
#32798=DIRECTION('',(-1.30104260698261E-15,1.,-1.73611473352215E-31));
#32799=DIRECTION('center_axis',(1.,1.30104260698261E-15,-1.3010426069826E-16));
#32800=DIRECTION('ref_axis',(-1.30104260698261E-15,1.,3.07902494602621E-48));
#32801=DIRECTION('',(-1.3010426069826E-16,0.,-1.));
#32802=DIRECTION('',(-1.30104260698261E-15,1.,-1.73611473352215E-31));
#32803=DIRECTION('center_axis',(-1.30104260698261E-15,1.,-1.73611473352215E-31));
#32804=DIRECTION('ref_axis',(-1.,-1.30104260698261E-15,2.25875923892257E-46));
#32805=DIRECTION('center_axis',(-1.30104260698261E-15,1.,-1.73611473352215E-31));
#32806=DIRECTION('ref_axis',(-1.,-1.30104260698261E-15,2.25875923892257E-46));
#32807=DIRECTION('center_axis',(0.,0.,-1.));
#32808=DIRECTION('ref_axis',(-1.,0.,0.));
#32809=DIRECTION('center_axis',(0.,0.,-1.));
#32810=DIRECTION('ref_axis',(1.,0.,0.));
#32811=DIRECTION('center_axis',(0.,0.,1.));
#32812=DIRECTION('ref_axis',(-1.,-1.73472347597681E-15,0.));
#32813=DIRECTION('',(0.,0.,-1.));
#32814=DIRECTION('center_axis',(0.,0.,1.));
#32815=DIRECTION('ref_axis',(1.,0.,0.));
#32816=DIRECTION('',(-0.258819045102518,0.965925826289069,0.));
#32817=DIRECTION('',(2.04085114820801E-16,1.,0.));
#32818=DIRECTION('',(-1.,1.2823896663807E-16,0.));
#32819=DIRECTION('',(-0.707106781186548,0.707106781186547,0.));
#32820=DIRECTION('center_axis',(1.,-2.04085114820801E-16,0.));
#32821=DIRECTION('ref_axis',(2.04085114820801E-16,1.,0.));
#32822=DIRECTION('',(0.,0.,1.));
#32823=DIRECTION('',(0.,1.,0.));
#32824=DIRECTION('',(0.,0.,1.));
#32825=DIRECTION('center_axis',(-1.,-2.04085114820801E-16,0.));
#32826=DIRECTION('ref_axis',(2.04085114820801E-16,-1.,0.));
#32827=DIRECTION('',(0.,0.,1.));
#32828=DIRECTION('',(0.,-1.,0.));
#32829=DIRECTION('',(0.,0.,-1.));
#32830=DIRECTION('',(2.04085114820801E-16,-1.,0.));
#32831=DIRECTION('center_axis',(0.,0.,1.));
#32832=DIRECTION('ref_axis',(1.,0.,0.));
#32833=DIRECTION('',(-0.258819045102518,-0.965925826289069,0.));
#32834=DIRECTION('center_axis',(0.,0.,-1.));
#32835=DIRECTION('ref_axis',(1.,-1.73472347597681E-15,0.));
#32836=DIRECTION('',(-0.707106781186557,-0.707106781186538,0.));
#32837=DIRECTION('',(-1.,-1.2823896663807E-16,0.));
#32838=DIRECTION('center_axis',(0.,0.,-1.));
#32839=DIRECTION('ref_axis',(-1.,0.,0.));
#32840=DIRECTION('',(0.,0.,1.));
#32841=DIRECTION('center_axis',(0.,0.,-1.));
#32842=DIRECTION('ref_axis',(1.,0.,0.));
#32843=DIRECTION('center_axis',(0.,0.,1.));
#32844=DIRECTION('ref_axis',(1.,0.,0.));
#32845=DIRECTION('',(1.,0.,0.));
#32846=DIRECTION('',(0.707106781186546,0.707106781186549,0.));
#32847=DIRECTION('',(0.,1.,0.));
#32848=DIRECTION('',(-0.707106781186561,0.707106781186534,0.));
#32849=DIRECTION('',(-1.,-1.95534159233113E-16,0.));
#32850=DIRECTION('',(-0.707106781186562,-0.707106781186533,0.));
#32851=DIRECTION('',(1.26352022694434E-16,-1.,0.));
#32852=DIRECTION('',(0.707106781186547,-0.707106781186548,0.));
#32853=DIRECTION('',(1.,0.,0.));
#32854=DIRECTION('',(0.707106781186546,0.707106781186549,0.));
#32855=DIRECTION('center_axis',(0.,0.,1.));
#32856=DIRECTION('ref_axis',(1.,0.,0.));
#32857=DIRECTION('',(0.,1.,0.));
#32858=DIRECTION('center_axis',(0.,0.,1.));
#32859=DIRECTION('ref_axis',(1.,0.,0.));
#32860=DIRECTION('',(-0.707106781186552,0.707106781186543,0.));
#32861=DIRECTION('center_axis',(0.,0.,-1.));
#32862=DIRECTION('ref_axis',(1.,0.,0.));
#32863=DIRECTION('center_axis',(0.,0.,1.));
#32864=DIRECTION('ref_axis',(1.,0.,0.));
#32865=DIRECTION('center_axis',(0.,0.,-1.));
#32866=DIRECTION('ref_axis',(1.,0.,0.));
#32867=DIRECTION('',(-0.707106781186546,0.707106781186549,0.));
#32868=DIRECTION('center_axis',(0.,0.,-1.));
#32869=DIRECTION('ref_axis',(1.,0.,0.));
#32870=DIRECTION('',(0.,1.,0.));
#32871=DIRECTION('center_axis',(0.,0.,-1.));
#32872=DIRECTION('ref_axis',(1.,0.,0.));
#32873=DIRECTION('',(0.707106781186546,0.707106781186549,0.));
#32874=DIRECTION('center_axis',(0.,0.,-1.));
#32875=DIRECTION('ref_axis',(1.,0.,0.));
#32876=DIRECTION('center_axis',(0.,0.,1.));
#32877=DIRECTION('ref_axis',(1.,0.,0.));
#32878=DIRECTION('center_axis',(0.,0.,-1.));
#32879=DIRECTION('ref_axis',(1.,0.,0.));
#32880=DIRECTION('',(0.707106781186547,0.707106781186548,0.));
#32881=DIRECTION('',(1.,4.61786466713945E-17,0.));
#32882=DIRECTION('',(0.707106781186546,-0.707106781186549,0.));
#32883=DIRECTION('center_axis',(0.,0.,-1.));
#32884=DIRECTION('ref_axis',(1.,0.,0.));
#32885=DIRECTION('center_axis',(0.,0.,1.));
#32886=DIRECTION('ref_axis',(1.,0.,0.));
#32887=DIRECTION('center_axis',(0.,0.,-1.));
#32888=DIRECTION('ref_axis',(1.,0.,0.));
#32889=DIRECTION('',(0.707106781186547,-0.707106781186547,0.));
#32890=DIRECTION('center_axis',(0.,0.,-1.));
#32891=DIRECTION('ref_axis',(1.,0.,0.));
#32892=DIRECTION('',(0.,-1.,0.));
#32893=DIRECTION('center_axis',(0.,0.,-1.));
#32894=DIRECTION('ref_axis',(1.,0.,0.));
#32895=DIRECTION('',(-0.707106781186552,-0.707106781186543,0.));
#32896=DIRECTION('center_axis',(0.,0.,-1.));
#32897=DIRECTION('ref_axis',(1.,0.,0.));
#32898=DIRECTION('center_axis',(0.,0.,1.));
#32899=DIRECTION('ref_axis',(1.,0.,0.));
#32900=DIRECTION('center_axis',(0.,0.,-1.));
#32901=DIRECTION('ref_axis',(1.,0.,0.));
#32902=DIRECTION('',(-0.707106781186552,-0.707106781186543,0.));
#32903=DIRECTION('center_axis',(0.,0.,1.));
#32904=DIRECTION('ref_axis',(1.,0.,0.));
#32905=DIRECTION('',(0.,-1.,0.));
#32906=DIRECTION('center_axis',(0.,0.,1.));
#32907=DIRECTION('ref_axis',(1.,0.,0.));
#32908=DIRECTION('',(0.707106781186546,-0.707106781186549,0.));
#32909=DIRECTION('center_axis',(-0.707106781186538,0.707106781186557,0.));
#32910=DIRECTION('ref_axis',(0.,0.,1.));
#32911=DIRECTION('',(0.,0.,-1.));
#32912=DIRECTION('',(-0.707106781186557,-0.707106781186538,0.));
#32913=DIRECTION('center_axis',(0.707106781186547,0.707106781186548,0.));
#32914=DIRECTION('ref_axis',(0.,0.,1.));
#32915=DIRECTION('',(0.,0.,1.));
#32916=DIRECTION('',(0.707106781186548,-0.707106781186547,0.));
#32917=DIRECTION('center_axis',(0.,0.,-1.));
#32918=DIRECTION('ref_axis',(-1.,0.,0.));
#32919=DIRECTION('',(-2.04085114820801E-16,-1.,0.));
#32920=DIRECTION('',(0.258819045102518,-0.965925826289069,0.));
#32921=DIRECTION('',(1.,-1.2823896663807E-16,0.));
#32922=DIRECTION('center_axis',(1.,-2.04085114820801E-16,0.));
#32923=DIRECTION('ref_axis',(2.04085114820801E-16,1.,0.));
#32924=DIRECTION('',(0.,0.,-1.));
#32925=DIRECTION('',(0.,-1.,0.));
#32926=DIRECTION('',(0.,0.,1.));
#32927=DIRECTION('center_axis',(0.,0.,1.));
#32928=DIRECTION('ref_axis',(1.,0.,0.));
#32929=DIRECTION('',(1.,1.2823896663807E-16,0.));
#32930=DIRECTION('',(-0.258819045102518,-0.965925826289069,0.));
#32931=DIRECTION('',(-2.04085114820801E-16,1.,0.));
#32932=DIRECTION('center_axis',(-1.,-2.04085114820801E-16,0.));
#32933=DIRECTION('ref_axis',(2.04085114820801E-16,-1.,0.));
#32934=DIRECTION('',(0.,0.,-1.));
#32935=DIRECTION('',(0.,1.,0.));
#32936=DIRECTION('',(0.,0.,-1.));
#32937=DIRECTION('center_axis',(-1.30104260698261E-15,1.,-1.73611473352215E-31));
#32938=DIRECTION('ref_axis',(-1.,-1.30104260698261E-15,0.));
#32939=DIRECTION('center_axis',(-0.965925826289069,-0.258819045102518,0.));
#32940=DIRECTION('ref_axis',(0.258819045102518,-0.965925826289069,0.));
#32941=DIRECTION('center_axis',(-0.965925826289069,-0.258819045102518,0.));
#32942=DIRECTION('ref_axis',(0.258819045102518,-0.965925826289069,0.));
#32943=DIRECTION('center_axis',(-0.965925826289069,-0.258819045102518,0.));
#32944=DIRECTION('ref_axis',(0.258819045102518,-0.965925826289069,0.));
#32945=DIRECTION('center_axis',(-1.2823896663807E-16,1.,0.));
#32946=DIRECTION('ref_axis',(-1.,-1.2823896663807E-16,0.));
#32947=DIRECTION('center_axis',(-1.2823896663807E-16,-1.,0.));
#32948=DIRECTION('ref_axis',(-1.,1.2823896663807E-16,0.));
#32949=DIRECTION('',(0.,0.,-1.));
#32950=DIRECTION('',(-1.,-1.2823896663807E-16,0.));
#32951=DIRECTION('',(0.,0.,1.));
#32952=DIRECTION('center_axis',(-1.,-2.04085114820801E-16,0.));
#32953=DIRECTION('ref_axis',(2.04085114820801E-16,-1.,0.));
#32954=DIRECTION('',(0.,0.,-1.));
#32955=DIRECTION('',(0.,1.,0.));
#32956=DIRECTION('',(2.04085114820801E-16,-1.,0.));
#32957=DIRECTION('center_axis',(-0.965925826289069,-0.258819045102518,0.));
#32958=DIRECTION('ref_axis',(0.258819045102518,-0.965925826289069,0.));
#32959=DIRECTION('center_axis',(-0.965925826289069,-0.258819045102518,0.));
#32960=DIRECTION('ref_axis',(0.258819045102518,-0.965925826289069,0.));
#32961=DIRECTION('',(0.258819045102518,-0.965925826289069,0.));
#32962=DIRECTION('',(0.,0.,1.));
#32963=DIRECTION('center_axis',(1.,-2.04085114820801E-16,0.));
#32964=DIRECTION('ref_axis',(2.04085114820801E-16,1.,0.));
#32965=DIRECTION('',(0.,0.,1.));
#32966=DIRECTION('',(0.,-1.,0.));
#32967=DIRECTION('',(2.04085114820801E-16,1.,0.));
#32968=DIRECTION('center_axis',(1.2823896663807E-16,1.,0.));
#32969=DIRECTION('ref_axis',(-1.,1.2823896663807E-16,0.));
#32970=DIRECTION('',(-1.,1.2823896663807E-16,0.));
#32971=DIRECTION('',(0.,0.,1.));
#32972=DIRECTION('center_axis',(-1.2823896663807E-16,-1.,0.));
#32973=DIRECTION('ref_axis',(-1.,1.2823896663807E-16,0.));
#32974=DIRECTION('center_axis',(0.965925826289069,-0.258819045102518,0.));
#32975=DIRECTION('ref_axis',(0.258819045102518,0.965925826289069,0.));
#32976=DIRECTION('center_axis',(0.965925826289069,-0.258819045102518,0.));
#32977=DIRECTION('ref_axis',(0.258819045102518,0.965925826289069,0.));
#32978=DIRECTION('',(0.258819045102518,0.965925826289069,0.));
#32979=DIRECTION('',(0.,0.,1.));
#32980=DIRECTION('center_axis',(0.965925826289069,-0.258819045102518,0.));
#32981=DIRECTION('ref_axis',(0.258819045102518,0.965925826289069,0.));
#32982=DIRECTION('center_axis',(0.965925826289069,-0.258819045102518,0.));
#32983=DIRECTION('ref_axis',(0.258819045102518,0.965925826289069,0.));
#32984=DIRECTION('center_axis',(0.965925826289069,-0.258819045102518,0.));
#32985=DIRECTION('ref_axis',(0.258819045102518,0.965925826289069,0.));
#32986=DIRECTION('center_axis',(0.,1.,0.));
#32987=DIRECTION('ref_axis',(0.,0.,1.));
#32988=DIRECTION('',(1.,0.,0.));
#32989=DIRECTION('',(0.,0.,-1.));
#32990=DIRECTION('',(0.,0.,-1.));
#32991=DIRECTION('center_axis',(-0.707106781186549,0.707106781186546,0.));
#32992=DIRECTION('ref_axis',(-0.707106781186546,-0.707106781186549,0.));
#32993=DIRECTION('',(0.707106781186546,0.707106781186549,0.));
#32994=DIRECTION('',(0.,0.,-1.));
#32995=DIRECTION('center_axis',(-1.,0.,0.));
#32996=DIRECTION('ref_axis',(0.,0.,1.));
#32997=DIRECTION('',(0.,1.,0.));
#32998=DIRECTION('',(0.,0.,-1.));
#32999=DIRECTION('center_axis',(-0.707106781186534,-0.707106781186561,0.));
#33000=DIRECTION('ref_axis',(0.707106781186561,-0.707106781186534,0.));
#33001=DIRECTION('',(-0.707106781186561,0.707106781186534,0.));
#33002=DIRECTION('',(0.,0.,-1.));
#33003=DIRECTION('center_axis',(1.95534159233113E-16,-1.,0.));
#33004=DIRECTION('ref_axis',(1.,1.95534159233113E-16,0.));
#33005=DIRECTION('',(-1.,-1.95534159233113E-16,0.));
#33006=DIRECTION('',(0.,0.,-1.));
#33007=DIRECTION('center_axis',(0.707106781186533,-0.707106781186562,0.));
#33008=DIRECTION('ref_axis',(0.707106781186562,0.707106781186533,0.));
#33009=DIRECTION('',(-0.707106781186562,-0.707106781186533,0.));
#33010=DIRECTION('',(0.,0.,-1.));
#33011=DIRECTION('center_axis',(1.,1.26352022694434E-16,0.));
#33012=DIRECTION('ref_axis',(-1.26352022694434E-16,1.,0.));
#33013=DIRECTION('',(1.26352022694434E-16,-1.,0.));
#33014=DIRECTION('',(0.,0.,-1.));
#33015=DIRECTION('center_axis',(0.707106781186548,0.707106781186547,0.));
#33016=DIRECTION('ref_axis',(-0.707106781186547,0.707106781186548,0.));
#33017=DIRECTION('',(0.707106781186547,-0.707106781186548,0.));
#33018=DIRECTION('',(0.,0.,-1.));
#33019=DIRECTION('center_axis',(0.,1.,0.));
#33020=DIRECTION('ref_axis',(0.,0.,1.));
#33021=DIRECTION('',(1.,0.,0.));
#33022=DIRECTION('',(0.,0.,-1.));
#33023=DIRECTION('center_axis',(-0.707106781186549,0.707106781186546,0.));
#33024=DIRECTION('ref_axis',(-0.707106781186546,-0.707106781186549,0.));
#33025=DIRECTION('',(0.707106781186546,0.707106781186549,0.));
#33026=DIRECTION('',(0.,0.,-1.));
#33027=DIRECTION('center_axis',(0.,0.,-1.));
#33028=DIRECTION('ref_axis',(-1.,0.,0.));
#33029=DIRECTION('center_axis',(0.,0.,1.));
#33030=DIRECTION('ref_axis',(1.,0.,0.));
#33031=DIRECTION('',(0.,0.,-1.));
#33032=DIRECTION('center_axis',(-1.,0.,0.));
#33033=DIRECTION('ref_axis',(0.,0.,1.));
#33034=DIRECTION('',(0.,1.,0.));
#33035=DIRECTION('',(0.,0.,-1.));
#33036=DIRECTION('center_axis',(0.,0.,-1.));
#33037=DIRECTION('ref_axis',(-1.,0.,0.));
#33038=DIRECTION('center_axis',(0.,0.,1.));
#33039=DIRECTION('ref_axis',(1.,0.,0.));
#33040=DIRECTION('',(0.,0.,-1.));
#33041=DIRECTION('center_axis',(-0.707106781186543,-0.707106781186552,0.));
#33042=DIRECTION('ref_axis',(0.707106781186553,-0.707106781186543,0.));
#33043=DIRECTION('',(-0.707106781186552,0.707106781186543,0.));
#33044=DIRECTION('',(0.,0.,-1.));
#33045=DIRECTION('center_axis',(0.,0.,-1.));
#33046=DIRECTION('ref_axis',(-1.,0.,0.));
#33047=DIRECTION('center_axis',(0.,0.,-1.));
#33048=DIRECTION('ref_axis',(1.,0.,0.));
#33049=DIRECTION('',(0.,0.,-1.));
#33050=DIRECTION('center_axis',(0.,0.,-1.));
#33051=DIRECTION('ref_axis',(-1.,0.,0.));
#33052=DIRECTION('center_axis',(0.,0.,1.));
#33053=DIRECTION('ref_axis',(1.,0.,0.));
#33054=DIRECTION('',(0.,0.,-1.));
#33055=DIRECTION('center_axis',(0.,0.,-1.));
#33056=DIRECTION('ref_axis',(-1.,0.,0.));
#33057=DIRECTION('center_axis',(0.,0.,-1.));
#33058=DIRECTION('ref_axis',(1.,0.,0.));
#33059=DIRECTION('',(0.,0.,-1.));
#33060=DIRECTION('center_axis',(-0.707106781186549,-0.707106781186546,0.));
#33061=DIRECTION('ref_axis',(0.707106781186546,-0.707106781186549,0.));
#33062=DIRECTION('',(-0.707106781186546,0.707106781186549,0.));
#33063=DIRECTION('',(0.,0.,-1.));
#33064=DIRECTION('center_axis',(0.,0.,-1.));
#33065=DIRECTION('ref_axis',(-1.,0.,0.));
#33066=DIRECTION('center_axis',(0.,0.,-1.));
#33067=DIRECTION('ref_axis',(1.,0.,0.));
#33068=DIRECTION('',(0.,0.,-1.));
#33069=DIRECTION('center_axis',(-1.,0.,0.));
#33070=DIRECTION('ref_axis',(0.,0.,1.));
#33071=DIRECTION('',(0.,1.,0.));
#33072=DIRECTION('',(0.,0.,-1.));
#33073=DIRECTION('center_axis',(0.,0.,-1.));
#33074=DIRECTION('ref_axis',(-1.,0.,0.));
#33075=DIRECTION('center_axis',(0.,0.,-1.));
#33076=DIRECTION('ref_axis',(1.,0.,0.));
#33077=DIRECTION('',(0.,0.,-1.));
#33078=DIRECTION('center_axis',(-0.70710678118655,0.707106781186545,0.));
#33079=DIRECTION('ref_axis',(-0.707106781186545,-0.70710678118655,0.));
#33080=DIRECTION('',(0.707106781186546,0.707106781186549,0.));
#33081=DIRECTION('',(0.,0.,-1.));
#33082=DIRECTION('center_axis',(0.,0.,-1.));
#33083=DIRECTION('ref_axis',(-1.,0.,0.));
#33084=DIRECTION('center_axis',(0.,0.,-1.));
#33085=DIRECTION('ref_axis',(1.,0.,0.));
#33086=DIRECTION('',(0.,0.,-1.));
#33087=DIRECTION('center_axis',(0.,0.,-1.));
#33088=DIRECTION('ref_axis',(-1.,0.,0.));
#33089=DIRECTION('center_axis',(0.,0.,1.));
#33090=DIRECTION('ref_axis',(1.,0.,0.));
#33091=DIRECTION('',(0.,0.,-1.));
#33092=DIRECTION('center_axis',(0.,0.,-1.));
#33093=DIRECTION('ref_axis',(-1.,0.,0.));
#33094=DIRECTION('center_axis',(0.,0.,-1.));
#33095=DIRECTION('ref_axis',(1.,0.,0.));
#33096=DIRECTION('',(0.,0.,-1.));
#33097=DIRECTION('center_axis',(-0.707106781186548,0.707106781186547,0.));
#33098=DIRECTION('ref_axis',(-0.707106781186547,-0.707106781186548,0.));
#33099=DIRECTION('',(0.707106781186547,0.707106781186548,0.));
#33100=DIRECTION('',(0.,0.,-1.));
#33101=DIRECTION('center_axis',(-4.61786466713945E-17,1.,0.));
#33102=DIRECTION('ref_axis',(-1.,-4.61786466713945E-17,0.));
#33103=DIRECTION('',(1.,4.61786466713945E-17,0.));
#33104=DIRECTION('',(0.,0.,-1.));
#33105=DIRECTION('center_axis',(0.707106781186549,0.707106781186546,0.));
#33106=DIRECTION('ref_axis',(-0.707106781186546,0.707106781186549,0.));
#33107=DIRECTION('',(0.707106781186546,-0.707106781186549,0.));
#33108=DIRECTION('',(0.,0.,-1.));
#33109=DIRECTION('center_axis',(0.,0.,-1.));
#33110=DIRECTION('ref_axis',(-1.,0.,0.));
#33111=DIRECTION('center_axis',(0.,0.,-1.));
#33112=DIRECTION('ref_axis',(1.,0.,0.));
#33113=DIRECTION('',(0.,0.,-1.));
#33114=DIRECTION('center_axis',(0.,0.,-1.));
#33115=DIRECTION('ref_axis',(-1.,0.,0.));
#33116=DIRECTION('center_axis',(0.,0.,1.));
#33117=DIRECTION('ref_axis',(1.,0.,0.));
#33118=DIRECTION('',(0.,0.,-1.));
#33119=DIRECTION('center_axis',(0.,0.,-1.));
#33120=DIRECTION('ref_axis',(-1.,0.,0.));
#33121=DIRECTION('center_axis',(0.,0.,-1.));
#33122=DIRECTION('ref_axis',(1.,0.,0.));
#33123=DIRECTION('',(0.,0.,-1.));
#33124=DIRECTION('center_axis',(0.707106781186548,0.707106781186548,0.));
#33125=DIRECTION('ref_axis',(-0.707106781186548,0.707106781186548,0.));
#33126=DIRECTION('',(0.707106781186547,-0.707106781186547,0.));
#33127=DIRECTION('',(0.,0.,-1.));
#33128=DIRECTION('center_axis',(0.,0.,-1.));
#33129=DIRECTION('ref_axis',(-1.,0.,0.));
#33130=DIRECTION('center_axis',(0.,0.,-1.));
#33131=DIRECTION('ref_axis',(1.,0.,0.));
#33132=DIRECTION('',(0.,0.,-1.));
#33133=DIRECTION('center_axis',(1.,0.,0.));
#33134=DIRECTION('ref_axis',(0.,0.,-1.));
#33135=DIRECTION('',(0.,-1.,0.));
#33136=DIRECTION('',(0.,0.,-1.));
#33137=DIRECTION('center_axis',(0.,0.,-1.));
#33138=DIRECTION('ref_axis',(-1.,0.,0.));
#33139=DIRECTION('center_axis',(0.,0.,-1.));
#33140=DIRECTION('ref_axis',(1.,0.,0.));
#33141=DIRECTION('',(0.,0.,-1.));
#33142=DIRECTION('center_axis',(0.707106781186543,-0.707106781186552,0.));
#33143=DIRECTION('ref_axis',(0.707106781186552,0.707106781186543,0.));
#33144=DIRECTION('',(-0.707106781186552,-0.707106781186543,0.));
#33145=DIRECTION('',(0.,0.,-1.));
#33146=DIRECTION('center_axis',(0.,0.,-1.));
#33147=DIRECTION('ref_axis',(-1.,0.,0.));
#33148=DIRECTION('center_axis',(0.,0.,-1.));
#33149=DIRECTION('ref_axis',(1.,0.,0.));
#33150=DIRECTION('',(0.,0.,-1.));
#33151=DIRECTION('center_axis',(0.,0.,-1.));
#33152=DIRECTION('ref_axis',(-1.,0.,0.));
#33153=DIRECTION('center_axis',(0.,0.,1.));
#33154=DIRECTION('ref_axis',(1.,0.,0.));
#33155=DIRECTION('',(0.,0.,-1.));
#33156=DIRECTION('center_axis',(0.,0.,-1.));
#33157=DIRECTION('ref_axis',(-1.,0.,0.));
#33158=DIRECTION('center_axis',(0.,0.,-1.));
#33159=DIRECTION('ref_axis',(1.,0.,0.));
#33160=DIRECTION('',(0.,0.,-1.));
#33161=DIRECTION('center_axis',(0.707106781186543,-0.707106781186552,0.));
#33162=DIRECTION('ref_axis',(0.707106781186552,0.707106781186543,0.));
#33163=DIRECTION('',(-0.707106781186552,-0.707106781186543,0.));
#33164=DIRECTION('',(0.,0.,-1.));
#33165=DIRECTION('center_axis',(0.,0.,-1.));
#33166=DIRECTION('ref_axis',(-1.,0.,0.));
#33167=DIRECTION('center_axis',(0.,0.,1.));
#33168=DIRECTION('ref_axis',(1.,0.,0.));
#33169=DIRECTION('',(0.,0.,-1.));
#33170=DIRECTION('center_axis',(1.,0.,0.));
#33171=DIRECTION('ref_axis',(0.,0.,-1.));
#33172=DIRECTION('',(0.,-1.,0.));
#33173=DIRECTION('',(0.,0.,-1.));
#33174=DIRECTION('center_axis',(0.,0.,-1.));
#33175=DIRECTION('ref_axis',(-1.,0.,0.));
#33176=DIRECTION('center_axis',(0.,0.,1.));
#33177=DIRECTION('ref_axis',(1.,0.,0.));
#33178=DIRECTION('',(0.,0.,-1.));
#33179=DIRECTION('center_axis',(0.707106781186549,0.707106781186546,0.));
#33180=DIRECTION('ref_axis',(-0.707106781186546,0.707106781186549,0.));
#33181=DIRECTION('',(0.707106781186546,-0.707106781186549,0.));
#33182=DIRECTION('center_axis',(-1.19636101791504E-15,1.,-1.04815936541451E-31));
#33183=DIRECTION('ref_axis',(-1.,-1.19636101791504E-15,0.));
#33184=DIRECTION('',(1.,1.19636101791504E-15,3.7386281809845E-17));
#33185=DIRECTION('',(-4.38061483832527E-16,-6.28895619248706E-31,-1.));
#33186=DIRECTION('',(-1.,-1.19636101791504E-15,0.));
#33187=DIRECTION('',(-8.76122967665054E-17,0.,1.));
#33188=DIRECTION('center_axis',(0.707106781186554,0.707106781186541,-3.09756245794624E-16));
#33189=DIRECTION('ref_axis',(4.38061483832527E-16,6.55212072256257E-31,
1.));
#33190=DIRECTION('',(-0.707106781186541,0.707106781186554,-2.64360933910924E-17));
#33191=DIRECTION('',(-4.38061483832527E-16,0.,-1.));
#33192=DIRECTION('',(0.707106781186541,-0.707106781186554,0.));
#33193=DIRECTION('center_axis',(0.,-1.,0.));
#33194=DIRECTION('ref_axis',(0.,0.,-1.));
#33195=DIRECTION('',(-1.,0.,0.));
#33196=DIRECTION('',(0.,0.,1.));
#33197=DIRECTION('',(1.,0.,0.));
#33198=DIRECTION('center_axis',(-0.707106781186533,-0.707106781186562,0.));
#33199=DIRECTION('ref_axis',(0.707106781186562,-0.707106781186533,0.));
#33200=DIRECTION('',(-0.707106781186562,0.707106781186533,0.));
#33201=DIRECTION('',(0.,0.,1.));
#33202=DIRECTION('',(0.707106781186562,-0.707106781186533,0.));
#33203=DIRECTION('center_axis',(-1.,1.26161707343768E-16,0.));
#33204=DIRECTION('ref_axis',(-1.26161707343768E-16,-1.,0.));
#33205=DIRECTION('',(1.26161707343768E-16,1.,0.));
#33206=DIRECTION('',(0.,0.,1.));
#33207=DIRECTION('',(-1.26161707343768E-16,-1.,0.));
#33208=DIRECTION('center_axis',(1.,1.26161707343768E-16,0.));
#33209=DIRECTION('ref_axis',(-1.26161707343768E-16,1.,0.));
#33210=DIRECTION('',(1.26161707343768E-16,-1.,0.));
#33211=DIRECTION('',(0.,0.,1.));
#33212=DIRECTION('',(-1.26161707343768E-16,1.,0.));
#33213=DIRECTION('',(0.,0.,1.));
#33214=DIRECTION('center_axis',(0.707106781186533,-0.707106781186562,0.));
#33215=DIRECTION('ref_axis',(0.707106781186562,0.707106781186533,0.));
#33216=DIRECTION('',(-0.707106781186562,-0.707106781186533,0.));
#33217=DIRECTION('',(0.,0.,1.));
#33218=DIRECTION('',(0.707106781186562,0.707106781186533,0.));
#33219=DIRECTION('center_axis',(0.,-1.,0.));
#33220=DIRECTION('ref_axis',(0.,0.,-1.));
#33221=DIRECTION('',(-1.,0.,0.));
#33222=DIRECTION('',(-8.76122967665054E-17,0.,1.));
#33223=DIRECTION('',(1.,0.,0.));
#33224=DIRECTION('center_axis',(-0.707106781186554,0.707106781186542,-6.19512491589247E-17));
#33225=DIRECTION('ref_axis',(8.76122967665054E-17,3.85000586821995E-33,
-1.));
#33226=DIRECTION('',(0.707106781186541,0.707106781186554,0.));
#33227=DIRECTION('',(-0.707106781186541,-0.707106781186554,-2.64360933910925E-17));
#33228=DIRECTION('center_axis',(1.,0.,0.));
#33229=DIRECTION('ref_axis',(0.,0.,-1.));
#33230=DIRECTION('',(0.,1.,0.));
#33231=DIRECTION('',(0.,0.,-1.));
#33232=DIRECTION('',(0.,1.,0.));
#33233=DIRECTION('',(0.,0.,1.));
#33234=DIRECTION('center_axis',(0.70710678118655,0.707106781186545,0.));
#33235=DIRECTION('ref_axis',(-0.707106781186545,0.70710678118655,0.));
#33236=DIRECTION('',(-0.707106781186545,0.70710678118655,0.));
#33237=DIRECTION('',(0.,0.,1.));
#33238=DIRECTION('',(-0.707106781186545,0.70710678118655,0.));
#33239=DIRECTION('center_axis',(0.,1.,0.));
#33240=DIRECTION('ref_axis',(0.,0.,1.));
#33241=DIRECTION('',(0.,0.,1.));
#33242=DIRECTION('',(-1.,0.,0.));
#33243=DIRECTION('',(-1.,0.,0.));
#33244=DIRECTION('center_axis',(0.707106781186549,-0.707106781186546,0.));
#33245=DIRECTION('ref_axis',(0.707106781186546,0.707106781186549,0.));
#33246=DIRECTION('',(0.,0.,1.));
#33247=DIRECTION('',(0.707106781186546,0.707106781186549,0.));
#33248=DIRECTION('',(0.707106781186546,0.707106781186549,0.));
#33249=DIRECTION('center_axis',(-1.62579519772897E-16,-1.,0.));
#33250=DIRECTION('ref_axis',(1.,-1.62579519772897E-16,0.));
#33251=DIRECTION('',(0.,0.,1.));
#33252=DIRECTION('',(1.,-1.62579519772897E-16,0.));
#33253=DIRECTION('',(1.,-1.62579519772897E-16,0.));
#33254=DIRECTION('center_axis',(-0.707106781186544,-0.707106781186551,0.));
#33255=DIRECTION('ref_axis',(0.707106781186551,-0.707106781186544,0.));
#33256=DIRECTION('',(0.,0.,1.));
#33257=DIRECTION('',(0.707106781186551,-0.707106781186544,0.));
#33258=DIRECTION('',(0.707106781186551,-0.707106781186544,0.));
#33259=DIRECTION('center_axis',(0.,1.,0.));
#33260=DIRECTION('ref_axis',(0.,0.,1.));
#33261=DIRECTION('',(-1.,0.,0.));
#33262=DIRECTION('',(0.,0.,1.));
#33263=DIRECTION('',(-1.,0.,0.));
#33264=DIRECTION('center_axis',(0.707106781186544,-0.707106781186551,0.));
#33265=DIRECTION('ref_axis',(0.707106781186551,0.707106781186544,0.));
#33266=DIRECTION('',(0.,0.,1.));
#33267=DIRECTION('',(0.707106781186551,0.707106781186544,0.));
#33268=DIRECTION('',(0.707106781186551,0.707106781186544,0.));
#33269=DIRECTION('center_axis',(1.62579519772897E-16,-1.,0.));
#33270=DIRECTION('ref_axis',(1.,1.62579519772897E-16,0.));
#33271=DIRECTION('',(0.,0.,1.));
#33272=DIRECTION('',(1.,1.62579519772897E-16,0.));
#33273=DIRECTION('',(1.,1.62579519772897E-16,0.));
#33274=DIRECTION('center_axis',(-0.707106781186549,-0.707106781186546,0.));
#33275=DIRECTION('ref_axis',(0.707106781186546,-0.707106781186549,0.));
#33276=DIRECTION('',(0.,0.,1.));
#33277=DIRECTION('',(0.707106781186546,-0.707106781186549,0.));
#33278=DIRECTION('',(0.707106781186546,-0.707106781186549,0.));
#33279=DIRECTION('center_axis',(0.,1.,0.));
#33280=DIRECTION('ref_axis',(0.,0.,1.));
#33281=DIRECTION('',(-1.,0.,0.));
#33282=DIRECTION('',(0.,0.,1.));
#33283=DIRECTION('',(-1.,0.,0.));
#33284=DIRECTION('center_axis',(-0.70710678118655,0.707106781186545,0.));
#33285=DIRECTION('ref_axis',(-0.707106781186545,-0.70710678118655,0.));
#33286=DIRECTION('',(-0.707106781186545,-0.70710678118655,0.));
#33287=DIRECTION('',(0.,0.,1.));
#33288=DIRECTION('',(-0.707106781186545,-0.70710678118655,0.));
#33289=DIRECTION('center_axis',(-1.,0.,0.));
#33290=DIRECTION('ref_axis',(0.,0.,1.));
#33291=DIRECTION('',(0.,-1.,0.));
#33292=DIRECTION('',(0.,0.,1.));
#33293=DIRECTION('',(0.,-1.,0.));
#33294=DIRECTION('center_axis',(-0.707106781186546,-0.707106781186549,0.));
#33295=DIRECTION('ref_axis',(0.707106781186549,-0.707106781186546,0.));
#33296=DIRECTION('',(0.707106781186549,-0.707106781186546,0.));
#33297=DIRECTION('',(0.,0.,1.));
#33298=DIRECTION('',(0.707106781186549,-0.707106781186546,0.));
#33299=DIRECTION('center_axis',(-1.,0.,0.));
#33300=DIRECTION('ref_axis',(0.,0.,1.));
#33301=DIRECTION('',(0.,-1.,0.));
#33302=DIRECTION('',(0.,0.,1.));
#33303=DIRECTION('',(0.,-1.,0.));
#33304=DIRECTION('center_axis',(1.2823896663807E-16,1.,0.));
#33305=DIRECTION('ref_axis',(-1.,1.2823896663807E-16,0.));
#33306=DIRECTION('center_axis',(-1.2823896663807E-16,-1.,0.));
#33307=DIRECTION('ref_axis',(-1.,1.2823896663807E-16,2.52323414687535E-15));
#33308=DIRECTION('',(1.,-1.2823896663807E-16,0.));
#33309=DIRECTION('',(0.,0.,-1.));
#33310=DIRECTION('center_axis',(1.,-2.04085114820801E-16,0.));
#33311=DIRECTION('ref_axis',(2.04085114820801E-16,1.,0.));
#33312=DIRECTION('',(0.,0.,1.));
#33313=DIRECTION('',(0.,1.,0.));
#33314=DIRECTION('',(-2.04085114820801E-16,-1.,0.));
#33315=DIRECTION('center_axis',(-0.965925826289069,-0.258819045102518,0.));
#33316=DIRECTION('ref_axis',(0.258819045102518,-0.965925826289069,0.));
#33317=DIRECTION('center_axis',(-0.965925826289069,-0.258819045102518,0.));
#33318=DIRECTION('ref_axis',(0.258819045102518,-0.965925826289069,0.));
#33319=DIRECTION('',(0.258819045102518,-0.965925826289069,0.));
#33320=DIRECTION('',(0.,0.,1.));
#33321=DIRECTION('center_axis',(0.965925826289069,-0.258819045102518,0.));
#33322=DIRECTION('ref_axis',(0.258819045102518,0.965925826289069,0.));
#33323=DIRECTION('center_axis',(0.965925826289069,-0.258819045102518,0.));
#33324=DIRECTION('ref_axis',(0.258819045102518,0.965925826289069,0.));
#33325=DIRECTION('',(0.258819045102518,0.965925826289069,0.));
#33326=DIRECTION('',(0.,0.,-1.));
#33327=DIRECTION('center_axis',(-1.,-2.04085114820801E-16,0.));
#33328=DIRECTION('ref_axis',(2.04085114820801E-16,-1.,0.));
#33329=DIRECTION('',(0.,0.,-1.));
#33330=DIRECTION('',(0.,-1.,0.));
#33331=DIRECTION('',(-2.04085114820801E-16,1.,0.));
#33332=DIRECTION('center_axis',(-1.2823896663807E-16,1.,0.));
#33333=DIRECTION('ref_axis',(-1.,-1.2823896663807E-16,0.));
#33334=DIRECTION('',(1.,1.2823896663807E-16,0.));
#33335=DIRECTION('center_axis',(-1.2823896663807E-16,-1.,0.));
#33336=DIRECTION('ref_axis',(-1.,1.2823896663807E-16,-2.52323414687536E-15));
#33337=DIRECTION('center_axis',(-0.61566147532566,-0.788010753606721,0.));
#33338=DIRECTION('ref_axis',(0.78801075360672,-0.61566147532566,0.));
#33339=DIRECTION('center_axis',(-0.615661475325663,-0.788010753606718,3.86575390646386E-15));
#33340=DIRECTION('ref_axis',(0.788010753606718,-0.615661475325663,-6.5758767605984E-13));
#33341=DIRECTION('',(0.78801075360672,-0.61566147532566,0.));
#33342=DIRECTION('',(0.,0.,1.));
#33343=DIRECTION('center_axis',(0.707106781186548,0.707106781186547,0.));
#33344=DIRECTION('ref_axis',(-0.707106781186547,0.707106781186548,0.));
#33345=DIRECTION('',(0.707106781186547,-0.707106781186548,0.));
#33346=DIRECTION('',(-0.707106781186547,0.707106781186548,0.));
#33347=DIRECTION('',(0.,0.,1.));
#33348=DIRECTION('center_axis',(-0.707106781186548,0.707106781186547,0.));
#33349=DIRECTION('ref_axis',(-0.707106781186547,-0.707106781186548,0.));
#33350=DIRECTION('',(0.707106781186547,0.707106781186548,0.));
#33351=DIRECTION('',(0.,0.,1.));
#33352=DIRECTION('',(-0.707106781186547,-0.707106781186548,0.));
#33353=DIRECTION('center_axis',(0.,0.,1.));
#33354=DIRECTION('ref_axis',(1.,0.,0.));
#33355=DIRECTION('',(1.,0.,0.));
#33356=DIRECTION('',(1.,-4.33680868994201E-15,0.));
#33357=DIRECTION('',(0.78801075360672,0.61566147532566,0.));
#33358=DIRECTION('center_axis',(0.61566147532566,-0.788010753606721,0.));
#33359=DIRECTION('ref_axis',(0.78801075360672,0.61566147532566,0.));
#33360=DIRECTION('center_axis',(0.615661475325666,-0.788010753606716,-4.56861825309369E-15));
#33361=DIRECTION('ref_axis',(0.788010753606716,0.615661475325665,-3.955354877202E-13));
#33362=DIRECTION('',(0.,0.,1.));
#33363=DIRECTION('center_axis',(3.7386281809845E-17,4.26676715361993E-32,
-1.));
#33364=DIRECTION('ref_axis',(-1.,4.36567830323557E-65,-3.7386281809845E-17));
#33365=DIRECTION('',(1.,0.,0.));
#33366=DIRECTION('',(0.707106781186546,0.707106781186549,0.));
#33367=DIRECTION('center_axis',(0.,0.,1.));
#33368=DIRECTION('ref_axis',(1.,0.,0.));
#33369=DIRECTION('',(0.,1.,0.));
#33370=DIRECTION('center_axis',(0.,0.,1.));
#33371=DIRECTION('ref_axis',(1.,0.,0.));
#33372=DIRECTION('',(-0.707106781186549,0.707106781186546,0.));
#33373=DIRECTION('center_axis',(0.,0.,-1.));
#33374=DIRECTION('ref_axis',(1.,0.,0.));
#33375=DIRECTION('center_axis',(0.,0.,1.));
#33376=DIRECTION('ref_axis',(1.,0.,0.));
#33377=DIRECTION('center_axis',(0.,0.,-1.));
#33378=DIRECTION('ref_axis',(1.,0.,0.));
#33379=DIRECTION('',(-0.707106781186548,0.707106781186547,0.));
#33380=DIRECTION('center_axis',(0.,0.,-1.));
#33381=DIRECTION('ref_axis',(1.,0.,0.));
#33382=DIRECTION('',(0.,1.,0.));
#33383=DIRECTION('center_axis',(0.,0.,-1.));
#33384=DIRECTION('ref_axis',(1.,0.,0.));
#33385=DIRECTION('',(0.707106781186545,0.70710678118655,0.));
#33386=DIRECTION('center_axis',(0.,0.,-1.));
#33387=DIRECTION('ref_axis',(1.,0.,0.));
#33388=DIRECTION('center_axis',(0.,0.,1.));
#33389=DIRECTION('ref_axis',(1.,0.,0.));
#33390=DIRECTION('center_axis',(0.,0.,-1.));
#33391=DIRECTION('ref_axis',(1.,0.,0.));
#33392=DIRECTION('',(0.707106781186546,0.707106781186549,0.));
#33393=DIRECTION('',(1.,1.22464679914735E-16,0.));
#33394=DIRECTION('',(0.707106781186546,-0.707106781186549,0.));
#33395=DIRECTION('center_axis',(0.,0.,-1.));
#33396=DIRECTION('ref_axis',(1.,0.,0.));
#33397=DIRECTION('center_axis',(0.,0.,1.));
#33398=DIRECTION('ref_axis',(1.,0.,0.));
#33399=DIRECTION('center_axis',(0.,0.,-1.));
#33400=DIRECTION('ref_axis',(1.,0.,0.));
#33401=DIRECTION('',(0.707106781186545,-0.70710678118655,0.));
#33402=DIRECTION('center_axis',(0.,0.,-1.));
#33403=DIRECTION('ref_axis',(1.,0.,0.));
#33404=DIRECTION('',(0.,-1.,0.));
#33405=DIRECTION('center_axis',(0.,0.,-1.));
#33406=DIRECTION('ref_axis',(1.,0.,0.));
#33407=DIRECTION('',(-0.707106781186548,-0.707106781186547,0.));
#33408=DIRECTION('center_axis',(0.,0.,-1.));
#33409=DIRECTION('ref_axis',(1.,0.,0.));
#33410=DIRECTION('center_axis',(0.,0.,1.));
#33411=DIRECTION('ref_axis',(1.,0.,0.));
#33412=DIRECTION('center_axis',(0.,0.,-1.));
#33413=DIRECTION('ref_axis',(1.,0.,0.));
#33414=DIRECTION('',(-0.707106781186549,-0.707106781186546,0.));
#33415=DIRECTION('center_axis',(0.,0.,1.));
#33416=DIRECTION('ref_axis',(1.,0.,0.));
#33417=DIRECTION('',(0.,-1.,0.));
#33418=DIRECTION('center_axis',(0.,0.,1.));
#33419=DIRECTION('ref_axis',(1.,0.,0.));
#33420=DIRECTION('',(0.707106781186546,-0.707106781186549,0.));
#33421=DIRECTION('',(1.,-3.50803534070133E-16,0.));
#33422=DIRECTION('center_axis',(0.,0.,-1.));
#33423=DIRECTION('ref_axis',(-1.,0.,0.));
#33424=DIRECTION('',(1.,-4.33680868994201E-15,0.));
#33425=DIRECTION('',(-0.707106781186547,-0.707106781186548,0.));
#33426=DIRECTION('',(-1.26161707343768E-16,-1.,0.));
#33427=DIRECTION('',(0.707106781186562,-0.707106781186533,0.));
#33428=DIRECTION('',(1.,0.,0.));
#33429=DIRECTION('',(-0.707106781186548,0.707106781186547,0.));
#33430=DIRECTION('',(1.,1.19636101791504E-15,0.));
#33431=DIRECTION('',(-0.707106781186541,-0.707106781186554,0.));
#33432=DIRECTION('',(1.,0.,0.));
#33433=DIRECTION('',(0.707106781186562,0.707106781186533,0.));
#33434=DIRECTION('',(-1.26161707343768E-16,1.,0.));
#33435=DIRECTION('',(-0.707106781186547,0.707106781186548,0.));
#33436=DIRECTION('',(1.,0.,0.));
#33437=DIRECTION('center_axis',(-0.707106781186554,0.707106781186542,1.85853747476774E-16));
#33438=DIRECTION('ref_axis',(-2.62836890299516E-16,1.6519124519235E-33,
-1.));
#33439=DIRECTION('',(0.707106781186541,0.707106781186554,0.));
#33440=DIRECTION('',(2.62836890299516E-16,0.,1.));
#33441=DIRECTION('',(2.62836890299516E-16,0.,1.));
#33442=DIRECTION('center_axis',(-0.707106781186533,-0.707106781186562,0.));
#33443=DIRECTION('ref_axis',(0.707106781186562,-0.707106781186533,0.));
#33444=DIRECTION('',(-0.707106781186562,0.707106781186533,0.));
#33445=DIRECTION('',(0.,0.,1.));
#33446=DIRECTION('',(0.,0.,1.));
#33447=DIRECTION('center_axis',(-1.,1.26161707343768E-16,0.));
#33448=DIRECTION('ref_axis',(-1.26161707343768E-16,-1.,0.));
#33449=DIRECTION('',(1.26161707343768E-16,1.,0.));
#33450=DIRECTION('',(0.,0.,1.));
#33451=DIRECTION('center_axis',(-0.707106781186548,0.707106781186547,0.));
#33452=DIRECTION('ref_axis',(-0.707106781186547,-0.707106781186548,0.));
#33453=DIRECTION('',(0.707106781186547,0.707106781186548,0.));
#33454=DIRECTION('',(0.,0.,1.));
#33455=DIRECTION('center_axis',(0.,-1.,0.));
#33456=DIRECTION('ref_axis',(0.,0.,-1.));
#33457=DIRECTION('',(-1.,0.,0.));
#33458=DIRECTION('',(2.62836890299516E-16,0.,-1.));
#33459=DIRECTION('center_axis',(0.,0.,1.));
#33460=DIRECTION('ref_axis',(1.,0.,0.));
#33461=DIRECTION('',(0.,0.,1.));
#33462=DIRECTION('center_axis',(0.,0.,1.));
#33463=DIRECTION('ref_axis',(1.,0.,0.));
#33464=DIRECTION('',(0.,0.,-1.));
#33465=DIRECTION('center_axis',(0.,0.,1.));
#33466=DIRECTION('ref_axis',(1.,0.,0.));
#33467=DIRECTION('',(0.,0.,1.));
#33468=DIRECTION('center_axis',(0.,0.,1.));
#33469=DIRECTION('ref_axis',(1.,0.,0.));
#33470=DIRECTION('',(0.,0.,-1.));
#33471=DIRECTION('center_axis',(-1.,0.,0.));
#33472=DIRECTION('ref_axis',(0.,0.,1.));
#33473=DIRECTION('',(0.,-1.,0.));
#33474=DIRECTION('center_axis',(-0.707106781186549,-0.707106781186546,0.));
#33475=DIRECTION('ref_axis',(0.707106781186546,-0.707106781186549,0.));
#33476=DIRECTION('',(0.707106781186546,-0.707106781186549,0.));
#33477=DIRECTION('',(0.,0.,1.));
#33478=DIRECTION('center_axis',(-6.49101394191508E-16,-1.,0.));
#33479=DIRECTION('ref_axis',(1.,-6.49101394191508E-16,0.));
#33480=DIRECTION('',(1.,-3.50803534070133E-16,0.));
#33481=DIRECTION('center_axis',(0.,0.,1.));
#33482=DIRECTION('ref_axis',(1.,0.,0.));
#33483=DIRECTION('center_axis',(0.,0.,-1.));
#33484=DIRECTION('ref_axis',(1.,0.,0.));
#33485=DIRECTION('',(0.,0.,-1.));
#33486=DIRECTION('',(0.,0.,1.));
#33487=DIRECTION('center_axis',(0.,0.,1.));
#33488=DIRECTION('ref_axis',(1.,0.,0.));
#33489=DIRECTION('center_axis',(0.,0.,-1.));
#33490=DIRECTION('ref_axis',(1.,0.,0.));
#33491=DIRECTION('',(0.,0.,-1.));
#33492=DIRECTION('',(0.,0.,1.));
#33493=DIRECTION('center_axis',(0.,0.,1.));
#33494=DIRECTION('ref_axis',(1.,0.,0.));
#33495=DIRECTION('center_axis',(0.,0.,1.));
#33496=DIRECTION('ref_axis',(1.,0.,0.));
#33497=DIRECTION('center_axis',(0.,0.,-1.));
#33498=DIRECTION('ref_axis',(-1.,0.,0.));
#33499=DIRECTION('center_axis',(0.,0.,-1.));
#33500=DIRECTION('ref_axis',(1.,0.,0.));
#33501=DIRECTION('',(0.,0.,-1.));
#33502=DIRECTION('',(0.,0.,1.));
#33503=DIRECTION('center_axis',(0.,0.,-1.));
#33504=DIRECTION('ref_axis',(-1.,0.,0.));
#33505=DIRECTION('center_axis',(0.,0.,-1.));
#33506=DIRECTION('ref_axis',(1.,0.,0.));
#33507=DIRECTION('',(0.,0.,-1.));
#33508=DIRECTION('',(0.,0.,1.));
#33509=DIRECTION('center_axis',(-1.,0.,0.));
#33510=DIRECTION('ref_axis',(0.,0.,1.));
#33511=DIRECTION('',(0.,-1.,0.));
#33512=DIRECTION('center_axis',(-0.707106781186546,0.707106781186549,0.));
#33513=DIRECTION('ref_axis',(-0.707106781186549,-0.707106781186546,0.));
#33514=DIRECTION('',(-0.707106781186548,-0.707106781186547,0.));
#33515=DIRECTION('center_axis',(0.,0.,1.));
#33516=DIRECTION('ref_axis',(1.,0.,0.));
#33517=DIRECTION('center_axis',(0.,0.,-1.));
#33518=DIRECTION('ref_axis',(1.,0.,0.));
#33519=DIRECTION('',(0.,0.,-1.));
#33520=DIRECTION('',(0.,0.,1.));
#33521=DIRECTION('center_axis',(0.,0.,1.));
#33522=DIRECTION('ref_axis',(1.,0.,0.));
#33523=DIRECTION('center_axis',(0.,0.,-1.));
#33524=DIRECTION('ref_axis',(1.,0.,0.));
#33525=DIRECTION('',(0.,0.,-1.));
#33526=DIRECTION('',(0.,0.,1.));
#33527=DIRECTION('center_axis',(0.,0.,1.));
#33528=DIRECTION('ref_axis',(1.,0.,0.));
#33529=DIRECTION('center_axis',(0.,0.,1.));
#33530=DIRECTION('ref_axis',(1.,0.,0.));
#33531=DIRECTION('center_axis',(1.22464679914735E-16,-1.,0.));
#33532=DIRECTION('ref_axis',(1.,1.22464679914735E-16,0.));
#33533=DIRECTION('',(0.,0.,1.));
#33534=DIRECTION('',(1.,1.22464679914735E-16,0.));
#33535=DIRECTION('',(0.,0.,1.));
#33536=DIRECTION('center_axis',(-0.707106781186549,-0.707106781186546,0.));
#33537=DIRECTION('ref_axis',(0.707106781186546,-0.707106781186549,0.));
#33538=DIRECTION('',(0.707106781186546,-0.707106781186549,0.));
#33539=DIRECTION('center_axis',(0.,0.,1.));
#33540=DIRECTION('ref_axis',(1.,0.,0.));
#33541=DIRECTION('center_axis',(0.,0.,-1.));
#33542=DIRECTION('ref_axis',(1.,0.,0.));
#33543=DIRECTION('',(0.,0.,-1.));
#33544=DIRECTION('',(0.,0.,1.));
#33545=DIRECTION('center_axis',(0.,0.,1.));
#33546=DIRECTION('ref_axis',(1.,0.,0.));
#33547=DIRECTION('center_axis',(0.,0.,-1.));
#33548=DIRECTION('ref_axis',(1.,0.,0.));
#33549=DIRECTION('',(0.,0.,-1.));
#33550=DIRECTION('',(0.,0.,1.));
#33551=DIRECTION('center_axis',(0.,0.,1.));
#33552=DIRECTION('ref_axis',(1.,0.,0.));
#33553=DIRECTION('center_axis',(0.,0.,1.));
#33554=DIRECTION('ref_axis',(1.,0.,0.));
#33555=DIRECTION('center_axis',(0.,0.,-1.));
#33556=DIRECTION('ref_axis',(-1.,0.,0.));
#33557=DIRECTION('center_axis',(0.,0.,-1.));
#33558=DIRECTION('ref_axis',(1.,0.,0.));
#33559=DIRECTION('',(0.,0.,-1.));
#33560=DIRECTION('',(0.,0.,1.));
#33561=DIRECTION('center_axis',(0.,0.,-1.));
#33562=DIRECTION('ref_axis',(-1.,0.,0.));
#33563=DIRECTION('center_axis',(0.,0.,-1.));
#33564=DIRECTION('ref_axis',(1.,0.,0.));
#33565=DIRECTION('',(0.,0.,-1.));
#33566=DIRECTION('',(0.,0.,1.));
#33567=DIRECTION('center_axis',(1.,0.,0.));
#33568=DIRECTION('ref_axis',(0.,0.,-1.));
#33569=DIRECTION('',(0.,1.,0.));
#33570=DIRECTION('center_axis',(0.707106781186549,-0.707106781186546,0.));
#33571=DIRECTION('ref_axis',(0.707106781186546,0.707106781186549,0.));
#33572=DIRECTION('',(0.707106781186545,0.70710678118655,0.));
#33573=DIRECTION('center_axis',(0.707106781186549,-0.707106781186546,0.));
#33574=DIRECTION('ref_axis',(0.707106781186546,0.707106781186549,0.));
#33575=DIRECTION('',(0.707106781186546,0.707106781186549,0.));
#33576=DIRECTION('center_axis',(0.,0.,1.));
#33577=DIRECTION('ref_axis',(1.,0.,0.));
#33578=DIRECTION('center_axis',(0.,0.,-1.));
#33579=DIRECTION('ref_axis',(1.,0.,0.));
#33580=DIRECTION('',(0.,0.,-1.));
#33581=DIRECTION('',(0.,0.,1.));
#33582=DIRECTION('center_axis',(0.,0.,1.));
#33583=DIRECTION('ref_axis',(1.,0.,0.));
#33584=DIRECTION('center_axis',(0.,0.,-1.));
#33585=DIRECTION('ref_axis',(1.,0.,0.));
#33586=DIRECTION('',(0.,0.,-1.));
#33587=DIRECTION('',(0.,0.,1.));
#33588=DIRECTION('center_axis',(0.,0.,1.));
#33589=DIRECTION('ref_axis',(1.,0.,0.));
#33590=DIRECTION('center_axis',(0.,0.,1.));
#33591=DIRECTION('ref_axis',(1.,0.,0.));
#33592=DIRECTION('center_axis',(0.,0.,1.));
#33593=DIRECTION('ref_axis',(1.,0.,0.));
#33594=DIRECTION('',(0.,0.,1.));
#33595=DIRECTION('center_axis',(0.,0.,1.));
#33596=DIRECTION('ref_axis',(1.,0.,0.));
#33597=DIRECTION('',(0.,0.,-1.));
#33598=DIRECTION('center_axis',(0.,0.,1.));
#33599=DIRECTION('ref_axis',(1.,0.,0.));
#33600=DIRECTION('',(0.,0.,1.));
#33601=DIRECTION('center_axis',(0.,0.,1.));
#33602=DIRECTION('ref_axis',(1.,0.,0.));
#33603=DIRECTION('',(0.,0.,-1.));
#33604=DIRECTION('center_axis',(0.707106781186548,0.707106781186547,0.));
#33605=DIRECTION('ref_axis',(-0.707106781186547,0.707106781186548,0.));
#33606=DIRECTION('',(0.707106781186547,-0.707106781186548,0.));
#33607=DIRECTION('',(0.,0.,1.));
#33608=DIRECTION('',(0.,0.,1.));
#33609=DIRECTION('center_axis',(1.,1.26161707343768E-16,0.));
#33610=DIRECTION('ref_axis',(-1.26161707343768E-16,1.,0.));
#33611=DIRECTION('',(1.26161707343768E-16,-1.,0.));
#33612=DIRECTION('',(0.,0.,1.));
#33613=DIRECTION('center_axis',(0.707106781186533,-0.707106781186562,0.));
#33614=DIRECTION('ref_axis',(0.707106781186562,0.707106781186533,0.));
#33615=DIRECTION('',(-0.707106781186562,-0.707106781186533,0.));
#33616=DIRECTION('',(0.,0.,1.));
#33617=DIRECTION('center_axis',(0.,-1.,0.));
#33618=DIRECTION('ref_axis',(0.,0.,-1.));
#33619=DIRECTION('',(-1.,0.,0.));
#33620=DIRECTION('center_axis',(0.,-1.,0.));
#33621=DIRECTION('ref_axis',(0.,0.,-1.));
#33622=DIRECTION('',(1.,0.,0.));
#33623=DIRECTION('',(0.,0.,1.));
#33624=DIRECTION('center_axis',(0.707106781186549,-0.707106781186546,0.));
#33625=DIRECTION('ref_axis',(0.707106781186546,0.707106781186549,0.));
#33626=DIRECTION('',(0.707106781186546,0.707106781186549,0.));
#33627=DIRECTION('center_axis',(1.,0.,0.));
#33628=DIRECTION('ref_axis',(0.,0.,-1.));
#33629=DIRECTION('',(0.,1.,0.));
#33630=DIRECTION('center_axis',(0.707106781186546,0.707106781186549,0.));
#33631=DIRECTION('ref_axis',(-0.707106781186549,0.707106781186546,0.));
#33632=DIRECTION('',(-0.707106781186549,0.707106781186546,0.));
#33633=DIRECTION('center_axis',(0.707106781186546,0.707106781186549,0.));
#33634=DIRECTION('ref_axis',(-0.707106781186549,0.707106781186546,0.));
#33635=DIRECTION('',(-0.707106781186548,0.707106781186547,0.));
#33636=DIRECTION('center_axis',(-0.707106781186549,-0.707106781186546,0.));
#33637=DIRECTION('ref_axis',(0.707106781186546,-0.707106781186549,0.));
#33638=DIRECTION('',(0.707106781186545,-0.70710678118655,0.));
#33639=DIRECTION('center_axis',(-0.707106781186546,0.707106781186549,0.));
#33640=DIRECTION('ref_axis',(-0.707106781186549,-0.707106781186546,0.));
#33641=DIRECTION('',(-0.707106781186549,-0.707106781186546,0.));
#33642=DIRECTION('center_axis',(0.707106781186547,0.707106781186548,1.85853747476773E-16));
#33643=DIRECTION('ref_axis',(-2.62836890299516E-16,-6.09040047468605E-31,
1.));
#33644=DIRECTION('',(0.707106781186548,-0.707106781186547,0.));
#33645=DIRECTION('',(2.62836890299516E-16,6.28895619248706E-31,-1.));
#33646=DIRECTION('center_axis',(-1.19636101791504E-15,1.,3.14447809624353E-31));
#33647=DIRECTION('ref_axis',(-1.,-1.19636101791504E-15,0.));
#33648=DIRECTION('',(-1.,-1.19636101791504E-15,0.));
#33649=DIRECTION('center_axis',(0.,0.,1.));
#33650=DIRECTION('ref_axis',(1.,0.,0.));
#33651=DIRECTION('center_axis',(1.,1.73472347597681E-16,0.));
#33652=DIRECTION('ref_axis',(-1.73472347597681E-16,1.,0.));
#33653=DIRECTION('',(-1.73472347597681E-16,1.,0.));
#33654=DIRECTION('',(0.,0.,1.));
#33655=DIRECTION('center_axis',(0.,0.,1.));
#33656=DIRECTION('ref_axis',(1.,0.,0.));
#33657=DIRECTION('center_axis',(0.,0.,1.));
#33658=DIRECTION('ref_axis',(1.,0.,0.));
#33659=DIRECTION('',(0.,0.,1.));
#33660=DIRECTION('center_axis',(-1.,1.73472347597681E-16,0.));
#33661=DIRECTION('ref_axis',(-1.73472347597681E-16,-1.,0.));
#33662=DIRECTION('',(-1.73472347597681E-16,-1.,0.));
#33663=DIRECTION('center_axis',(0.,0.,1.));
#33664=DIRECTION('ref_axis',(1.,0.,0.));
#33665=DIRECTION('center_axis',(0.,-1.,0.));
#33666=DIRECTION('ref_axis',(0.,0.,-1.));
#33667=DIRECTION('center_axis',(0.,-1.,0.));
#33668=DIRECTION('ref_axis',(0.,0.,-1.));
#33669=DIRECTION('center_axis',(0.,-1.,0.));
#33670=DIRECTION('ref_axis',(0.,0.,-1.));
#33671=DIRECTION('center_axis',(0.,-1.,0.));
#33672=DIRECTION('ref_axis',(0.,0.,-1.));
#33673=DIRECTION('axis',(0.,0.,1.));
#33674=DIRECTION('refdir',(1.,0.,0.));
#33675=DIRECTION('center_axis',(-6.99485272571294E-17,-0.923879532511288,
0.382683432365087));
#33676=DIRECTION('ref_axis',(0.,-0.382683432365087,-0.923879532511288));
#33677=DIRECTION('center_axis',(0.,0.923879532511288,-0.382683432365087));
#33678=DIRECTION('ref_axis',(0.,0.382683432365087,0.923879532511288));
#33679=DIRECTION('center_axis',(1.,-1.77588086089071E-17,1.39910753728411E-16));
#33680=DIRECTION('ref_axis',(-1.22464679914735E-16,0.382683432365087,0.923879532511288));
#33681=DIRECTION('center_axis',(-6.99485272571294E-17,-0.923879532511288,
0.382683432365087));
#33682=DIRECTION('ref_axis',(6.87413134363318E-33,-0.382683432365087,-0.923879532511288));
#33683=DIRECTION('center_axis',(-1.,1.77588086089071E-17,-1.39910753728411E-16));
#33684=DIRECTION('ref_axis',(-1.22464679914735E-16,0.382683432365087,0.923879532511288));
#33685=DIRECTION('center_axis',(-6.99485272571294E-17,-0.923879532511288,
0.382683432365087));
#33686=DIRECTION('ref_axis',(1.30371071656723E-32,-0.382683432365087,-0.923879532511288));
#33687=DIRECTION('center_axis',(-6.99485272571294E-17,-0.923879532511288,
0.382683432365087));
#33688=DIRECTION('ref_axis',(7.11155521594025E-34,-0.382683432365087,-0.923879532511288));
#33689=DIRECTION('',(1.0961176199419E-16,0.722104291896042,-0.691784208858019));
#33690=DIRECTION('center_axis',(-6.99485272571294E-17,-0.923879532511288,
0.382683432365087));
#33691=DIRECTION('ref_axis',(7.11155521594025E-34,-0.382683432365087,-0.923879532511288));
#33692=DIRECTION('center_axis',(-0.5,-0.33141357403559,-0.800103145191267));
#33693=DIRECTION('ref_axis',(-0.866025403784439,0.191341716182545,0.461939766255643));
#33694=DIRECTION('center_axis',(-6.99485272571294E-17,-0.923879532511288,
0.382683432365087));
#33695=DIRECTION('ref_axis',(-4.26190864642653E-32,-0.382683432365087,-0.923879532511288));
#33696=DIRECTION('center_axis',(0.,-0.923879532511288,0.382683432365087));
#33697=DIRECTION('ref_axis',(0.,-0.382683432365087,-0.923879532511288));
#33698=DIRECTION('center_axis',(0.,-0.923879532511288,0.382683432365087));
#33699=DIRECTION('ref_axis',(0.,-0.382683432365087,-0.923879532511288));
#33700=DIRECTION('center_axis',(0.,0.923879532511288,-0.382683432365087));
#33701=DIRECTION('ref_axis',(0.,0.382683432365087,0.923879532511288));
#33702=DIRECTION('center_axis',(0.,0.923879532511288,-0.382683432365087));
#33703=DIRECTION('ref_axis',(0.,0.382683432365087,0.923879532511288));
#33704=DIRECTION('center_axis',(0.,-0.923879532511288,0.382683432365087));
#33705=DIRECTION('ref_axis',(0.,-0.382683432365087,-0.923879532511288));
#33706=DIRECTION('center_axis',(0.,-0.923879532511288,0.382683432365087));
#33707=DIRECTION('ref_axis',(0.,-0.382683432365087,-0.923879532511288));
#33708=DIRECTION('',(0.,0.923879532511288,-0.382683432365087));
#33709=DIRECTION('center_axis',(0.,-0.923879532511288,0.382683432365087));
#33710=DIRECTION('ref_axis',(0.,-0.382683432365087,-0.923879532511288));
#33711=DIRECTION('center_axis',(0.,0.,-1.));
#33712=DIRECTION('ref_axis',(-1.,0.,0.));
#33713=DIRECTION('center_axis',(0.,0.,-1.));
#33714=DIRECTION('ref_axis',(-1.,0.,0.));
#33715=DIRECTION('center_axis',(0.,0.,-1.));
#33716=DIRECTION('ref_axis',(-1.,0.,0.));
#33717=DIRECTION('center_axis',(0.,0.,-1.));
#33718=DIRECTION('ref_axis',(-1.,0.,0.));
#33719=DIRECTION('',(0.,0.,1.));
#33720=DIRECTION('center_axis',(0.,0.,-1.));
#33721=DIRECTION('ref_axis',(-1.,0.,0.));
#33722=DIRECTION('center_axis',(0.,0.,-1.));
#33723=DIRECTION('ref_axis',(-1.,0.,0.));
#33724=DIRECTION('center_axis',(0.,0.,-1.));
#33725=DIRECTION('ref_axis',(-1.,0.,0.));
#33726=DIRECTION('center_axis',(0.,0.,-1.));
#33727=DIRECTION('ref_axis',(-1.,0.,0.));
#33728=DIRECTION('center_axis',(0.,0.,-1.));
#33729=DIRECTION('ref_axis',(-1.,0.,0.));
#33730=DIRECTION('center_axis',(0.,0.,-1.));
#33731=DIRECTION('ref_axis',(-1.,0.,0.));
#33732=DIRECTION('center_axis',(6.12323399573677E-17,0.,1.));
#33733=DIRECTION('ref_axis',(1.,0.,0.));
#33734=DIRECTION('center_axis',(1.22464679914735E-16,-1.,0.));
#33735=DIRECTION('ref_axis',(-1.,-1.22464679914735E-16,0.));
#33736=DIRECTION('center_axis',(0.,-0.923879532511288,0.382683432365087));
#33737=DIRECTION('ref_axis',(0.,-0.382683432365087,-0.923879532511288));
#33738=DIRECTION('center_axis',(0.,-0.923879532511288,0.382683432365087));
#33739=DIRECTION('ref_axis',(0.,-0.382683432365087,-0.923879532511288));
#33740=DIRECTION('center_axis',(0.,-0.923879532511288,0.382683432365087));
#33741=DIRECTION('ref_axis',(0.,-0.382683432365087,-0.923879532511288));
#33742=DIRECTION('center_axis',(0.,-0.923879532511288,0.382683432365087));
#33743=DIRECTION('ref_axis',(0.,-0.382683432365087,-0.923879532511288));
#33744=DIRECTION('center_axis',(0.,-0.923879532511288,0.382683432365087));
#33745=DIRECTION('ref_axis',(0.,-0.382683432365087,-0.923879532511288));
#33746=DIRECTION('center_axis',(0.,-0.923879532511288,0.382683432365087));
#33747=DIRECTION('ref_axis',(0.,-0.382683432365087,-0.923879532511288));
#33748=DIRECTION('center_axis',(0.,0.923879532511288,-0.382683432365087));
#33749=DIRECTION('ref_axis',(0.,0.382683432365087,0.923879532511288));
#33750=DIRECTION('center_axis',(0.,0.923879532511288,-0.382683432365087));
#33751=DIRECTION('ref_axis',(0.,0.382683432365087,0.923879532511288));
#33752=DIRECTION('center_axis',(0.,0.923879532511288,-0.382683432365087));
#33753=DIRECTION('ref_axis',(0.,0.382683432365087,0.923879532511288));
#33754=DIRECTION('center_axis',(0.,0.923879532511288,-0.382683432365087));
#33755=DIRECTION('ref_axis',(0.,0.382683432365087,0.923879532511288));
#33756=DIRECTION('center_axis',(0.,0.923879532511288,-0.382683432365087));
#33757=DIRECTION('ref_axis',(0.,0.382683432365087,0.923879532511288));
#33758=DIRECTION('center_axis',(0.,-0.923879532511288,0.382683432365087));
#33759=DIRECTION('ref_axis',(0.,-0.382683432365087,-0.923879532511288));
#33760=DIRECTION('center_axis',(0.,0.,1.));
#33761=DIRECTION('ref_axis',(1.,0.,0.));
#33762=DIRECTION('',(3.56799717200074E-15,-1.,0.));
#33763=DIRECTION('',(-0.866025403784438,-0.500000000000001,0.));
#33764=DIRECTION('center_axis',(0.,0.,1.));
#33765=DIRECTION('ref_axis',(1.,0.,0.));
#33766=DIRECTION('',(-0.866025403784438,-0.500000000000001,0.));
#33767=DIRECTION('',(-0.866025403784441,0.499999999999995,0.));
#33768=DIRECTION('center_axis',(0.,0.,1.));
#33769=DIRECTION('ref_axis',(1.,0.,0.));
#33770=DIRECTION('',(-0.866025403784441,0.499999999999995,0.));
#33771=DIRECTION('',(-1.05162021911601E-14,1.,0.));
#33772=DIRECTION('center_axis',(0.,0.,1.));
#33773=DIRECTION('ref_axis',(1.,0.,0.));
#33774=DIRECTION('',(-1.05162021911601E-14,1.,0.));
#33775=DIRECTION('',(0.866025403784434,0.500000000000007,0.));
#33776=DIRECTION('center_axis',(0.,0.,1.));
#33777=DIRECTION('ref_axis',(1.,0.,0.));
#33778=DIRECTION('',(0.866025403784434,0.500000000000007,0.));
#33779=DIRECTION('',(0.866025403784441,-0.499999999999995,0.));
#33780=DIRECTION('center_axis',(0.,0.,1.));
#33781=DIRECTION('ref_axis',(1.,0.,0.));
#33782=DIRECTION('',(0.866025403784441,-0.499999999999995,0.));
#33783=DIRECTION('',(3.56799717200074E-15,-1.,0.));
#33784=DIRECTION('center_axis',(0.499999999999995,0.866025403784442,0.));
#33785=DIRECTION('ref_axis',(-0.866025403784441,0.499999999999995,0.));
#33786=DIRECTION('',(-0.866025403784441,0.499999999999995,0.));
#33787=DIRECTION('',(0.,0.,1.));
#33788=DIRECTION('',(0.,0.,1.));
#33789=DIRECTION('center_axis',(1.,1.05162021911601E-14,0.));
#33790=DIRECTION('ref_axis',(-1.05162021911601E-14,1.,0.));
#33791=DIRECTION('',(-1.05162021911601E-14,1.,0.));
#33792=DIRECTION('',(0.,0.,1.));
#33793=DIRECTION('center_axis',(0.500000000000007,-0.866025403784435,0.));
#33794=DIRECTION('ref_axis',(0.866025403784435,0.500000000000007,0.));
#33795=DIRECTION('',(0.866025403784434,0.500000000000007,0.));
#33796=DIRECTION('',(0.,0.,1.));
#33797=DIRECTION('center_axis',(-0.499999999999995,-0.866025403784441,0.));
#33798=DIRECTION('ref_axis',(0.866025403784442,-0.499999999999995,0.));
#33799=DIRECTION('',(0.866025403784441,-0.499999999999995,0.));
#33800=DIRECTION('',(0.,0.,1.));
#33801=DIRECTION('center_axis',(-1.,-3.56799717200074E-15,0.));
#33802=DIRECTION('ref_axis',(3.56799717200074E-15,-1.,0.));
#33803=DIRECTION('',(3.56799717200074E-15,-1.,0.));
#33804=DIRECTION('',(0.,0.,1.));
#33805=DIRECTION('center_axis',(-0.500000000000001,0.866025403784438,0.));
#33806=DIRECTION('ref_axis',(-0.866025403784438,-0.500000000000001,0.));
#33807=DIRECTION('',(-0.866025403784438,-0.500000000000001,0.));
#33808=DIRECTION('center_axis',(0.,0.,1.));
#33809=DIRECTION('ref_axis',(1.,0.,0.));
#33810=DIRECTION('center_axis',(0.,0.923879532511288,-0.382683432365087));
#33811=DIRECTION('ref_axis',(0.,0.382683432365087,0.923879532511288));
#33812=DIRECTION('center_axis',(0.,0.923879532511288,-0.382683432365087));
#33813=DIRECTION('ref_axis',(0.,0.382683432365087,0.923879532511288));
#33814=DIRECTION('center_axis',(0.,0.923879532511288,-0.382683432365087));
#33815=DIRECTION('ref_axis',(1.22464679914735E-16,-0.382683432365087,-0.923879532511288));
#33816=DIRECTION('center_axis',(0.,0.923879532511288,-0.382683432365087));
#33817=DIRECTION('ref_axis',(0.,0.382683432365087,0.923879532511288));
#33818=DIRECTION('center_axis',(0.,0.923879532511288,-0.382683432365087));
#33819=DIRECTION('ref_axis',(0.,0.382683432365087,0.923879532511288));
#33820=DIRECTION('center_axis',(0.,-0.923879532511288,0.382683432365087));
#33821=DIRECTION('ref_axis',(0.,-0.382683432365087,-0.923879532511288));
#33822=DIRECTION('center_axis',(0.,-0.923879532511288,0.382683432365087));
#33823=DIRECTION('ref_axis',(0.,-0.382683432365087,-0.923879532511288));
#33824=DIRECTION('center_axis',(0.,-0.923879532511288,0.382683432365087));
#33825=DIRECTION('ref_axis',(-7.6571373978539E-16,0.382683432365087,0.923879532511288));
#33826=DIRECTION('center_axis',(0.,-0.923879532511288,0.382683432365087));
#33827=DIRECTION('ref_axis',(0.,-0.382683432365087,-0.923879532511288));
#33828=DIRECTION('center_axis',(0.,-0.923879532511288,0.382683432365087));
#33829=DIRECTION('ref_axis',(0.,-0.382683432365087,-0.923879532511288));
#33830=DIRECTION('center_axis',(-0.5,-0.331413574035589,-0.800103145191266));
#33831=DIRECTION('ref_axis',(-0.84802901144343,6.89411318440465E-18,0.529949804934655));
#33832=DIRECTION('',(0.,0.923879532511288,-0.382683432365087));
#33833=DIRECTION('',(0.,0.923879532511288,-0.382683432365087));
#33834=DIRECTION('center_axis',(-1.,4.14906208744436E-17,1.00167219626363E-16));
#33835=DIRECTION('ref_axis',(1.00167219626363E-16,0.,1.));
#33836=DIRECTION('',(0.,0.923879532511288,-0.382683432365087));
#33837=DIRECTION('center_axis',(-0.5,0.331413574035589,0.800103145191267));
#33838=DIRECTION('ref_axis',(0.848029011443431,-1.03411697766071E-17,0.529949804934654));
#33839=DIRECTION('',(0.,0.923879532511288,-0.382683432365087));
#33840=DIRECTION('center_axis',(0.5,0.331413574035589,0.800103145191267));
#33841=DIRECTION('ref_axis',(0.84802901144343,-3.44705659220234E-18,-0.529949804934655));
#33842=DIRECTION('',(0.,0.923879532511288,-0.382683432365087));
#33843=DIRECTION('center_axis',(1.,0.,0.));
#33844=DIRECTION('ref_axis',(0.,0.,-1.));
#33845=DIRECTION('',(0.,0.923879532511288,-0.382683432365087));
#33846=DIRECTION('center_axis',(0.499999999999999,-0.33141357403559,-0.800103145191267));
#33847=DIRECTION('ref_axis',(-0.848029011443431,5.08102344929861E-18,-0.529949804934654));
#33848=DIRECTION('center_axis',(-6.99485272571294E-17,-0.923879532511288,
0.382683432365087));
#33849=DIRECTION('ref_axis',(-2.37033238942555E-33,-0.382683432365087,-0.923879532511288));
#33850=DIRECTION('',(-6.16297582203915E-33,1.23259516440783E-32,1.));
#33851=DIRECTION('',(1.,2.91351622293183E-31,6.16297582203915E-33));
#33852=DIRECTION('',(-6.16297582203915E-33,1.23259516440783E-32,1.));
#33853=DIRECTION('',(1.,2.91351622293183E-31,6.16297582203915E-33));
#33854=DIRECTION('',(5.91781640741636E-18,9.12120421661795E-31,-1.));
#33855=DIRECTION('',(-1.38777878078333E-17,1.,9.12038295461407E-31));
#33856=DIRECTION('',(-6.16297582203915E-33,1.23259516440783E-32,1.));
#33857=DIRECTION('',(1.,2.91351622293183E-31,6.16297582203915E-33));
#33858=DIRECTION('',(4.16333634234429E-17,-4.16333634234424E-17,-1.));
#33859=DIRECTION('',(-5.5511151231277E-17,1.,-4.16333634234424E-17));
#33860=DIRECTION('',(-6.16297582203915E-33,1.23259516440783E-32,1.));
#33861=DIRECTION('',(1.,2.91351622293183E-31,6.16297582203915E-33));
#33862=DIRECTION('',(-6.16297582203915E-33,1.23259516440783E-32,1.));
#33863=DIRECTION('',(1.,2.91351622293183E-31,6.16297582203915E-33));
#33864=DIRECTION('',(5.91781640741636E-18,9.12120421661795E-31,-1.));
#33865=DIRECTION('',(-1.38777878078331E-17,1.,9.12038295461407E-31));
#33866=DIRECTION('',(-6.16297582203915E-33,1.23259516440783E-32,1.));
#33867=DIRECTION('',(1.,2.91351622293183E-31,6.16297582203915E-33));
#33868=DIRECTION('',(4.16333634234429E-17,-4.16333634234424E-17,-1.));
#33869=DIRECTION('',(-5.5511151231277E-17,1.,-4.16333634234424E-17));
#33870=DIRECTION('axis',(0.,0.,1.));
#33871=DIRECTION('refdir',(1.,0.,0.));
#33872=DIRECTION('center_axis',(0.,-1.,0.));
#33873=DIRECTION('ref_axis',(0.,0.,-1.));
#33874=DIRECTION('center_axis',(0.,-1.,0.));
#33875=DIRECTION('ref_axis',(0.,0.,-1.));
#33876=DIRECTION('',(0.,-1.,0.));
#33877=DIRECTION('center_axis',(0.,-1.,0.));
#33878=DIRECTION('ref_axis',(0.,0.,-1.));
#33879=DIRECTION('center_axis',(0.,-1.,0.));
#33880=DIRECTION('ref_axis',(0.,0.,-1.));
#33881=DIRECTION('',(-1.04972719113862E-16,-0.515038074910054,0.857167300702112));
#33882=DIRECTION('center_axis',(0.,-1.,0.));
#33883=DIRECTION('ref_axis',(0.,0.,-1.));
#33884=DIRECTION('center_axis',(0.,-1.,0.));
#33885=DIRECTION('ref_axis',(0.,0.,-1.));
#33886=DIRECTION('',(0.,-1.,0.));
#33887=DIRECTION('center_axis',(0.,-1.,0.));
#33888=DIRECTION('ref_axis',(0.,0.,-1.));
#33889=DIRECTION('center_axis',(0.,-1.,0.));
#33890=DIRECTION('ref_axis',(0.,0.,-1.));
#33891=DIRECTION('',(-1.04972719113862E-16,-0.515038074910054,0.857167300702112));
#33892=DIRECTION('center_axis',(0.,-1.,0.));
#33893=DIRECTION('ref_axis',(0.,0.,-1.));
#33894=DIRECTION('center_axis',(0.,-1.,0.));
#33895=DIRECTION('ref_axis',(0.,0.,-1.));
#33896=DIRECTION('',(0.,-1.,0.));
#33897=DIRECTION('center_axis',(0.,-1.,0.));
#33898=DIRECTION('ref_axis',(0.,0.,-1.));
#33899=DIRECTION('center_axis',(0.,-1.,0.));
#33900=DIRECTION('ref_axis',(0.,0.,-1.));
#33901=DIRECTION('',(-1.04972719113862E-16,-0.515038074910054,0.857167300702112));
#33902=DIRECTION('center_axis',(0.,-1.,0.));
#33903=DIRECTION('ref_axis',(0.,0.,-1.));
#33904=DIRECTION('center_axis',(0.,-1.,0.));
#33905=DIRECTION('ref_axis',(0.,0.,-1.));
#33906=DIRECTION('',(0.,-1.,0.));
#33907=DIRECTION('center_axis',(0.,-1.,0.));
#33908=DIRECTION('ref_axis',(0.,0.,-1.));
#33909=DIRECTION('center_axis',(0.,-1.,0.));
#33910=DIRECTION('ref_axis',(0.,0.,-1.));
#33911=DIRECTION('',(-1.04972719113862E-16,-0.515038074910056,0.857167300702111));
#33912=DIRECTION('center_axis',(0.,-1.,0.));
#33913=DIRECTION('ref_axis',(0.,0.,-1.));
#33914=DIRECTION('center_axis',(0.,-1.,0.));
#33915=DIRECTION('ref_axis',(0.,0.,-1.));
#33916=DIRECTION('',(0.,-1.,0.));
#33917=DIRECTION('center_axis',(0.,-1.,0.));
#33918=DIRECTION('ref_axis',(0.,0.,-1.));
#33919=DIRECTION('center_axis',(0.,-1.,0.));
#33920=DIRECTION('ref_axis',(0.,0.,-1.));
#33921=DIRECTION('',(-1.04972719113862E-16,-0.515038074910056,0.857167300702111));
#33922=DIRECTION('center_axis',(0.,-1.,0.));
#33923=DIRECTION('ref_axis',(0.,0.,-1.));
#33924=DIRECTION('center_axis',(0.,-1.,0.));
#33925=DIRECTION('ref_axis',(0.,0.,-1.));
#33926=DIRECTION('',(0.,-1.,0.));
#33927=DIRECTION('center_axis',(0.,-1.,0.));
#33928=DIRECTION('ref_axis',(0.,0.,-1.));
#33929=DIRECTION('center_axis',(0.,-1.,0.));
#33930=DIRECTION('ref_axis',(0.,0.,-1.));
#33931=DIRECTION('',(-1.04972719113862E-16,-0.515038074910054,0.857167300702112));
#33932=DIRECTION('center_axis',(0.,-1.,0.));
#33933=DIRECTION('ref_axis',(0.,0.,-1.));
#33934=DIRECTION('center_axis',(0.,-1.,0.));
#33935=DIRECTION('ref_axis',(0.,0.,-1.));
#33936=DIRECTION('',(0.,-1.,0.));
#33937=DIRECTION('center_axis',(0.,-1.,0.));
#33938=DIRECTION('ref_axis',(0.,0.,-1.));
#33939=DIRECTION('center_axis',(0.,-1.,0.));
#33940=DIRECTION('ref_axis',(0.,0.,-1.));
#33941=DIRECTION('',(-1.04972719113862E-16,-0.515038074910054,0.857167300702112));
#33942=DIRECTION('center_axis',(0.,-1.,0.));
#33943=DIRECTION('ref_axis',(0.,0.,-1.));
#33944=DIRECTION('center_axis',(0.,-1.,0.));
#33945=DIRECTION('ref_axis',(0.,0.,-1.));
#33946=DIRECTION('',(0.,-1.,0.));
#33947=DIRECTION('center_axis',(0.,-1.,0.));
#33948=DIRECTION('ref_axis',(0.,0.,-1.));
#33949=DIRECTION('center_axis',(0.,-1.,0.));
#33950=DIRECTION('ref_axis',(0.,0.,-1.));
#33951=DIRECTION('',(-1.04972719113862E-16,-0.515038074910054,0.857167300702112));
#33952=DIRECTION('center_axis',(0.,1.,0.));
#33953=DIRECTION('ref_axis',(0.,0.,1.));
#33954=DIRECTION('',(0.,0.,-1.));
#33955=DIRECTION('',(1.,0.,0.));
#33956=DIRECTION('',(0.,0.,-1.));
#33957=DIRECTION('',(1.,0.,0.));
#33958=DIRECTION('center_axis',(-1.,0.,0.));
#33959=DIRECTION('ref_axis',(0.,0.,1.));
#33960=DIRECTION('',(0.,-1.,0.));
#33961=DIRECTION('center_axis',(-1.,0.,0.));
#33962=DIRECTION('ref_axis',(0.,0.,1.));
#33963=DIRECTION('',(0.,0.,1.));
#33964=DIRECTION('center_axis',(-1.,0.,0.));
#33965=DIRECTION('ref_axis',(0.,0.,1.));
#33966=DIRECTION('',(0.,1.,0.));
#33967=DIRECTION('',(0.,0.,-1.));
#33968=DIRECTION('',(0.,1.,0.));
#33969=DIRECTION('',(0.,0.,-1.));
#33970=DIRECTION('',(0.,1.,0.));
#33971=DIRECTION('center_axis',(0.,-1.,0.));
#33972=DIRECTION('ref_axis',(0.,0.,-1.));
#33973=DIRECTION('',(-1.,0.,0.));
#33974=DIRECTION('',(0.,0.,-1.));
#33975=DIRECTION('',(-1.,0.,0.));
#33976=DIRECTION('center_axis',(1.,0.,0.));
#33977=DIRECTION('ref_axis',(0.,0.,-1.));
#33978=DIRECTION('',(0.,1.,0.));
#33979=DIRECTION('center_axis',(1.,0.,0.));
#33980=DIRECTION('ref_axis',(0.,0.,-1.));
#33981=DIRECTION('',(0.,0.,1.));
#33982=DIRECTION('center_axis',(1.,0.,0.));
#33983=DIRECTION('ref_axis',(0.,0.,-1.));
#33984=DIRECTION('',(0.,-1.,0.));
#33985=DIRECTION('',(0.,-1.,0.));
#33986=DIRECTION('',(0.,-1.,0.));
#33987=DIRECTION('',(0.,0.,-1.));
#33988=DIRECTION('center_axis',(0.,1.,0.));
#33989=DIRECTION('ref_axis',(0.,0.,1.));
#33990=DIRECTION('',(1.,0.,0.));
#33991=DIRECTION('',(1.,0.,0.));
#33992=DIRECTION('center_axis',(0.,0.,1.));
#33993=DIRECTION('ref_axis',(1.,0.,0.));
#33994=DIRECTION('center_axis',(0.,0.,1.));
#33995=DIRECTION('ref_axis',(1.,0.,0.));
#33996=DIRECTION('center_axis',(0.,0.,1.));
#33997=DIRECTION('ref_axis',(1.,0.,0.));
#33998=DIRECTION('',(1.,0.,0.));
#33999=DIRECTION('center_axis',(0.,1.,0.));
#34000=DIRECTION('ref_axis',(0.,0.,1.));
#34001=DIRECTION('',(1.,0.,0.));
#34002=DIRECTION('',(-1.,0.,0.));
#34003=DIRECTION('center_axis',(0.,0.,-1.));
#34004=DIRECTION('ref_axis',(-1.,0.,0.));
#34005=DIRECTION('',(-1.,0.,0.));
#34006=DIRECTION('center_axis',(-1.,0.,0.));
#34007=DIRECTION('ref_axis',(0.,0.,1.));
#34008=DIRECTION('center_axis',(-1.,0.,0.));
#34009=DIRECTION('ref_axis',(0.,0.,1.));
#34010=DIRECTION('axis',(0.,0.,1.));
#34011=DIRECTION('refdir',(1.,0.,0.));
#34012=DIRECTION('center_axis',(1.,0.,0.));
#34013=DIRECTION('ref_axis',(0.,0.,-1.));
#34014=DIRECTION('center_axis',(1.,0.,0.));
#34015=DIRECTION('ref_axis',(0.,0.,-1.));
#34016=DIRECTION('center_axis',(1.,0.,0.));
#34017=DIRECTION('ref_axis',(0.,0.,-1.));
#34018=DIRECTION('',(-0.70710678118655,8.65956056235489E-17,-0.707106781186544));
#34019=DIRECTION('center_axis',(-1.,0.,0.));
#34020=DIRECTION('ref_axis',(0.,0.,-1.));
#34021=DIRECTION('center_axis',(-1.,5.24877093477881E-17,0.));
#34022=DIRECTION('ref_axis',(-5.24877093477881E-17,-1.,0.));
#34023=DIRECTION('',(-0.515038074910058,0.85716730070211,-1.04972719113862E-16));
#34024=DIRECTION('center_axis',(-1.,5.24877093477881E-17,0.));
#34025=DIRECTION('ref_axis',(-5.24877093477881E-17,-1.,0.));
#34026=DIRECTION('center_axis',(-1.,5.24877093477881E-17,0.));
#34027=DIRECTION('ref_axis',(-5.24877093477881E-17,-1.,0.));
#34028=DIRECTION('center_axis',(-1.,5.24877093477881E-17,0.));
#34029=DIRECTION('ref_axis',(-5.24877093477881E-17,-1.,0.));
#34030=DIRECTION('center_axis',(-1.,5.24877093477881E-17,0.));
#34031=DIRECTION('ref_axis',(-5.24877093477881E-17,-1.,0.));
#34032=DIRECTION('center_axis',(-1.,5.24877093477881E-17,0.));
#34033=DIRECTION('ref_axis',(-5.24877093477881E-17,-1.,0.));
#34034=DIRECTION('center_axis',(-1.,5.24877093477881E-17,0.));
#34035=DIRECTION('ref_axis',(-5.24877093477881E-17,-1.,0.));
#34036=DIRECTION('center_axis',(-1.,5.24877093477881E-17,0.));
#34037=DIRECTION('ref_axis',(-5.24877093477881E-17,-1.,0.));
#34038=DIRECTION('center_axis',(-1.,0.,0.));
#34039=DIRECTION('ref_axis',(0.,0.,1.));
#34040=DIRECTION('',(1.,0.,0.));
#34041=DIRECTION('center_axis',(-1.,0.,0.));
#34042=DIRECTION('ref_axis',(0.,0.,1.));
#34043=DIRECTION('center_axis',(-1.,0.,0.));
#34044=DIRECTION('ref_axis',(0.,0.,1.));
#34045=DIRECTION('center_axis',(-1.,0.,0.));
#34046=DIRECTION('ref_axis',(0.,0.,1.));
#34047=DIRECTION('',(1.,0.,0.));
#34048=DIRECTION('center_axis',(-1.,0.,0.));
#34049=DIRECTION('ref_axis',(0.,0.,1.));
#34050=DIRECTION('center_axis',(-1.,0.,0.));
#34051=DIRECTION('ref_axis',(0.,0.,1.));
#34052=DIRECTION('center_axis',(-1.,0.,0.));
#34053=DIRECTION('ref_axis',(0.,0.,1.));
#34054=DIRECTION('',(1.,0.,0.));
#34055=DIRECTION('center_axis',(-1.,0.,0.));
#34056=DIRECTION('ref_axis',(0.,0.,1.));
#34057=DIRECTION('center_axis',(1.,0.,0.));
#34058=DIRECTION('ref_axis',(0.,0.,-1.));
#34059=DIRECTION('',(0.,0.5,-0.866025403784439));
#34060=DIRECTION('',(0.,1.,-1.87789324842145E-16));
#34061=DIRECTION('',(0.,0.5,0.866025403784439));
#34062=DIRECTION('',(0.,-0.5,0.866025403784439));
#34063=DIRECTION('',(0.,-1.,0.));
#34064=DIRECTION('',(0.,-0.5,-0.866025403784439));
#34065=DIRECTION('center_axis',(-1.,0.,0.));
#34066=DIRECTION('ref_axis',(0.,0.,1.));
#34067=DIRECTION('center_axis',(1.,0.,0.));
#34068=DIRECTION('ref_axis',(0.,0.,-1.));
#34069=DIRECTION('center_axis',(-1.,0.,0.));
#34070=DIRECTION('ref_axis',(0.,0.,1.));
#34071=DIRECTION('center_axis',(0.,1.87789324842145E-16,1.));
#34072=DIRECTION('ref_axis',(0.,-1.,1.87789324842145E-16));
#34073=DIRECTION('',(0.,1.,-1.87789324842145E-16));
#34074=DIRECTION('',(-1.,0.,0.));
#34075=DIRECTION('',(-1.,0.,0.));
#34076=DIRECTION('',(0.,1.,-1.87789324842145E-16));
#34077=DIRECTION('center_axis',(0.,-0.866025403784439,0.5));
#34078=DIRECTION('ref_axis',(0.,-0.5,-0.866025403784439));
#34079=DIRECTION('',(0.,0.5,0.866025403784439));
#34080=DIRECTION('',(-1.,0.,0.));
#34081=DIRECTION('',(0.,0.5,0.866025403784439));
#34082=DIRECTION('center_axis',(0.,-0.866025403784439,-0.5));
#34083=DIRECTION('ref_axis',(0.,0.5,-0.866025403784439));
#34084=DIRECTION('',(0.,-0.5,0.866025403784439));
#34085=DIRECTION('',(-1.,0.,0.));
#34086=DIRECTION('',(0.,-0.5,0.866025403784439));
#34087=DIRECTION('center_axis',(0.,0.,-1.));
#34088=DIRECTION('ref_axis',(-1.,0.,0.));
#34089=DIRECTION('',(0.,-1.,0.));
#34090=DIRECTION('',(-1.,0.,0.));
#34091=DIRECTION('',(0.,-1.,0.));
#34092=DIRECTION('center_axis',(0.,0.866025403784439,-0.5));
#34093=DIRECTION('ref_axis',(0.,0.5,0.866025403784439));
#34094=DIRECTION('',(0.,-0.5,-0.866025403784439));
#34095=DIRECTION('',(-1.,0.,0.));
#34096=DIRECTION('',(0.,-0.5,-0.866025403784439));
#34097=DIRECTION('center_axis',(0.,0.866025403784439,0.5));
#34098=DIRECTION('ref_axis',(0.,-0.5,0.866025403784439));
#34099=DIRECTION('',(0.,0.5,-0.866025403784439));
#34100=DIRECTION('',(0.,0.5,-0.866025403784439));
#34101=DIRECTION('center_axis',(-1.,0.,0.));
#34102=DIRECTION('ref_axis',(0.,0.,1.));
#34103=DIRECTION('center_axis',(-1.,0.,0.));
#34104=DIRECTION('ref_axis',(0.,0.,1.));
#34105=DIRECTION('center_axis',(-1.,0.,0.));
#34106=DIRECTION('ref_axis',(0.,0.,1.));
#34107=DIRECTION('center_axis',(-1.,0.,0.));
#34108=DIRECTION('ref_axis',(0.,0.,1.));
#34109=DIRECTION('center_axis',(-1.,0.,0.));
#34110=DIRECTION('ref_axis',(0.,0.,1.));
#34111=DIRECTION('center_axis',(-1.,0.,0.));
#34112=DIRECTION('ref_axis',(0.,0.,1.));
#34113=DIRECTION('center_axis',(-1.,-3.84779799073557E-18,0.));
#34114=DIRECTION('ref_axis',(3.84779799073557E-18,-1.,0.));
#34115=DIRECTION('center_axis',(-1.,-3.84779799073557E-18,0.));
#34116=DIRECTION('ref_axis',(3.84779799073557E-18,-1.,0.));
#34117=DIRECTION('',(1.,3.84779799073557E-18,0.));
#34118=DIRECTION('center_axis',(-1.,-3.84779799073557E-18,0.));
#34119=DIRECTION('ref_axis',(3.84779799073557E-18,-1.,0.));
#34120=DIRECTION('center_axis',(-1.,-3.84779799073557E-18,0.));
#34121=DIRECTION('ref_axis',(3.84779799073557E-18,-1.,0.));
#34122=DIRECTION('center_axis',(-1.,-3.84779799073557E-18,0.));
#34123=DIRECTION('ref_axis',(3.84779799073557E-18,-1.,0.));
#34124=DIRECTION('',(-1.,-3.84779799073557E-18,0.));
#34125=DIRECTION('center_axis',(-1.,-3.84779799073557E-18,0.));
#34126=DIRECTION('ref_axis',(3.84779799073557E-18,-1.,0.));
#34127=DIRECTION('center_axis',(1.,3.84779799073557E-18,0.));
#34128=DIRECTION('ref_axis',(-3.84779799073557E-18,1.,0.));
#34129=DIRECTION('center_axis',(-1.,-3.84779799073557E-18,0.));
#34130=DIRECTION('ref_axis',(3.84779799073557E-18,-1.,0.));
#34131=DIRECTION('center_axis',(-1.,-1.22125762314651E-17,0.));
#34132=DIRECTION('ref_axis',(-3.62527989531715E-33,1.83697019872103E-16,
-1.));
#34133=DIRECTION('center_axis',(-1.,-1.22125762314651E-17,0.));
#34134=DIRECTION('ref_axis',(1.22125762314651E-17,-1.,0.));
#34135=DIRECTION('',(1.,0.,0.));
#34136=DIRECTION('center_axis',(-1.,-1.22125762314651E-17,0.));
#34137=DIRECTION('ref_axis',(1.22125762314651E-17,-1.,0.));
#34138=DIRECTION('',(1.,0.,0.));
#34139=DIRECTION('center_axis',(-1.,-1.22125762314651E-17,0.));
#34140=DIRECTION('ref_axis',(-3.08148791101958E-33,1.83697019872103E-16,
-1.));
#34141=DIRECTION('center_axis',(-1.,-1.22125762314651E-17,0.));
#34142=DIRECTION('ref_axis',(1.22125762314651E-17,-1.,0.));
#34143=DIRECTION('',(1.,0.,0.));
#34144=DIRECTION('center_axis',(-1.,-1.22125762314651E-17,0.));
#34145=DIRECTION('ref_axis',(1.22125762314651E-17,-1.,0.));
#34146=DIRECTION('',(1.,0.,0.));
#34147=DIRECTION('center_axis',(1.,1.22125762314651E-17,0.));
#34148=DIRECTION('ref_axis',(-1.22125762314651E-17,1.,0.));
#34149=DIRECTION('',(0.,0.,-1.));
#34150=DIRECTION('',(0.,0.,1.));
#34151=DIRECTION('center_axis',(-1.,-1.22125762314651E-17,0.));
#34152=DIRECTION('ref_axis',(1.22125762314651E-17,-1.,0.));
#34153=DIRECTION('',(0.,0.,-1.));
#34154=DIRECTION('',(0.,0.,1.));
#34155=DIRECTION('center_axis',(0.,1.,0.));
#34156=DIRECTION('ref_axis',(0.,0.,1.));
#34157=DIRECTION('center_axis',(0.,-1.,0.));
#34158=DIRECTION('ref_axis',(0.,0.,-1.));
#34159=DIRECTION('axis',(0.,0.,1.));
#34160=DIRECTION('refdir',(1.,0.,0.));
#34161=DIRECTION('center_axis',(1.,1.22464679914735E-16,0.));
#34162=DIRECTION('ref_axis',(-1.22464679914735E-16,1.,0.));
#34163=DIRECTION('center_axis',(1.,1.22464679914735E-16,0.));
#34164=DIRECTION('ref_axis',(-1.22464679914735E-16,1.,0.));
#34165=DIRECTION('',(-1.,-1.22464679914735E-16,0.));
#34166=DIRECTION('center_axis',(1.,1.22464679914735E-16,0.));
#34167=DIRECTION('ref_axis',(-1.22464679914735E-16,1.,0.));
#34168=DIRECTION('center_axis',(1.,1.22464679914735E-16,0.));
#34169=DIRECTION('ref_axis',(-1.22464679914735E-16,1.,0.));
#34170=DIRECTION('',(-0.707106781186546,0.707106781186549,8.65956056235495E-17));
#34171=DIRECTION('center_axis',(1.,1.22464679914735E-16,0.));
#34172=DIRECTION('ref_axis',(-1.22464679914735E-16,1.,0.));
#34173=DIRECTION('center_axis',(-1.,-1.22464679914735E-16,0.));
#34174=DIRECTION('ref_axis',(1.22464679914735E-16,-1.,0.));
#34175=DIRECTION('center_axis',(1.,1.22464679914735E-16,0.));
#34176=DIRECTION('ref_axis',(-1.22464679914735E-16,1.,0.));
#34177=DIRECTION('',(0.707106781186552,-0.707106781186543,8.65956056235488E-17));
#34178=DIRECTION('center_axis',(1.,1.22464679914735E-16,0.));
#34179=DIRECTION('ref_axis',(-1.22464679914735E-16,1.,0.));
#34180=DIRECTION('center_axis',(1.,1.22464679914735E-16,0.));
#34181=DIRECTION('ref_axis',(-1.22464679914735E-16,1.,0.));
#34182=DIRECTION('center_axis',(1.,1.22464679914735E-16,0.));
#34183=DIRECTION('ref_axis',(-1.22464679914735E-16,1.,0.));
#34184=DIRECTION('',(-1.,-1.22464679914735E-16,0.));
#34185=DIRECTION('center_axis',(1.,1.22464679914735E-16,0.));
#34186=DIRECTION('ref_axis',(-1.22464679914735E-16,1.,0.));
#34187=DIRECTION('center_axis',(1.,1.22464679914735E-16,0.));
#34188=DIRECTION('ref_axis',(-1.22464679914735E-16,1.,0.));
#34189=DIRECTION('center_axis',(-1.,-1.22464679914735E-16,0.));
#34190=DIRECTION('ref_axis',(1.22464679914735E-16,-1.,0.));
#34191=DIRECTION('',(0.,0.5,-0.866025403784439));
#34192=DIRECTION('',(0.,1.,0.));
#34193=DIRECTION('',(0.,0.5,0.866025403784439));
#34194=DIRECTION('',(0.,-0.5,0.866025403784438));
#34195=DIRECTION('',(0.,-1.,-1.50231459873716E-16));
#34196=DIRECTION('',(0.,-0.5,-0.866025403784439));
#34197=DIRECTION('center_axis',(1.,1.22464679914735E-16,0.));
#34198=DIRECTION('ref_axis',(-1.22464679914735E-16,1.,0.));
#34199=DIRECTION('center_axis',(-1.06057523872491E-16,0.866025403784439,
0.5));
#34200=DIRECTION('ref_axis',(-5.09861652542584E-33,-0.5,0.866025403784439));
#34201=DIRECTION('',(-1.,-1.22464679914735E-16,0.));
#34202=DIRECTION('',(0.,0.5,-0.866025403784439));
#34203=DIRECTION('',(-1.,-1.22464679914735E-16,0.));
#34204=DIRECTION('center_axis',(0.,0.,1.));
#34205=DIRECTION('ref_axis',(1.,0.,0.));
#34206=DIRECTION('',(0.,1.,0.));
#34207=DIRECTION('',(-1.,-1.22464679914735E-16,0.));
#34208=DIRECTION('center_axis',(1.06057523872491E-16,-0.866025403784439,
0.5));
#34209=DIRECTION('ref_axis',(-8.4117933897259E-34,-0.5,-0.866025403784439));
#34210=DIRECTION('',(0.,0.5,0.866025403784439));
#34211=DIRECTION('',(-1.,-1.22464679914735E-16,0.));
#34212=DIRECTION('center_axis',(1.06057523872491E-16,-0.866025403784439,
-0.5));
#34213=DIRECTION('ref_axis',(-5.93979586439842E-33,0.5,-0.866025403784439));
#34214=DIRECTION('',(0.,-0.5,0.866025403784438));
#34215=DIRECTION('',(-1.,-1.22464679914735E-16,0.));
#34216=DIRECTION('center_axis',(-1.8398047646558E-32,1.50231459873716E-16,
-1.));
#34217=DIRECTION('ref_axis',(0.,1.,1.50231459873716E-16));
#34218=DIRECTION('',(0.,-1.,-1.50231459873716E-16));
#34219=DIRECTION('',(-1.,-1.22464679914735E-16,0.));
#34220=DIRECTION('center_axis',(-1.06057523872491E-16,0.866025403784439,
-0.5));
#34221=DIRECTION('ref_axis',(2.96989793219921E-33,0.5,0.866025403784439));
#34222=DIRECTION('',(0.,-0.5,-0.866025403784439));
#34223=DIRECTION('center_axis',(-1.,0.,0.));
#34224=DIRECTION('ref_axis',(0.,0.,1.));
#34225=DIRECTION('axis',(0.,0.,1.));
#34226=DIRECTION('refdir',(1.,0.,0.));
#34227=DIRECTION('center_axis',(1.,0.,0.));
#34228=DIRECTION('ref_axis',(0.,0.,-1.));
#34229=DIRECTION('center_axis',(1.,0.,0.));
#34230=DIRECTION('ref_axis',(0.,0.,-1.));
#34231=DIRECTION('center_axis',(1.,0.,0.));
#34232=DIRECTION('ref_axis',(0.,0.,-1.));
#34233=DIRECTION('',(-0.707106781186551,8.65956056235489E-17,-0.707106781186544));
#34234=DIRECTION('center_axis',(-1.,0.,0.));
#34235=DIRECTION('ref_axis',(0.,0.,-1.));
#34236=DIRECTION('center_axis',(-1.,7.08538566198487E-17,0.));
#34237=DIRECTION('ref_axis',(-7.08538566198487E-17,-1.,0.));
#34238=DIRECTION('',(-0.515038074910058,0.85716730070211,-1.04972719113862E-16));
#34239=DIRECTION('center_axis',(-1.,7.08538566198487E-17,0.));
#34240=DIRECTION('ref_axis',(-7.08538566198487E-17,-1.,0.));
#34241=DIRECTION('center_axis',(-1.,7.08538566198487E-17,0.));
#34242=DIRECTION('ref_axis',(-7.08538566198487E-17,-1.,0.));
#34243=DIRECTION('center_axis',(-1.,7.08538566198487E-17,0.));
#34244=DIRECTION('ref_axis',(-7.08538566198487E-17,-1.,0.));
#34245=DIRECTION('center_axis',(-1.,7.08538566198487E-17,0.));
#34246=DIRECTION('ref_axis',(-7.08538566198487E-17,-1.,0.));
#34247=DIRECTION('center_axis',(-1.,7.08538566198487E-17,0.));
#34248=DIRECTION('ref_axis',(-7.08538566198487E-17,-1.,0.));
#34249=DIRECTION('center_axis',(-1.,7.08538566198487E-17,0.));
#34250=DIRECTION('ref_axis',(-7.08538566198487E-17,-1.,0.));
#34251=DIRECTION('center_axis',(-1.,7.08538566198487E-17,0.));
#34252=DIRECTION('ref_axis',(-7.08538566198487E-17,-1.,0.));
#34253=DIRECTION('center_axis',(-1.,0.,0.));
#34254=DIRECTION('ref_axis',(0.,0.,1.));
#34255=DIRECTION('',(1.,0.,0.));
#34256=DIRECTION('center_axis',(-1.,0.,0.));
#34257=DIRECTION('ref_axis',(0.,0.,1.));
#34258=DIRECTION('center_axis',(-1.,0.,0.));
#34259=DIRECTION('ref_axis',(0.,0.,1.));
#34260=DIRECTION('center_axis',(-1.,0.,0.));
#34261=DIRECTION('ref_axis',(0.,0.,1.));
#34262=DIRECTION('',(1.,0.,0.));
#34263=DIRECTION('center_axis',(-1.,0.,0.));
#34264=DIRECTION('ref_axis',(0.,0.,1.));
#34265=DIRECTION('center_axis',(-1.,0.,0.));
#34266=DIRECTION('ref_axis',(0.,0.,1.));
#34267=DIRECTION('center_axis',(-1.,0.,0.));
#34268=DIRECTION('ref_axis',(0.,0.,1.));
#34269=DIRECTION('',(1.,0.,0.));
#34270=DIRECTION('center_axis',(-1.,0.,0.));
#34271=DIRECTION('ref_axis',(0.,0.,1.));
#34272=DIRECTION('center_axis',(1.,0.,0.));
#34273=DIRECTION('ref_axis',(0.,0.,-1.));
#34274=DIRECTION('',(0.,0.5,-0.866025403784439));
#34275=DIRECTION('',(0.,1.,-1.25192883228097E-16));
#34276=DIRECTION('',(0.,0.5,0.866025403784439));
#34277=DIRECTION('',(0.,-0.5,0.866025403784439));
#34278=DIRECTION('',(0.,-1.,0.));
#34279=DIRECTION('',(0.,-0.5,-0.866025403784439));
#34280=DIRECTION('center_axis',(-1.,0.,0.));
#34281=DIRECTION('ref_axis',(0.,0.,1.));
#34282=DIRECTION('center_axis',(1.,0.,0.));
#34283=DIRECTION('ref_axis',(0.,0.,-1.));
#34284=DIRECTION('center_axis',(-1.,0.,0.));
#34285=DIRECTION('ref_axis',(0.,0.,1.));
#34286=DIRECTION('center_axis',(0.,1.25192883228097E-16,1.));
#34287=DIRECTION('ref_axis',(0.,-1.,1.25192883228097E-16));
#34288=DIRECTION('',(0.,1.,-1.25192883228097E-16));
#34289=DIRECTION('',(-1.,0.,0.));
#34290=DIRECTION('',(-1.,0.,0.));
#34291=DIRECTION('',(0.,1.,-1.25192883228097E-16));
#34292=DIRECTION('center_axis',(0.,-0.866025403784439,0.5));
#34293=DIRECTION('ref_axis',(0.,-0.5,-0.866025403784439));
#34294=DIRECTION('',(0.,0.5,0.866025403784439));
#34295=DIRECTION('',(-1.,0.,0.));
#34296=DIRECTION('',(0.,0.5,0.866025403784439));
#34297=DIRECTION('center_axis',(0.,-0.866025403784439,-0.5));
#34298=DIRECTION('ref_axis',(0.,0.5,-0.866025403784439));
#34299=DIRECTION('',(0.,-0.5,0.866025403784439));
#34300=DIRECTION('',(-1.,0.,0.));
#34301=DIRECTION('',(0.,-0.5,0.866025403784439));
#34302=DIRECTION('center_axis',(0.,0.,-1.));
#34303=DIRECTION('ref_axis',(-1.,0.,0.));
#34304=DIRECTION('',(0.,-1.,0.));
#34305=DIRECTION('',(-1.,0.,0.));
#34306=DIRECTION('',(0.,-1.,0.));
#34307=DIRECTION('center_axis',(0.,0.866025403784439,-0.5));
#34308=DIRECTION('ref_axis',(0.,0.5,0.866025403784439));
#34309=DIRECTION('',(0.,-0.5,-0.866025403784439));
#34310=DIRECTION('',(-1.,0.,0.));
#34311=DIRECTION('',(0.,-0.5,-0.866025403784439));
#34312=DIRECTION('center_axis',(0.,0.866025403784439,0.5));
#34313=DIRECTION('ref_axis',(0.,-0.5,0.866025403784439));
#34314=DIRECTION('',(0.,0.5,-0.866025403784439));
#34315=DIRECTION('',(0.,0.5,-0.866025403784439));
#34316=DIRECTION('center_axis',(-1.,0.,0.));
#34317=DIRECTION('ref_axis',(0.,0.,1.));
#34318=DIRECTION('center_axis',(-1.,0.,0.));
#34319=DIRECTION('ref_axis',(0.,0.,1.));
#34320=DIRECTION('center_axis',(-1.,0.,0.));
#34321=DIRECTION('ref_axis',(0.,0.,1.));
#34322=DIRECTION('center_axis',(-1.,0.,0.));
#34323=DIRECTION('ref_axis',(0.,0.,1.));
#34324=DIRECTION('center_axis',(-1.,0.,0.));
#34325=DIRECTION('ref_axis',(0.,0.,1.));
#34326=DIRECTION('center_axis',(-1.,0.,0.));
#34327=DIRECTION('ref_axis',(0.,0.,1.));
#34328=DIRECTION('center_axis',(-1.,-1.17680295328379E-17,0.));
#34329=DIRECTION('ref_axis',(1.17680295328379E-17,-1.,0.));
#34330=DIRECTION('center_axis',(-1.,-1.17680295328379E-17,0.));
#34331=DIRECTION('ref_axis',(1.17680295328379E-17,-1.,0.));
#34332=DIRECTION('',(1.,1.17680295328379E-17,0.));
#34333=DIRECTION('center_axis',(-1.,-1.17680295328379E-17,0.));
#34334=DIRECTION('ref_axis',(1.17680295328379E-17,-1.,0.));
#34335=DIRECTION('center_axis',(-1.,-1.17680295328379E-17,0.));
#34336=DIRECTION('ref_axis',(1.17680295328379E-17,-1.,0.));
#34337=DIRECTION('center_axis',(-1.,-1.17680295328379E-17,0.));
#34338=DIRECTION('ref_axis',(1.17680295328379E-17,-1.,0.));
#34339=DIRECTION('',(-1.,-1.17680295328379E-17,0.));
#34340=DIRECTION('center_axis',(-1.,-1.17680295328379E-17,0.));
#34341=DIRECTION('ref_axis',(1.17680295328379E-17,-1.,0.));
#34342=DIRECTION('center_axis',(1.,1.17680295328379E-17,0.));
#34343=DIRECTION('ref_axis',(-1.17680295328379E-17,1.,0.));
#34344=DIRECTION('center_axis',(-1.,-1.17680295328379E-17,0.));
#34345=DIRECTION('ref_axis',(1.17680295328379E-17,-1.,0.));
#34346=DIRECTION('center_axis',(-1.,-3.79192062724778E-17,0.));
#34347=DIRECTION('ref_axis',(-8.5006563062609E-33,1.83697019872103E-16,
-1.));
#34348=DIRECTION('center_axis',(-1.,-3.79192062724778E-17,0.));
#34349=DIRECTION('ref_axis',(3.79192062724778E-17,-1.,0.));
#34350=DIRECTION('',(1.,0.,0.));
#34351=DIRECTION('center_axis',(-1.,-3.79192062724778E-17,0.));
#34352=DIRECTION('ref_axis',(3.79192062724778E-17,-1.,0.));
#34353=DIRECTION('',(1.,0.,0.));
#34354=DIRECTION('center_axis',(-1.,-3.79192062724778E-17,0.));
#34355=DIRECTION('ref_axis',(-7.70371977754894E-33,1.83697019872103E-16,
-1.));
#34356=DIRECTION('center_axis',(-1.,-3.79192062724778E-17,0.));
#34357=DIRECTION('ref_axis',(3.79192062724778E-17,-1.,0.));
#34358=DIRECTION('',(1.,0.,0.));
#34359=DIRECTION('center_axis',(-1.,-3.79192062724778E-17,0.));
#34360=DIRECTION('ref_axis',(3.79192062724778E-17,-1.,0.));
#34361=DIRECTION('',(1.,0.,0.));
#34362=DIRECTION('center_axis',(1.,3.79192062724778E-17,0.));
#34363=DIRECTION('ref_axis',(-3.79192062724778E-17,1.,0.));
#34364=DIRECTION('',(0.,-6.27682405047592E-17,-1.));
#34365=DIRECTION('',(0.,-6.27682405047592E-17,1.));
#34366=DIRECTION('center_axis',(-1.,-3.79192062724778E-17,0.));
#34367=DIRECTION('ref_axis',(3.79192062724778E-17,-1.,0.));
#34368=DIRECTION('',(0.,-6.27682405047592E-17,-1.));
#34369=DIRECTION('',(0.,-6.27682405047592E-17,1.));
#34370=DIRECTION('center_axis',(0.,1.,6.27682405047592E-17));
#34371=DIRECTION('ref_axis',(0.,-6.27682405047592E-17,1.));
#34372=DIRECTION('center_axis',(0.,-1.,6.27682405047592E-17));
#34373=DIRECTION('ref_axis',(0.,-6.27682405047592E-17,-1.));
#34374=DIRECTION('axis',(0.,0.,1.));
#34375=DIRECTION('refdir',(1.,0.,0.));
#34376=DIRECTION('center_axis',(1.,1.22464679914735E-16,0.));
#34377=DIRECTION('ref_axis',(-1.22464679914735E-16,1.,0.));
#34378=DIRECTION('center_axis',(1.,1.22464679914735E-16,0.));
#34379=DIRECTION('ref_axis',(-1.22464679914735E-16,1.,0.));
#34380=DIRECTION('',(-1.,-1.22464679914735E-16,0.));
#34381=DIRECTION('center_axis',(1.,1.22464679914735E-16,0.));
#34382=DIRECTION('ref_axis',(-1.22464679914735E-16,1.,0.));
#34383=DIRECTION('center_axis',(1.,1.22464679914735E-16,0.));
#34384=DIRECTION('ref_axis',(-1.22464679914735E-16,1.,0.));
#34385=DIRECTION('',(-0.70710678118655,0.707106781186545,8.6595605623549E-17));
#34386=DIRECTION('center_axis',(1.,1.22464679914735E-16,0.));
#34387=DIRECTION('ref_axis',(-1.22464679914735E-16,1.,0.));
#34388=DIRECTION('center_axis',(-1.,-1.22464679914735E-16,0.));
#34389=DIRECTION('ref_axis',(1.22464679914735E-16,-1.,0.));
#34390=DIRECTION('center_axis',(1.,1.22464679914735E-16,0.));
#34391=DIRECTION('ref_axis',(-1.22464679914735E-16,1.,0.));
#34392=DIRECTION('',(0.707106781186548,-0.707106781186547,8.65956056235493E-17));
#34393=DIRECTION('center_axis',(1.,1.22464679914735E-16,0.));
#34394=DIRECTION('ref_axis',(-1.22464679914735E-16,1.,0.));
#34395=DIRECTION('center_axis',(1.,1.22464679914735E-16,0.));
#34396=DIRECTION('ref_axis',(-1.22464679914735E-16,1.,0.));
#34397=DIRECTION('center_axis',(1.,1.22464679914735E-16,0.));
#34398=DIRECTION('ref_axis',(-1.22464679914735E-16,1.,0.));
#34399=DIRECTION('',(-1.,-1.22464679914735E-16,0.));
#34400=DIRECTION('center_axis',(1.,1.22464679914735E-16,0.));
#34401=DIRECTION('ref_axis',(-1.22464679914735E-16,1.,0.));
#34402=DIRECTION('center_axis',(1.,1.22464679914735E-16,0.));
#34403=DIRECTION('ref_axis',(-1.22464679914735E-16,1.,0.));
#34404=DIRECTION('center_axis',(-1.,-1.22464679914735E-16,0.));
#34405=DIRECTION('ref_axis',(1.22464679914735E-16,-1.,0.));
#34406=DIRECTION('',(0.,0.5,-0.866025403784439));
#34407=DIRECTION('',(0.,1.,0.));
#34408=DIRECTION('',(0.,0.5,0.866025403784439));
#34409=DIRECTION('',(0.,-0.5,0.866025403784438));
#34410=DIRECTION('',(0.,-1.,-1.50231459873716E-16));
#34411=DIRECTION('',(0.,-0.5,-0.866025403784439));
#34412=DIRECTION('center_axis',(1.,1.22464679914735E-16,0.));
#34413=DIRECTION('ref_axis',(-1.22464679914735E-16,1.,0.));
#34414=DIRECTION('center_axis',(-1.06057523872491E-16,0.866025403784439,
0.5));
#34415=DIRECTION('ref_axis',(-5.09861652542584E-33,-0.5,0.866025403784439));
#34416=DIRECTION('',(-1.,-1.22464679914735E-16,0.));
#34417=DIRECTION('',(0.,0.5,-0.866025403784439));
#34418=DIRECTION('',(-1.,-1.22464679914735E-16,0.));
#34419=DIRECTION('center_axis',(0.,0.,1.));
#34420=DIRECTION('ref_axis',(1.,0.,0.));
#34421=DIRECTION('',(0.,1.,0.));
#34422=DIRECTION('',(-1.,-1.22464679914735E-16,0.));
#34423=DIRECTION('center_axis',(1.06057523872491E-16,-0.866025403784439,
0.5));
#34424=DIRECTION('ref_axis',(-8.4117933897259E-34,-0.5,-0.866025403784439));
#34425=DIRECTION('',(0.,0.5,0.866025403784439));
#34426=DIRECTION('',(-1.,-1.22464679914735E-16,0.));
#34427=DIRECTION('center_axis',(1.06057523872491E-16,-0.866025403784439,
-0.5));
#34428=DIRECTION('ref_axis',(-5.93979586439842E-33,0.5,-0.866025403784439));
#34429=DIRECTION('',(0.,-0.5,0.866025403784438));
#34430=DIRECTION('',(-1.,-1.22464679914735E-16,0.));
#34431=DIRECTION('center_axis',(-1.8398047646558E-32,1.50231459873716E-16,
-1.));
#34432=DIRECTION('ref_axis',(0.,1.,1.50231459873716E-16));
#34433=DIRECTION('',(0.,-1.,-1.50231459873716E-16));
#34434=DIRECTION('',(-1.,-1.22464679914735E-16,0.));
#34435=DIRECTION('center_axis',(-1.06057523872491E-16,0.866025403784439,
-0.5));
#34436=DIRECTION('ref_axis',(2.96989793219921E-33,0.5,0.866025403784439));
#34437=DIRECTION('',(0.,-0.5,-0.866025403784439));
#34438=DIRECTION('center_axis',(-1.,0.,0.));
#34439=DIRECTION('ref_axis',(0.,0.,1.));
#34440=DIRECTION('axis',(0.,0.,1.));
#34441=DIRECTION('refdir',(1.,0.,0.));
#34442=DIRECTION('center_axis',(1.,1.22464679914735E-16,0.));
#34443=DIRECTION('ref_axis',(-1.22464679914735E-16,1.,0.));
#34444=DIRECTION('center_axis',(1.,1.22464679914735E-16,0.));
#34445=DIRECTION('ref_axis',(-1.22464679914735E-16,1.,0.));
#34446=DIRECTION('',(-1.,-1.22464679914735E-16,0.));
#34447=DIRECTION('center_axis',(1.,1.22464679914735E-16,0.));
#34448=DIRECTION('ref_axis',(-1.22464679914735E-16,1.,0.));
#34449=DIRECTION('center_axis',(1.,1.22464679914735E-16,0.));
#34450=DIRECTION('ref_axis',(-1.22464679914735E-16,1.,0.));
#34451=DIRECTION('',(-0.707106781186548,0.707106781186547,8.65956056235492E-17));
#34452=DIRECTION('center_axis',(1.,1.22464679914735E-16,0.));
#34453=DIRECTION('ref_axis',(-1.22464679914735E-16,1.,0.));
#34454=DIRECTION('center_axis',(-1.,-1.22464679914735E-16,0.));
#34455=DIRECTION('ref_axis',(1.22464679914735E-16,-1.,0.));
#34456=DIRECTION('center_axis',(1.,1.22464679914735E-16,0.));
#34457=DIRECTION('ref_axis',(-1.22464679914735E-16,1.,0.));
#34458=DIRECTION('',(0.707106781186552,-0.707106781186543,8.65956056235488E-17));
#34459=DIRECTION('center_axis',(1.,1.22464679914735E-16,0.));
#34460=DIRECTION('ref_axis',(-1.22464679914735E-16,1.,0.));
#34461=DIRECTION('center_axis',(1.,1.22464679914735E-16,0.));
#34462=DIRECTION('ref_axis',(-1.22464679914735E-16,1.,0.));
#34463=DIRECTION('center_axis',(1.,1.22464679914735E-16,0.));
#34464=DIRECTION('ref_axis',(-1.22464679914735E-16,1.,0.));
#34465=DIRECTION('',(-1.,-1.22464679914735E-16,0.));
#34466=DIRECTION('center_axis',(1.,1.22464679914735E-16,0.));
#34467=DIRECTION('ref_axis',(-1.22464679914735E-16,1.,0.));
#34468=DIRECTION('center_axis',(1.,1.22464679914735E-16,0.));
#34469=DIRECTION('ref_axis',(-1.22464679914735E-16,1.,0.));
#34470=DIRECTION('center_axis',(-1.,-1.22464679914735E-16,0.));
#34471=DIRECTION('ref_axis',(1.22464679914735E-16,-1.,0.));
#34472=DIRECTION('',(0.,0.5,-0.866025403784439));
#34473=DIRECTION('',(0.,1.,2.50385766456193E-16));
#34474=DIRECTION('',(0.,0.5,0.866025403784439));
#34475=DIRECTION('',(0.,-0.5,0.866025403784438));
#34476=DIRECTION('',(0.,-1.,0.));
#34477=DIRECTION('',(0.,-0.5,-0.866025403784439));
#34478=DIRECTION('center_axis',(1.,1.22464679914735E-16,0.));
#34479=DIRECTION('ref_axis',(-1.22464679914735E-16,1.,0.));
#34480=DIRECTION('center_axis',(-1.06057523872491E-16,0.866025403784439,
0.5));
#34481=DIRECTION('ref_axis',(4.03425722881252E-33,-0.5,0.866025403784439));
#34482=DIRECTION('',(-1.,-1.22464679914735E-16,0.));
#34483=DIRECTION('',(0.,0.5,-0.866025403784439));
#34484=DIRECTION('',(-1.,-1.22464679914735E-16,0.));
#34485=DIRECTION('center_axis',(3.06634127442634E-32,-2.50385766456193E-16,
1.));
#34486=DIRECTION('ref_axis',(0.,-1.,-2.50385766456193E-16));
#34487=DIRECTION('',(0.,1.,2.50385766456193E-16));
#34488=DIRECTION('',(-1.,-1.22464679914735E-16,0.));
#34489=DIRECTION('center_axis',(1.06057523872491E-16,-0.866025403784439,
0.5));
#34490=DIRECTION('ref_axis',(-2.96989793219921E-33,-0.5,-0.866025403784439));
#34491=DIRECTION('',(0.,0.5,0.866025403784439));
#34492=DIRECTION('',(-1.,-1.22464679914735E-16,0.));
#34493=DIRECTION('center_axis',(1.06057523872491E-16,-0.866025403784439,
-0.5));
#34494=DIRECTION('ref_axis',(-4.03425722881252E-33,0.5,-0.866025403784439));
#34495=DIRECTION('',(0.,-0.5,0.866025403784438));
#34496=DIRECTION('',(-1.,-1.22464679914735E-16,0.));
#34497=DIRECTION('center_axis',(0.,0.,-1.));
#34498=DIRECTION('ref_axis',(-1.,0.,0.));
#34499=DIRECTION('',(0.,-1.,0.));
#34500=DIRECTION('',(-1.,-1.22464679914735E-16,0.));
#34501=DIRECTION('center_axis',(-1.06057523872491E-16,0.866025403784439,
-0.5));
#34502=DIRECTION('ref_axis',(4.03425722881253E-33,0.5,0.866025403784439));
#34503=DIRECTION('',(0.,-0.5,-0.866025403784439));
#34504=DIRECTION('center_axis',(-1.,0.,0.));
#34505=DIRECTION('ref_axis',(0.,0.,1.));
#34506=DIRECTION('',(-4.5073300221945E-16,-1.,-8.07537495060514E-17));
#34507=DIRECTION('',(1.,-4.5073300221945E-16,-5.55111512312576E-17));
#34508=DIRECTION('',(-1.,4.5073300221945E-16,5.55111512312576E-17));
#34509=DIRECTION('',(5.55111512312576E-17,-8.0546287827281E-17,1.));
#34510=DIRECTION('',(5.55111512312576E-17,-8.0546287827281E-17,1.));
#34511=DIRECTION('',(-1.,4.5073300221945E-16,5.55111512312576E-17));
#34512=DIRECTION('',(5.42599571062591E-16,1.,2.23147540040148E-16));
#34513=DIRECTION('',(6.93889464437771E-17,-2.23147540040149E-16,1.));
#34514=DIRECTION('',(1.,-8.98144108254207E-16,-8.32667268468865E-17));
#34515=DIRECTION('',(8.32667268468863E-17,-2.43284111655657E-16,1.));
#34516=DIRECTION('',(1.,-1.25327657546597E-15,5.82867087928207E-16));
#34517=DIRECTION('',(-5.82867087928207E-16,1.16001952307546E-16,1.));
#34518=DIRECTION('',(-1.50933018765266E-16,-1.,-2.53345869017621E-16));
#34519=DIRECTION('',(-1.,1.50933018765266E-16,8.32667268468864E-17));
#34520=DIRECTION('',(-8.33920355819539E-16,-1.,-9.90584807164179E-17));
#34521=DIRECTION('',(1.,-8.33920355819539E-16,-1.80411241501588E-16));
#34522=DIRECTION('',(0.,0.,1.));
#34523=DIRECTION('',(1.,0.,0.));
#34524=DIRECTION('',(-0.709546664443677,0.704658449872598,-4.88441536442122E-18));
#34525=DIRECTION('',(-6.4491047261943E-18,4.37764731775903E-19,1.));
#34526=DIRECTION('',(1.,2.77555756156289E-17,4.33010681256471E-29));
#34527=DIRECTION('',(-2.77555756156289E-17,1.,1.22464679914694E-16));
#34528=DIRECTION('',(1.22464679914735E-16,-1.,0.));
#34529=DIRECTION('',(1.,1.22464679914735E-16,-1.22464679914735E-16));
#34530=DIRECTION('',(-3.55404041318072E-32,1.22464679914735E-16,1.));
#34531=DIRECTION('',(1.22464679914735E-16,-1.,1.22464679914735E-16));
#34532=DIRECTION('',(5.55111512312576E-17,-8.0546287827281E-17,1.));
#34533=DIRECTION('',(-1.,4.5073300221945E-16,5.55111512312576E-17));
#34534=DIRECTION('',(0.00917060220956452,-6.94718371857935E-16,0.99995794914342));
#34535=DIRECTION('',(6.78825748670609E-16,1.,6.88522083890669E-16));
#34536=DIRECTION('',(0.951318325679895,-0.308210063472303,-7.11898636950769E-17));
#34537=DIRECTION('',(-8.72816584845502E-17,-3.84243700013842E-17,-1.));
#34538=DIRECTION('',(-0.568493171869114,-0.822687980669582,-3.47067524454931E-17));
#34539=DIRECTION('',(-1.56261371453658E-16,1.50166622153945E-16,-1.));
#34540=DIRECTION('',(-0.979426759612045,-0.20179995677861,-2.15172294371058E-17));
#34541=DIRECTION('',(-3.47582008972345E-18,1.23496263539437E-16,-1.));
#34542=DIRECTION('',(-5.55111512312576E-17,8.93081782155988E-17,-1.));
#34543=DIRECTION('',(3.15183454675772E-16,1.,8.93081782155987E-17));
#34544=DIRECTION('',(-1.,4.5073300221945E-16,5.55111512312576E-17));
#34545=DIRECTION('',(5.55111512312576E-17,-8.0546287827281E-17,1.));
#34546=DIRECTION('',(-0.0250517396628792,-5.67480107562551E-16,0.999686155920879));
#34547=DIRECTION('',(2.7264405065344E-18,1.,5.67726587268301E-16));
#34548=DIRECTION('',(-0.50830027520806,-0.861179905840476,-4.11485111189334E-17));
#34549=DIRECTION('',(-1.60975272749014E-16,1.42795118331208E-16,-1.));
#34550=DIRECTION('',(0.979426759612045,-0.20179995677861,-2.15172294370209E-17));
#34551=DIRECTION('',(3.47582008981007E-18,1.23496263539437E-16,-1.));
#34552=DIRECTION('',(0.970260862360484,-0.2420616842284,-2.97224983180942E-17));
#34553=DIRECTION('',(1.01167001946839E-18,1.26844040772007E-16,-1.));
#34554=DIRECTION('',(-0.970260862360484,-0.2420616842284,-2.97224983181783E-17));
#34555=DIRECTION('',(-1.01167001938177E-18,1.26844040772007E-16,-1.));
#34556=DIRECTION('',(0.125965052119064,0.992034679658247,1.21810889615276E-16));
#34557=DIRECTION('',(-4.14609915188478E-18,1.23315399874103E-16,-1.));
#34558=DIRECTION('',(-0.125965052119064,0.992034679658247,1.21810889615265E-16));
#34559=DIRECTION('',(4.14609915197138E-18,1.23315399874103E-16,-1.));
#34560=DIRECTION('',(-5.55111512312576E-17,8.93081782155988E-17,-1.));
#34561=DIRECTION('',(3.15183454675772E-16,1.,8.93081782155987E-17));
#34562=DIRECTION('',(-5.55111512312576E-17,8.93081782155988E-17,-1.));
#34563=DIRECTION('',(3.15183454675772E-16,1.,8.93081782155987E-17));
#34564=DIRECTION('',(-5.55111512312576E-17,8.93081782155988E-17,-1.));
#34565=DIRECTION('',(3.15183454675772E-16,1.,8.93081782155987E-17));
#34566=DIRECTION('',(-5.55111512312576E-17,8.93081782155988E-17,-1.));
#34567=DIRECTION('',(3.15183454675772E-16,1.,8.93081782155987E-17));
#34568=DIRECTION('',(-5.55111512312576E-17,8.93081782155988E-17,-1.));
#34569=DIRECTION('',(3.15183454675772E-16,1.,8.93081782155987E-17));
#34570=DIRECTION('',(-5.55111512312576E-17,8.93081782155988E-17,-1.));
#34571=DIRECTION('',(3.15183454675772E-16,1.,8.93081782155987E-17));
#34572=DIRECTION('',(-5.55111512312576E-17,8.93081782155988E-17,-1.));
#34573=DIRECTION('',(3.15183454675772E-16,1.,8.93081782155987E-17));
#34574=DIRECTION('',(-5.55111512312576E-17,8.93081782155988E-17,-1.));
#34575=DIRECTION('',(3.15183454675772E-16,1.,8.93081782155987E-17));
#34576=DIRECTION('',(-5.55111512312576E-17,8.93081782155988E-17,-1.));
#34577=DIRECTION('',(3.15183454675772E-16,1.,8.93081782155987E-17));
#34578=DIRECTION('',(-5.55111512312576E-17,8.93081782155988E-17,-1.));
#34579=DIRECTION('',(3.15183454675772E-16,1.,8.93081782155987E-17));
#34580=DIRECTION('',(-5.55111512312576E-17,8.93081782155988E-17,-1.));
#34581=DIRECTION('',(3.15183454675772E-16,1.,8.93081782155987E-17));
#34582=DIRECTION('',(-5.55111512312576E-17,8.93081782155988E-17,-1.));
#34583=DIRECTION('',(3.15183454675772E-16,1.,8.93081782155987E-17));
#34584=DIRECTION('',(-5.55111512312576E-17,8.93081782155988E-17,-1.));
#34585=DIRECTION('',(3.15183454675772E-16,1.,8.93081782155987E-17));
#34586=DIRECTION('',(-5.55111512312576E-17,8.93081782155988E-17,-1.));
#34587=DIRECTION('',(3.15183454675772E-16,1.,8.93081782155987E-17));
#34588=DIRECTION('',(-5.55111512312576E-17,8.93081782155988E-17,-1.));
#34589=DIRECTION('',(3.15183454675772E-16,1.,8.93081782155987E-17));
#34590=DIRECTION('',(-0.39018572765941,3.21306033389243E-17,0.920736171729392));
#34591=DIRECTION('',(-7.02566079304691E-17,1.,-6.46696967659226E-17));
#34592=DIRECTION('',(0.342434989471226,-8.79348777081821E-16,0.939541525418564));
#34593=DIRECTION('',(6.78825748670589E-16,1.,6.88522083890673E-16));
#34594=DIRECTION('',(0.342434989471226,-8.79348777081821E-16,0.939541525418564));
#34595=DIRECTION('',(6.78825748670589E-16,1.,6.88522083890673E-16));
#34596=DIRECTION('',(-0.39018572765941,3.21306033389243E-17,0.920736171729392));
#34597=DIRECTION('',(-7.02566079304691E-17,1.,-6.46696967659226E-17));
#34598=DIRECTION('',(-0.39018572765941,3.21306033389243E-17,0.920736171729392));
#34599=DIRECTION('',(-7.02566079304691E-17,1.,-6.46696967659226E-17));
#34600=DIRECTION('',(-0.39018572765941,3.21306033389243E-17,0.920736171729392));
#34601=DIRECTION('',(-7.02566079304691E-17,1.,-6.46696967659226E-17));
#34602=DIRECTION('',(-0.39018572765941,3.21306033389243E-17,0.920736171729392));
#34603=DIRECTION('',(-7.02566079304691E-17,1.,-6.46696967659226E-17));
#34604=DIRECTION('',(-0.39018572765941,3.21306033389243E-17,0.920736171729392));
#34605=DIRECTION('',(-7.02566079304691E-17,1.,-6.46696967659226E-17));
#34606=DIRECTION('',(-0.39018572765941,3.21306033389243E-17,0.920736171729392));
#34607=DIRECTION('',(-7.02566079304691E-17,1.,-6.46696967659226E-17));
#34608=DIRECTION('',(-0.39018572765941,3.21306033389243E-17,0.920736171729392));
#34609=DIRECTION('',(-7.02566079304691E-17,1.,-6.46696967659226E-17));
#34610=DIRECTION('',(-0.39018572765941,3.21306033389243E-17,0.920736171729392));
#34611=DIRECTION('',(-7.02566079304691E-17,1.,-6.46696967659226E-17));
#34612=DIRECTION('',(-0.39018572765941,3.21306033389243E-17,0.920736171729392));
#34613=DIRECTION('',(-7.02566079304691E-17,1.,-6.46696967659226E-17));
#34614=DIRECTION('',(-0.39018572765941,3.21306033389243E-17,0.920736171729392));
#34615=DIRECTION('',(-7.02566079304691E-17,1.,-6.46696967659226E-17));
#34616=DIRECTION('',(-0.39018572765941,3.21306033389243E-17,0.920736171729392));
#34617=DIRECTION('',(-7.02566079304691E-17,1.,-6.46696967659226E-17));
#34618=DIRECTION('',(-0.39018572765941,3.21306033389243E-17,0.920736171729392));
#34619=DIRECTION('',(-7.02566079304691E-17,1.,-6.46696967659226E-17));
#34620=DIRECTION('',(-0.39018572765941,3.21306033389243E-17,0.920736171729392));
#34621=DIRECTION('',(-7.02566079304691E-17,1.,-6.46696967659226E-17));
#34622=DIRECTION('',(-0.39018572765941,3.21306033389243E-17,0.920736171729392));
#34623=DIRECTION('',(-7.02566079304691E-17,1.,-6.46696967659226E-17));
#34624=DIRECTION('',(-0.39018572765941,3.21306033389243E-17,0.920736171729392));
#34625=DIRECTION('',(-7.02566079304691E-17,1.,-6.46696967659226E-17));
#34626=DIRECTION('',(0.308210063472299,0.951318325679896,-1.39626245472703E-16));
#34627=DIRECTION('',(-1.83620234923647E-16,-8.72816584845505E-17,-1.));
#34628=DIRECTION('',(-0.951318325679897,0.308210063472296,7.16088563108324E-17));
#34629=DIRECTION('',(-1.34762946440481E-16,-1.83620234923647E-16,-1.));
#34630=DIRECTION('',(-0.308210063472293,-0.951318325679898,1.40045238088457E-16));
#34631=DIRECTION('',(-3.8424370001384E-17,-1.3476294644048E-16,-1.));
#34632=CARTESIAN_POINT('',(0.,0.,0.));
#34633=CARTESIAN_POINT('',(0.,0.,0.));
#34634=CARTESIAN_POINT('Origin',(-12.5,160.5,7.5));
#34635=CARTESIAN_POINT('',(-15.5,160.5,-7.5));
#34636=CARTESIAN_POINT('Origin',(-12.5,160.5,-7.5));
#34637=CARTESIAN_POINT('',(-15.5,160.5,7.5));
#34638=CARTESIAN_POINT('',(-15.5,160.5,7.5));
#34639=CARTESIAN_POINT('Origin',(-12.5,160.5,7.5));
#34640=CARTESIAN_POINT('Origin',(12.5,160.5,7.5));
#34641=CARTESIAN_POINT('',(9.50000000000003,160.5,-7.5));
#34642=CARTESIAN_POINT('Origin',(12.5,160.5,-7.5));
#34643=CARTESIAN_POINT('',(9.50000000000003,160.5,7.5));
#34644=CARTESIAN_POINT('',(9.50000000000003,160.5,7.5));
#34645=CARTESIAN_POINT('Origin',(12.5,160.5,7.5));
#34646=CARTESIAN_POINT('Origin',(-12.5,-190.,7.5));
#34647=CARTESIAN_POINT('',(-15.5,-190.,-7.5));
#34648=CARTESIAN_POINT('Origin',(-12.5,-190.,-7.5));
#34649=CARTESIAN_POINT('',(-15.5,-190.,7.5));
#34650=CARTESIAN_POINT('',(-15.5,-190.,7.5));
#34651=CARTESIAN_POINT('Origin',(-12.5,-190.,7.5));
#34652=CARTESIAN_POINT('Origin',(12.5,-190.,7.5));
#34653=CARTESIAN_POINT('',(9.50000000000003,-190.,-7.5));
#34654=CARTESIAN_POINT('Origin',(12.5,-190.,-7.5));
#34655=CARTESIAN_POINT('',(9.50000000000003,-190.,7.5));
#34656=CARTESIAN_POINT('',(9.50000000000003,-190.,7.5));
#34657=CARTESIAN_POINT('Origin',(12.5,-190.,7.5));
#34658=CARTESIAN_POINT('Origin',(-26.,160.5,7.5));
#34659=CARTESIAN_POINT('',(-29.4,160.5,-7.5));
#34660=CARTESIAN_POINT('Origin',(-26.,160.5,-7.5));
#34661=CARTESIAN_POINT('',(-29.4,160.5,7.5));
#34662=CARTESIAN_POINT('',(-29.4,160.5,7.5));
#34663=CARTESIAN_POINT('Origin',(-26.,160.5,7.5));
#34664=CARTESIAN_POINT('Origin',(26.,160.5,7.5));
#34665=CARTESIAN_POINT('',(22.6,160.5,-7.5));
#34666=CARTESIAN_POINT('Origin',(26.,160.5,-7.5));
#34667=CARTESIAN_POINT('',(22.6,160.5,7.5));
#34668=CARTESIAN_POINT('',(22.6,160.5,7.5));
#34669=CARTESIAN_POINT('Origin',(26.,160.5,7.5));
#34670=CARTESIAN_POINT('Origin',(-26.,-190.,7.5));
#34671=CARTESIAN_POINT('',(-29.4,-190.,-7.5));
#34672=CARTESIAN_POINT('Origin',(-26.,-190.,-7.5));
#34673=CARTESIAN_POINT('',(-29.4,-190.,7.5));
#34674=CARTESIAN_POINT('',(-29.4,-190.,7.5));
#34675=CARTESIAN_POINT('Origin',(-26.,-190.,7.5));
#34676=CARTESIAN_POINT('Origin',(26.,-190.,7.5));
#34677=CARTESIAN_POINT('',(22.6,-190.,-7.5));
#34678=CARTESIAN_POINT('Origin',(26.,-190.,-7.5));
#34679=CARTESIAN_POINT('',(22.6,-190.,7.5));
#34680=CARTESIAN_POINT('',(22.6,-190.,7.5));
#34681=CARTESIAN_POINT('Origin',(26.,-190.,7.5));
#34682=CARTESIAN_POINT('Origin',(-10.,260.,-6.93889390390723E-15));
#34683=CARTESIAN_POINT('',(-10.,250.,-3.));
#34684=CARTESIAN_POINT('Origin',(-10.,250.,-6.93889390390723E-15));
#34685=CARTESIAN_POINT('',(-10.,260.,-3.));
#34686=CARTESIAN_POINT('',(-10.,260.,-3.));
#34687=CARTESIAN_POINT('Origin',(-10.,260.,-6.93889390390723E-15));
#34688=CARTESIAN_POINT('Origin',(-10.,250.,-6.93889390390723E-15));
#34689=CARTESIAN_POINT('',(-10.,248.197418142917,-6.93889390390723E-15));
#34690=CARTESIAN_POINT('',(-10.,250.,-3.));
#34691=CARTESIAN_POINT('Origin',(10.,260.,-6.93889390390723E-15));
#34692=CARTESIAN_POINT('',(10.,250.,-3.));
#34693=CARTESIAN_POINT('Origin',(10.,250.,-6.93889390390723E-15));
#34694=CARTESIAN_POINT('',(10.,260.,-3.));
#34695=CARTESIAN_POINT('',(10.,260.,-3.));
#34696=CARTESIAN_POINT('Origin',(10.,260.,-6.93889390390723E-15));
#34697=CARTESIAN_POINT('Origin',(10.,250.,-6.93889390390723E-15));
#34698=CARTESIAN_POINT('',(9.99999999999999,248.197418142917,-6.93889390390723E-15));
#34699=CARTESIAN_POINT('',(10.,250.,-3.));
#34700=CARTESIAN_POINT('Origin',(-24.,260.,-6.93889390390723E-15));
#34701=CARTESIAN_POINT('',(-24.,243.,-2.5));
#34702=CARTESIAN_POINT('Origin',(-24.,243.,-6.93889390390723E-15));
#34703=CARTESIAN_POINT('',(-24.,260.,-2.5));
#34704=CARTESIAN_POINT('',(-24.,260.,-2.5));
#34705=CARTESIAN_POINT('Origin',(-24.,260.,-6.93889390390723E-15));
#34706=CARTESIAN_POINT('Origin',(-24.,243.,-6.93889390390723E-15));
#34707=CARTESIAN_POINT('',(-24.,241.497848452431,-6.93889390390723E-15));
#34708=CARTESIAN_POINT('',(-24.,243.,-2.5));
#34709=CARTESIAN_POINT('Origin',(24.,260.,-6.93889390390723E-15));
#34710=CARTESIAN_POINT('',(24.,243.,-2.5));
#34711=CARTESIAN_POINT('Origin',(24.,243.,-6.93889390390723E-15));
#34712=CARTESIAN_POINT('',(24.,260.,-2.5));
#34713=CARTESIAN_POINT('',(24.,260.,-2.5));
#34714=CARTESIAN_POINT('Origin',(24.,260.,-6.93889390390723E-15));
#34715=CARTESIAN_POINT('Origin',(24.,243.,-6.93889390390723E-15));
#34716=CARTESIAN_POINT('',(24.,241.497848452431,-6.93889390390723E-15));
#34717=CARTESIAN_POINT('',(24.,243.,-2.5));
#34718=CARTESIAN_POINT('Origin',(-150.,-260.,7.5));
#34719=CARTESIAN_POINT('',(-150.,-260.,-7.5));
#34720=CARTESIAN_POINT('',(-90.,-260.,-7.5));
#34721=CARTESIAN_POINT('',(-150.,-260.,-7.5));
#34722=CARTESIAN_POINT('',(-90.,-260.,7.5));
#34723=CARTESIAN_POINT('',(-90.,-260.,-7.5));
#34724=CARTESIAN_POINT('',(-150.,-260.,7.5));
#34725=CARTESIAN_POINT('',(-150.,-260.,7.5));
#34726=CARTESIAN_POINT('',(-150.,-260.,7.5));
#34727=CARTESIAN_POINT('Origin',(150.,-260.,7.5));
#34728=CARTESIAN_POINT('',(150.,-260.,-7.5));
#34729=CARTESIAN_POINT('',(150.,260.,-7.5));
#34730=CARTESIAN_POINT('',(150.,-260.,-7.5));
#34731=CARTESIAN_POINT('',(150.,260.,7.5));
#34732=CARTESIAN_POINT('',(150.,260.,7.5));
#34733=CARTESIAN_POINT('',(150.,-260.,7.5));
#34734=CARTESIAN_POINT('',(150.,-260.,7.5));
#34735=CARTESIAN_POINT('',(150.,-260.,7.5));
#34736=CARTESIAN_POINT('Origin',(-150.,260.,7.5));
#34737=CARTESIAN_POINT('',(-150.,260.,-7.5));
#34738=CARTESIAN_POINT('',(-150.,260.,-7.5));
#34739=CARTESIAN_POINT('',(-150.,260.,7.5));
#34740=CARTESIAN_POINT('',(-150.,260.,7.5));
#34741=CARTESIAN_POINT('',(-150.,260.,7.5));
#34742=CARTESIAN_POINT('Origin',(-150.,-260.,7.5));
#34743=CARTESIAN_POINT('',(-150.,-260.,-7.5));
#34744=CARTESIAN_POINT('',(-150.,-260.,7.5));
#34745=CARTESIAN_POINT('Origin',(-150.,-260.,7.5));
#34746=CARTESIAN_POINT('',(90.,-260.,7.5));
#34747=CARTESIAN_POINT('',(-150.,-260.,7.5));
#34748=CARTESIAN_POINT('',(90.,-260.,-7.5));
#34749=CARTESIAN_POINT('',(90.,-260.,-7.5));
#34750=CARTESIAN_POINT('',(-150.,-260.,-7.5));
#34751=CARTESIAN_POINT('Origin',(0.,0.,7.5));
#34752=CARTESIAN_POINT('',(-90.,-210.,7.5));
#34753=CARTESIAN_POINT('',(-90.,-210.,7.5));
#34754=CARTESIAN_POINT('',(90.,-210.,7.5));
#34755=CARTESIAN_POINT('',(-90.,-210.,7.5));
#34756=CARTESIAN_POINT('',(90.,-210.,7.5));
#34757=CARTESIAN_POINT('Origin',(0.,0.,-7.5));
#34758=CARTESIAN_POINT('',(-90.,-210.,-7.5));
#34759=CARTESIAN_POINT('',(-90.,-210.,-7.5));
#34760=CARTESIAN_POINT('',(90.,-210.,-7.5));
#34761=CARTESIAN_POINT('',(90.,-210.,-7.5));
#34762=CARTESIAN_POINT('',(-90.,-210.,-7.5));
#34763=CARTESIAN_POINT('Origin',(-90.,-210.,-7.5));
#34764=CARTESIAN_POINT('',(-90.,-210.,-7.5));
#34765=CARTESIAN_POINT('Origin',(-90.,-210.,-7.5));
#34766=CARTESIAN_POINT('',(90.,-210.,-7.5));
#34767=CARTESIAN_POINT('Origin',(90.,-210.,-7.5));
#34768=CARTESIAN_POINT('',(0.,0.,0.));
#34769=CARTESIAN_POINT('',(0.,0.,0.));
#34770=CARTESIAN_POINT('',(0.,0.,0.));
#34771=CARTESIAN_POINT('Origin',(-7.49999999999999,0.,0.));
#34772=CARTESIAN_POINT('',(385.2,-6.12323399573687E-16,-5.00000000000009));
#34773=CARTESIAN_POINT('Origin',(385.2,0.,0.));
#34774=CARTESIAN_POINT('',(399.5,-6.12323399573687E-16,-5.00000000000009));
#34775=CARTESIAN_POINT('',(-7.49999999999999,-6.12323399573687E-16,-5.00000000000009));
#34776=CARTESIAN_POINT('',(399.5,-1.5,4.76969600708481));
#34777=CARTESIAN_POINT('Origin',(399.5,0.,0.));
#34778=CARTESIAN_POINT('',(389.5,-1.5,4.76969600708482));
#34779=CARTESIAN_POINT('',(-7.49999999999999,-1.5,4.76969600708482));
#34780=CARTESIAN_POINT('',(389.5,1.5,4.76969600708482));
#34781=CARTESIAN_POINT('Ctrl Pts',(389.5,1.5,4.76969600708482));
#34782=CARTESIAN_POINT('Ctrl Pts',(389.310361373005,1.5,4.76969600708482));
#34783=CARTESIAN_POINT('Ctrl Pts',(389.108946257286,1.46186045804959,4.78218969528753));
#34784=CARTESIAN_POINT('Ctrl Pts',(388.739762231142,1.30843336307885,4.82642478051612));
#34785=CARTESIAN_POINT('Ctrl Pts',(388.571882312748,1.19320265630731,4.85743375864517));
#34786=CARTESIAN_POINT('Ctrl Pts',(388.306836828799,0.928157172358542,4.914967813075));
#34787=CARTESIAN_POINT('Ctrl Pts',(388.191575546484,0.760261209503116,4.94535597495049));
#34788=CARTESIAN_POINT('Ctrl Pts',(388.038125876745,0.391018858740931,4.98815066693925));
#34789=CARTESIAN_POINT('Ctrl Pts',(388.,0.189582132646001,5.00000000000009));
#34790=CARTESIAN_POINT('Ctrl Pts',(388.,-0.189582132646003,5.00000000000009));
#34791=CARTESIAN_POINT('Ctrl Pts',(388.038125876745,-0.391018858740932,
4.98815066693925));
#34792=CARTESIAN_POINT('Ctrl Pts',(388.191575546484,-0.760261209503118,
4.94535597495048));
#34793=CARTESIAN_POINT('Ctrl Pts',(388.306836828799,-0.928157172358544,
4.914967813075));
#34794=CARTESIAN_POINT('Ctrl Pts',(388.571882312748,-1.19320265630731,4.85743375864517));
#34795=CARTESIAN_POINT('Ctrl Pts',(388.739762231142,-1.30843336307885,4.82642478051612));
#34796=CARTESIAN_POINT('Ctrl Pts',(389.108946257286,-1.4618604580496,4.78218969528753));
#34797=CARTESIAN_POINT('Ctrl Pts',(389.310361373005,-1.5,4.76969600708482));
#34798=CARTESIAN_POINT('Ctrl Pts',(389.5,-1.5,4.76969600708482));
#34799=CARTESIAN_POINT('',(399.5,1.5,4.76969600708481));
#34800=CARTESIAN_POINT('',(-7.49999999999999,1.5,4.76969600708482));
#34801=CARTESIAN_POINT('Origin',(399.5,0.,0.));
#34802=CARTESIAN_POINT('Origin',(385.2,0.,0.));
#34803=CARTESIAN_POINT('',(385.,-6.36816335556636E-16,-5.2000000000001));
#34804=CARTESIAN_POINT('Origin',(385.,0.,0.));
#34805=CARTESIAN_POINT('Origin',(385.2,-6.36816335556636E-16,-5.2000000000001));
#34806=CARTESIAN_POINT('Origin',(385.,0.,0.));
#34807=CARTESIAN_POINT('',(384.5,-7.34788079488421E-16,-6.00000000000007));
#34808=CARTESIAN_POINT('Origin',(384.5,0.,0.));
#34809=CARTESIAN_POINT('',(385.,-6.73555739531045E-16,-5.50000000000001));
#34810=CARTESIAN_POINT('',(385.,-6.73555739531045E-16,-5.50000000000001));
#34811=CARTESIAN_POINT('Origin',(385.,0.,0.));
#34812=CARTESIAN_POINT('Origin',(-7.49999999999999,0.,0.));
#34813=CARTESIAN_POINT('',(346.3,-7.34788079488418E-16,-6.00000000000005));
#34814=CARTESIAN_POINT('Origin',(346.3,0.,0.));
#34815=CARTESIAN_POINT('',(-7.49999999999999,-7.34788079488418E-16,-6.00000000000005));
#34816=CARTESIAN_POINT('Origin',(346.3,0.,0.));
#34817=CARTESIAN_POINT('',(346.,-7.71527483462834E-16,-6.30000000000001));
#34818=CARTESIAN_POINT('Origin',(346.,0.,0.));
#34819=CARTESIAN_POINT('Origin',(346.3,-7.71527483462834E-16,-6.30000000000001));
#34820=CARTESIAN_POINT('Origin',(346.,0.,0.));
#34821=CARTESIAN_POINT('',(345.5,-9.18485099360533E-16,-7.50000000000014));
#34822=CARTESIAN_POINT('Origin',(345.5,0.,0.));
#34823=CARTESIAN_POINT('',(346.,-8.57252759403155E-16,-7.00000000000006));
#34824=CARTESIAN_POINT('',(346.,-8.57252759403155E-16,-7.00000000000006));
#34825=CARTESIAN_POINT('Origin',(346.,0.,0.));
#34826=CARTESIAN_POINT('Origin',(-7.49999999999999,0.,0.));
#34827=CARTESIAN_POINT('',(11.5,9.18485099360514E-16,7.49999999999999));
#34828=CARTESIAN_POINT('',(11.5,-9.1848509936052E-16,-7.50000000000004));
#34829=CARTESIAN_POINT('Origin',(11.5,0.,0.));
#34830=CARTESIAN_POINT('Origin',(11.5,0.,0.));
#34831=CARTESIAN_POINT('',(-7.49999999999999,-9.1848509936052E-16,-7.50000000000004));
#34832=CARTESIAN_POINT('Origin',(11.5,0.,0.));
#34833=CARTESIAN_POINT('',(11.,-8.5725275940315E-16,7.00000000000002));
#34834=CARTESIAN_POINT('',(11.5,-9.18485099360514E-16,7.49999999999999));
#34835=CARTESIAN_POINT('Origin',(11.,0.,0.));
#34836=CARTESIAN_POINT('Origin',(10.7,0.,0.));
#34837=CARTESIAN_POINT('',(10.7,-6.12323399573677E-16,-5.));
#34838=CARTESIAN_POINT('Origin',(10.7,0.,0.));
#34839=CARTESIAN_POINT('',(11.,-6.49062803548097E-16,-5.3));
#34840=CARTESIAN_POINT('Origin',(10.7,-6.49062803548097E-16,-5.3));
#34841=CARTESIAN_POINT('Origin',(11.,0.,0.));
#34842=CARTESIAN_POINT('Origin',(-7.49999999999999,0.,0.));
#34843=CARTESIAN_POINT('',(3.00000000000001,-6.12323399573677E-16,-5.));
#34844=CARTESIAN_POINT('Origin',(3.00000000000001,0.,0.));
#34845=CARTESIAN_POINT('',(-7.49999999999999,-6.12323399573677E-16,-5.));
#34846=CARTESIAN_POINT('Origin',(-7.49999999999999,0.,0.));
#34847=CARTESIAN_POINT('',(1.85000000000001,-5.87830463590729E-16,-4.8));
#34848=CARTESIAN_POINT('Origin',(1.85000000000001,0.,0.));
#34849=CARTESIAN_POINT('',(3.00000000000001,-5.87830463590729E-16,-4.8));
#34850=CARTESIAN_POINT('',(-7.49999999999999,-5.87830463590729E-16,-4.8));
#34851=CARTESIAN_POINT('Origin',(3.00000000000001,0.,0.));
#34852=CARTESIAN_POINT('Origin',(-7.49999999999999,0.,0.));
#34853=CARTESIAN_POINT('',(0.5,6.12323399573677E-16,5.));
#34854=CARTESIAN_POINT('',(0.5,-6.12323399573677E-16,-5.));
#34855=CARTESIAN_POINT('Origin',(0.5,0.,0.));
#34856=CARTESIAN_POINT('Origin',(0.5,0.,0.));
#34857=CARTESIAN_POINT('',(1.85000000000001,-6.12323399573677E-16,-5.));
#34858=CARTESIAN_POINT('',(-7.49999999999999,-6.12323399573677E-16,-5.));
#34859=CARTESIAN_POINT('Origin',(1.85000000000001,0.,0.));
#34860=CARTESIAN_POINT('Origin',(0.5,0.,0.));
#34861=CARTESIAN_POINT('',(6.93889390390723E-17,-5.51091059616313E-16,4.50000000000003));
#34862=CARTESIAN_POINT('',(0.5,-6.12323399573677E-16,5.));
#34863=CARTESIAN_POINT('Origin',(0.,0.,0.));
#34864=CARTESIAN_POINT('Origin',(1.85000000000001,5.,0.));
#34865=CARTESIAN_POINT('Origin',(3.00000000000001,5.,0.));
#34866=CARTESIAN_POINT('Origin',(11.,7.00000000000002,0.));
#34867=CARTESIAN_POINT('Origin',(346.,6.30000000000001,0.));
#34868=CARTESIAN_POINT('Origin',(385.,5.2000000000001,0.));
#34869=CARTESIAN_POINT('Origin',(400.,0.,0.));
#34870=CARTESIAN_POINT('',(400.,1.5,4.24264068711934));
#34871=CARTESIAN_POINT('Ctrl Pts',(399.5,1.5,4.76969600708481));
#34872=CARTESIAN_POINT('Ctrl Pts',(399.66715123186,1.5,4.59447390528654));
#34873=CARTESIAN_POINT('Ctrl Pts',(399.833884933644,1.5,4.41883232193548));
#34874=CARTESIAN_POINT('Ctrl Pts',(400.,1.5,4.24264068711934));
#34875=CARTESIAN_POINT('',(400.,-1.5,4.24264068711934));
#34876=CARTESIAN_POINT('Origin',(400.,0.,0.));
#34877=CARTESIAN_POINT('Ctrl Pts',(400.,-1.5,4.24264068711934));
#34878=CARTESIAN_POINT('Ctrl Pts',(399.833876215866,-1.5,4.41884156853607));
#34879=CARTESIAN_POINT('Ctrl Pts',(399.667149605032,-1.5,4.59447561066608));
#34880=CARTESIAN_POINT('Ctrl Pts',(399.5,-1.5,4.76969600708481));
#34881=CARTESIAN_POINT('Origin',(400.,0.,0.));
#34882=CARTESIAN_POINT('',(400.,1.5,3.2));
#34883=CARTESIAN_POINT('',(400.,1.5,5.));
#34884=CARTESIAN_POINT('',(400.,-1.5,3.2));
#34885=CARTESIAN_POINT('',(400.,1.5,3.2));
#34886=CARTESIAN_POINT('',(400.,-1.5,-3.61400724161835E-16));
#34887=CARTESIAN_POINT('Origin',(2.14313189850789E-16,4.50000000000003,
0.));
#34888=CARTESIAN_POINT('Origin',(388.,1.5,5.));
#34889=CARTESIAN_POINT('',(389.5,1.5,3.2));
#34890=CARTESIAN_POINT('',(389.5,1.5,5.));
#34891=CARTESIAN_POINT('',(388.,1.5,3.2));
#34892=CARTESIAN_POINT('Origin',(388.,-1.5,5.));
#34893=CARTESIAN_POINT('',(389.5,-1.5,3.2));
#34894=CARTESIAN_POINT('',(388.,-1.5,3.2));
#34895=CARTESIAN_POINT('',(389.5,-1.5,5.));
#34896=CARTESIAN_POINT('Origin',(388.,1.5,3.2));
#34897=CARTESIAN_POINT('Origin',(389.5,-6.50521303491303E-16,3.2));
#34898=CARTESIAN_POINT('Origin',(389.5,-6.50521303491303E-16,0.));
#34899=CARTESIAN_POINT('',(0.,0.,0.));
#34900=CARTESIAN_POINT('Origin',(5.,22.1731087802709,9.18440237676217));
#34901=CARTESIAN_POINT('',(5.,7.48707131916463,0.440185258433775));
#34902=CARTESIAN_POINT('Ctrl Pts',(5.,7.48707131916463,0.440185258433775));
#34903=CARTESIAN_POINT('Ctrl Pts',(4.68873581543082,7.48707131916463,0.440185258433775));
#34904=CARTESIAN_POINT('Ctrl Pts',(4.35845534789624,7.48402338137256,0.506766716239049));
#34905=CARTESIAN_POINT('Ctrl Pts',(3.75350716939841,7.46156020953612,0.769764179262972));
#34906=CARTESIAN_POINT('Ctrl Pts',(3.47861587184941,7.44093225812105,0.965560498093768));
#34907=CARTESIAN_POINT('Ctrl Pts',(3.04463387982388,7.3703917706363,1.40608039471696));
#34908=CARTESIAN_POINT('Ctrl Pts',(2.85577540978026,7.31555987078622,1.68094905379426));
#34909=CARTESIAN_POINT('Ctrl Pts',(2.60414734335626,7.15493061203946,2.26935538845465));
#34910=CARTESIAN_POINT('Ctrl Pts',(2.54150000000001,7.04816066352038,2.5826794094902));
#34911=CARTESIAN_POINT('Ctrl Pts',(2.54150000000001,6.81003232414892,3.15757207598616));
#34912=CARTESIAN_POINT('Ctrl Pts',(2.60414734335626,6.66397653879082,3.45462337059381));
#34913=CARTESIAN_POINT('Ctrl Pts',(2.85577540978025,6.36149246757615,3.9842715180421));
#34914=CARTESIAN_POINT('Ctrl Pts',(3.04463387982388,6.20590298301627,4.21740501902064));
#34915=CARTESIAN_POINT('Ctrl Pts',(3.47861587184941,5.94428803391508,4.57877928221917));
#34916=CARTESIAN_POINT('Ctrl Pts',(3.75350716939841,5.82042529346604,4.73181435132337));
#34917=CARTESIAN_POINT('Ctrl Pts',(4.35845534789624,5.65034186505947,4.93366550199495));
#34918=CARTESIAN_POINT('Ctrl Pts',(4.68873581543082,5.60541688222548,4.98290091979175));
#34919=CARTESIAN_POINT('Ctrl Pts',(5.31126418456918,5.60541688222548,4.98290091979175));
#34920=CARTESIAN_POINT('Ctrl Pts',(5.64154465210376,5.65034186505947,4.93366550199495));
#34921=CARTESIAN_POINT('Ctrl Pts',(6.24649283060159,5.82042529346604,4.73181435132337));
#34922=CARTESIAN_POINT('Ctrl Pts',(6.52138412815059,5.94428803391508,4.57877928221917));
#34923=CARTESIAN_POINT('Ctrl Pts',(6.95536612017612,6.20590298301627,4.21740501902064));
#34924=CARTESIAN_POINT('Ctrl Pts',(7.14422459021974,6.36149246757615,3.9842715180421));
#34925=CARTESIAN_POINT('Ctrl Pts',(7.39585265664374,6.66397653879082,3.45462337059381));
#34926=CARTESIAN_POINT('Ctrl Pts',(7.45849999999999,6.81003232414892,3.15757207598616));
#34927=CARTESIAN_POINT('Ctrl Pts',(7.45849999999999,7.04816066352038,2.5826794094902));
#34928=CARTESIAN_POINT('Ctrl Pts',(7.39585265664374,7.15493061203946,2.26935538845465));
#34929=CARTESIAN_POINT('Ctrl Pts',(7.14422459021974,7.31555987078622,1.68094905379426));
#34930=CARTESIAN_POINT('Ctrl Pts',(6.95536612017612,7.3703917706363,1.40608039471696));
#34931=CARTESIAN_POINT('Ctrl Pts',(6.52138412815059,7.44093225812105,0.965560498093769));
#34932=CARTESIAN_POINT('Ctrl Pts',(6.24649283060159,7.46156020953611,0.769764179262975));
#34933=CARTESIAN_POINT('Ctrl Pts',(5.64154465210376,7.48402338137256,0.506766716239051));
#34934=CARTESIAN_POINT('Ctrl Pts',(5.31126418456918,7.48707131916463,0.440185258433775));
#34935=CARTESIAN_POINT('Ctrl Pts',(5.,7.48707131916463,0.440185258433775));
#34936=CARTESIAN_POINT('',(5.,22.9972930864807,6.86472946987049));
#34937=CARTESIAN_POINT('',(5.,23.1139359987404,6.91304454608318));
#34938=CARTESIAN_POINT('Ctrl Pts',(5.,22.9972930864807,6.86472946987049));
#34939=CARTESIAN_POINT('Ctrl Pts',(5.30892798186098,22.9972930864807,6.86472946987049));
#34940=CARTESIAN_POINT('Ctrl Pts',(5.63829853703008,22.9797603253307,6.92434139206246));
#34941=CARTESIAN_POINT('Ctrl Pts',(6.24395747678749,22.9057609106853,7.16533358286599));
#34942=CARTESIAN_POINT('Ctrl Pts',(6.52026442354922,22.8489771609384,7.34656970696721));
#34943=CARTESIAN_POINT('Ctrl Pts',(6.95657880152062,22.7112821636813,7.76179785122406));
#34944=CARTESIAN_POINT('Ctrl Pts',(7.1457499860634,22.6211168109853,8.02352301118618));
#34945=CARTESIAN_POINT('Ctrl Pts',(7.39671656426829,22.4112998779956,8.59217580499353));
#34946=CARTESIAN_POINT('Ctrl Pts',(7.45849999999999,22.2913299574281,8.89899120750958));
#34947=CARTESIAN_POINT('Ctrl Pts',(7.45849999999999,22.0548876031137,9.46981354601478));
#34948=CARTESIAN_POINT('Ctrl Pts',(7.39671656426829,21.9227678957938,9.77159634207808));
#34949=CARTESIAN_POINT('Ctrl Pts',(7.1457499860634,21.6690326252767,10.3220575648447));
#34950=CARTESIAN_POINT('Ctrl Pts',(6.95657880152062,21.5477215221798,10.5708817325805));
#34951=CARTESIAN_POINT('Ctrl Pts',(6.52026442354922,21.3514759519323,10.9618574354199));
#34952=CARTESIAN_POINT('Ctrl Pts',(6.24395747678748,21.2634748340916,11.1301629022752));
#34953=CARTESIAN_POINT('Ctrl Pts',(5.63829853703008,21.1453931096609,11.3528956025049));
#34954=CARTESIAN_POINT('Ctrl Pts',(5.30892798186098,21.1156386495415,11.4074451312285));
#34955=CARTESIAN_POINT('Ctrl Pts',(4.69107201813902,21.1156386495415,11.4074451312285));
#34956=CARTESIAN_POINT('Ctrl Pts',(4.36170146296992,21.1453931096609,11.3528956025049));
#34957=CARTESIAN_POINT('Ctrl Pts',(3.75604252321252,21.2634748340916,11.1301629022752));
#34958=CARTESIAN_POINT('Ctrl Pts',(3.47973557645078,21.3514759519323,10.9618574354199));
#34959=CARTESIAN_POINT('Ctrl Pts',(3.04342119847938,21.5477215221798,10.5708817325805));
#34960=CARTESIAN_POINT('Ctrl Pts',(2.8542500139366,21.6690326252767,10.3220575648447));
#34961=CARTESIAN_POINT('Ctrl Pts',(2.60328343573171,21.9227678957938,9.77159634207808));
#34962=CARTESIAN_POINT('Ctrl Pts',(2.54150000000001,22.0548876031137,9.46981354601477));
#34963=CARTESIAN_POINT('Ctrl Pts',(2.54150000000001,22.2913299574281,8.89899120750958));
#34964=CARTESIAN_POINT('Ctrl Pts',(2.60328343573171,22.4112998779956,8.59217580499353));
#34965=CARTESIAN_POINT('Ctrl Pts',(2.85425001393659,22.6211168109853,8.02352301118618));
#34966=CARTESIAN_POINT('Ctrl Pts',(3.04342119847938,22.7112821636813,7.76179785122406));
#34967=CARTESIAN_POINT('Ctrl Pts',(3.47973557645078,22.8489771609384,7.34656970696721));
#34968=CARTESIAN_POINT('Ctrl Pts',(3.75604252321252,22.9057609106853,7.16533358286599));
#34969=CARTESIAN_POINT('Ctrl Pts',(4.36170146296993,22.9797603253307,6.92434139206246));
#34970=CARTESIAN_POINT('Ctrl Pts',(4.69107201813902,22.9972930864807,6.86472946987049));
#34971=CARTESIAN_POINT('Ctrl Pts',(5.,22.9972930864807,6.86472946987049));
#34972=CARTESIAN_POINT('Origin',(10.,13.4350288425444,-13.4350288425444));
#34973=CARTESIAN_POINT('',(0.,13.4350288425444,-10.6850288425444));
#34974=CARTESIAN_POINT('Origin',(0.,13.4350288425444,-13.4350288425444));
#34975=CARTESIAN_POINT('',(10.,13.4350288425444,-10.6850288425444));
#34976=CARTESIAN_POINT('',(10.,13.4350288425444,-10.6850288425444));
#34977=CARTESIAN_POINT('Origin',(10.,13.4350288425444,-13.4350288425444));
#34978=CARTESIAN_POINT('Origin',(10.,19.,0.));
#34979=CARTESIAN_POINT('',(0.,19.,2.74999999999999));
#34980=CARTESIAN_POINT('Origin',(0.,19.,0.));
#34981=CARTESIAN_POINT('',(10.,19.,2.74999999999999));
#34982=CARTESIAN_POINT('',(10.,19.,2.74999999999999));
#34983=CARTESIAN_POINT('Origin',(10.,19.,0.));
#34984=CARTESIAN_POINT('Origin',(10.,13.4350288425444,13.4350288425444));
#34985=CARTESIAN_POINT('',(0.,13.4350288425444,16.1850288425444));
#34986=CARTESIAN_POINT('Origin',(0.,13.4350288425444,13.4350288425444));
#34987=CARTESIAN_POINT('',(10.,13.4350288425444,16.1850288425444));
#34988=CARTESIAN_POINT('',(10.,13.4350288425444,16.1850288425444));
#34989=CARTESIAN_POINT('Origin',(10.,13.4350288425444,13.4350288425444));
#34990=CARTESIAN_POINT('Origin',(10.,-13.4350288425444,13.4350288425444));
#34991=CARTESIAN_POINT('',(0.,-13.4350288425444,16.1850288425444));
#34992=CARTESIAN_POINT('Origin',(0.,-13.4350288425444,13.4350288425444));
#34993=CARTESIAN_POINT('',(10.,-13.4350288425444,16.1850288425444));
#34994=CARTESIAN_POINT('',(10.,-13.4350288425444,16.1850288425444));
#34995=CARTESIAN_POINT('Origin',(10.,-13.4350288425444,13.4350288425444));
#34996=CARTESIAN_POINT('Origin',(10.,-19.,0.));
#34997=CARTESIAN_POINT('',(0.,-19.,2.74999999999999));
#34998=CARTESIAN_POINT('Origin',(0.,-19.,0.));
#34999=CARTESIAN_POINT('',(10.,-19.,2.74999999999999));
#35000=CARTESIAN_POINT('',(10.,-19.,2.74999999999999));
#35001=CARTESIAN_POINT('Origin',(10.,-19.,0.));
#35002=CARTESIAN_POINT('Origin',(10.,-13.4350288425444,-13.4350288425444));
#35003=CARTESIAN_POINT('',(0.,-13.4350288425444,-10.6850288425444));
#35004=CARTESIAN_POINT('Origin',(0.,-13.4350288425444,-13.4350288425444));
#35005=CARTESIAN_POINT('',(10.,-13.4350288425444,-10.6850288425444));
#35006=CARTESIAN_POINT('',(10.,-13.4350288425444,-10.6850288425444));
#35007=CARTESIAN_POINT('Origin',(10.,-13.4350288425444,-13.4350288425444));
#35008=CARTESIAN_POINT('Origin',(-34.1076474136955,0.,0.));
#35009=CARTESIAN_POINT('',(-31.5,-1.71450551880629E-15,-14.));
#35010=CARTESIAN_POINT('Origin',(-31.5,0.,0.));
#35011=CARTESIAN_POINT('',(0.,-1.71450551880629E-15,-14.));
#35012=CARTESIAN_POINT('',(-34.1076474136955,-1.71450551880629E-15,-14.));
#35013=CARTESIAN_POINT('Origin',(0.,0.,0.));
#35014=CARTESIAN_POINT('Origin',(-34.1076474136955,0.,0.));
#35015=CARTESIAN_POINT('',(10.,-1.34711147906209E-15,-11.));
#35016=CARTESIAN_POINT('Origin',(10.,0.,0.));
#35017=CARTESIAN_POINT('',(9.5,-1.34711147906209E-15,-11.));
#35018=CARTESIAN_POINT('',(-34.1076474136955,-1.34711147906209E-15,-11.));
#35019=CARTESIAN_POINT('Origin',(9.5,0.,0.));
#35020=CARTESIAN_POINT('Origin',(-34.1076474136955,0.,0.));
#35021=CARTESIAN_POINT('',(9.50000000000001,-1.31649530908341E-15,-10.75));
#35022=CARTESIAN_POINT('Origin',(9.50000000000001,0.,0.));
#35023=CARTESIAN_POINT('',(10.,-1.31649530908341E-15,-10.75));
#35024=CARTESIAN_POINT('',(-34.1076474136955,-1.31649530908341E-15,-10.75));
#35025=CARTESIAN_POINT('Origin',(10.,0.,0.));
#35026=CARTESIAN_POINT('Origin',(-34.1076474136955,0.,0.));
#35027=CARTESIAN_POINT('',(10.,-9.18485099360515E-16,-7.5));
#35028=CARTESIAN_POINT('Origin',(10.,0.,0.));
#35029=CARTESIAN_POINT('',(-32.,-9.18485099360515E-16,-7.5));
#35030=CARTESIAN_POINT('',(-34.1076474136955,-9.18485099360515E-16,-7.5));
#35031=CARTESIAN_POINT('Origin',(-32.,0.,0.));
#35032=CARTESIAN_POINT('Origin',(-34.1076474136955,0.,0.));
#35033=CARTESIAN_POINT('',(-32.,-1.3164953090834E-15,-10.75));
#35034=CARTESIAN_POINT('Origin',(-32.,0.,0.));
#35035=CARTESIAN_POINT('',(-31.5,-1.3164953090834E-15,-10.75));
#35036=CARTESIAN_POINT('',(-34.1076474136955,-1.3164953090834E-15,-10.75));
#35037=CARTESIAN_POINT('Origin',(-31.5,0.,0.));
#35038=CARTESIAN_POINT('Origin',(-34.1076474136955,0.,0.));
#35039=CARTESIAN_POINT('',(-31.5,-1.34711147906209E-15,-11.));
#35040=CARTESIAN_POINT('Origin',(-31.5,0.,0.));
#35041=CARTESIAN_POINT('',(-32.,-1.34711147906209E-15,-11.));
#35042=CARTESIAN_POINT('',(-34.1076474136955,-1.34711147906209E-15,-11.));
#35043=CARTESIAN_POINT('Origin',(-32.,0.,0.));
#35044=CARTESIAN_POINT('Origin',(-31.5,0.,0.));
#35045=CARTESIAN_POINT('',(-32.,-1.65327317884893E-15,-13.5));
#35046=CARTESIAN_POINT('Origin',(-32.,0.,0.));
#35047=CARTESIAN_POINT('Origin',(-31.5,-1.65327317884893E-15,-13.5));
#35048=CARTESIAN_POINT('Origin',(10.,23.,0.));
#35049=CARTESIAN_POINT('',(10.,11.3578166916005,20.));
#35050=CARTESIAN_POINT('',(10.,-11.3578166915893,20.));
#35051=CARTESIAN_POINT('',(10.,24.,20.));
#35052=CARTESIAN_POINT('',(10.,-11.3578166916005,-20.));
#35053=CARTESIAN_POINT('Origin',(10.,0.,0.));
#35054=CARTESIAN_POINT('',(10.,11.3578166916005,-20.));
#35055=CARTESIAN_POINT('',(10.,24.,-20.));
#35056=CARTESIAN_POINT('Origin',(10.,0.,0.));
#35057=CARTESIAN_POINT('Origin',(9.,0.,0.));
#35058=CARTESIAN_POINT('',(9.,-13.2664991614216,20.));
#35059=CARTESIAN_POINT('Ctrl Pts',(9.,-13.2664991614216,20.));
#35060=CARTESIAN_POINT('Ctrl Pts',(9.09995111742602,-13.2664991614216,20.));
#35061=CARTESIAN_POINT('Ctrl Pts',(9.21480544093045,-13.231938929479,20.));
#35062=CARTESIAN_POINT('Ctrl Pts',(9.42146594446646,-13.1132046912743,20.));
#35063=CARTESIAN_POINT('Ctrl Pts',(9.53638021469469,-12.9933163967994,20.));
#35064=CARTESIAN_POINT('Ctrl Pts',(9.7313641110186,-12.7122458236771,20.));
#35065=CARTESIAN_POINT('Ctrl Pts',(9.82490699559395,-12.4864240538002,20.));
#35066=CARTESIAN_POINT('Ctrl Pts',(9.96053133753905,-12.0059148948793,20.));
#35067=CARTESIAN_POINT('Ctrl Pts',(10.,-11.6534080045929,20.));
#35068=CARTESIAN_POINT('Ctrl Pts',(10.,-11.3578166916006,20.));
#35069=CARTESIAN_POINT('',(9.,-13.2664991614216,-20.));
#35070=CARTESIAN_POINT('Origin',(9.,0.,0.));
#35071=CARTESIAN_POINT('Ctrl Pts',(10.,-11.3578166916006,-20.));
#35072=CARTESIAN_POINT('Ctrl Pts',(10.,-11.6534080045929,-20.));
#35073=CARTESIAN_POINT('Ctrl Pts',(9.96053133753905,-12.0059148948793,-20.));
#35074=CARTESIAN_POINT('Ctrl Pts',(9.82490699559395,-12.4864240538002,-20.));
#35075=CARTESIAN_POINT('Ctrl Pts',(9.7313641110186,-12.7122458236771,-20.));
#35076=CARTESIAN_POINT('Ctrl Pts',(9.53638021469469,-12.9933163967994,-20.));
#35077=CARTESIAN_POINT('Ctrl Pts',(9.42146594446646,-13.1132046912743,-20.));
#35078=CARTESIAN_POINT('Ctrl Pts',(9.21480544093045,-13.231938929479,-20.));
#35079=CARTESIAN_POINT('Ctrl Pts',(9.09995111742602,-13.2664991614216,-20.));
#35080=CARTESIAN_POINT('Ctrl Pts',(9.,-13.2664991614216,-20.));
#35081=CARTESIAN_POINT('Origin',(9.,0.,0.));
#35082=CARTESIAN_POINT('',(9.,13.2664991614216,20.));
#35083=CARTESIAN_POINT('Ctrl Pts',(10.,11.3578166916006,20.));
#35084=CARTESIAN_POINT('Ctrl Pts',(10.,11.6534080045929,20.));
#35085=CARTESIAN_POINT('Ctrl Pts',(9.96053133753905,12.0059148948794,20.));
#35086=CARTESIAN_POINT('Ctrl Pts',(9.82490699559395,12.4864240538002,20.));
#35087=CARTESIAN_POINT('Ctrl Pts',(9.7313641110186,12.7122458236771,20.));
#35088=CARTESIAN_POINT('Ctrl Pts',(9.53638021469469,12.9933163967994,20.));
#35089=CARTESIAN_POINT('Ctrl Pts',(9.42146594446646,13.1132046912743,20.));
#35090=CARTESIAN_POINT('Ctrl Pts',(9.21480544093045,13.231938929479,20.));
#35091=CARTESIAN_POINT('Ctrl Pts',(9.09995111742602,13.2664991614216,20.));
#35092=CARTESIAN_POINT('Ctrl Pts',(9.,13.2664991614216,20.));
#35093=CARTESIAN_POINT('',(9.,13.2664991614216,-20.));
#35094=CARTESIAN_POINT('Ctrl Pts',(9.,13.2664991614216,-20.));
#35095=CARTESIAN_POINT('Ctrl Pts',(9.09995111742602,13.2664991614216,-20.));
#35096=CARTESIAN_POINT('Ctrl Pts',(9.21480544093045,13.231938929479,-20.));
#35097=CARTESIAN_POINT('Ctrl Pts',(9.42146594446646,13.1132046912743,-20.));
#35098=CARTESIAN_POINT('Ctrl Pts',(9.53638021469469,12.9933163967994,-20.));
#35099=CARTESIAN_POINT('Ctrl Pts',(9.7313641110186,12.7122458236771,-20.));
#35100=CARTESIAN_POINT('Ctrl Pts',(9.82490699559395,12.4864240538002,-20.));
#35101=CARTESIAN_POINT('Ctrl Pts',(9.96053133753905,12.0059148948794,-20.));
#35102=CARTESIAN_POINT('Ctrl Pts',(10.,11.6534080045929,-20.));
#35103=CARTESIAN_POINT('Ctrl Pts',(10.,11.3578166916006,-20.));
#35104=CARTESIAN_POINT('Origin',(9.,0.,0.));
#35105=CARTESIAN_POINT('Origin',(-34.1076474136955,0.,0.));
#35106=CARTESIAN_POINT('',(0.999999999999992,13.2664991614216,-20.));
#35107=CARTESIAN_POINT('',(-34.1076474136955,13.2664991614216,-20.));
#35108=CARTESIAN_POINT('',(0.999999999999971,13.2664991614216,20.));
#35109=CARTESIAN_POINT('Origin',(1.,0.,0.));
#35110=CARTESIAN_POINT('',(-34.1076474136955,13.2664991614216,20.));
#35111=CARTESIAN_POINT('Origin',(-34.1076474136955,0.,0.));
#35112=CARTESIAN_POINT('',(1.,-13.2664991614216,-20.));
#35113=CARTESIAN_POINT('',(-34.1076474136955,-13.2664991614216,-20.));
#35114=CARTESIAN_POINT('',(1.,-13.2664991614216,20.));
#35115=CARTESIAN_POINT('',(-34.1076474136955,-13.2664991614216,20.));
#35116=CARTESIAN_POINT('Origin',(1.,0.,0.));
#35117=CARTESIAN_POINT('Origin',(1.,0.,0.));
#35118=CARTESIAN_POINT('',(1.73472347597681E-15,-11.3578166916005,20.));
#35119=CARTESIAN_POINT('Ctrl Pts',(-4.16333634234434E-16,-11.3578166916005,
20.));
#35120=CARTESIAN_POINT('Ctrl Pts',(-8.757748284231E-16,-11.6534080045929,
20.));
#35121=CARTESIAN_POINT('Ctrl Pts',(0.039468662460955,-12.0059148948793,
20.));
#35122=CARTESIAN_POINT('Ctrl Pts',(0.175093004406055,-12.4864240538002,
20.));
#35123=CARTESIAN_POINT('Ctrl Pts',(0.268635888981406,-12.7122458236771,
20.));
#35124=CARTESIAN_POINT('Ctrl Pts',(0.463619785305314,-12.9933163967994,
20.));
#35125=CARTESIAN_POINT('Ctrl Pts',(0.578534055533546,-13.1132046912743,
20.));
#35126=CARTESIAN_POINT('Ctrl Pts',(0.785194559069557,-13.231938929479,20.));
#35127=CARTESIAN_POINT('Ctrl Pts',(0.900048882573979,-13.2664991614216,
20.));
#35128=CARTESIAN_POINT('Ctrl Pts',(1.,-13.2664991614216,20.));
#35129=CARTESIAN_POINT('',(0.,-11.3578166916005,-20.));
#35130=CARTESIAN_POINT('Origin',(0.,0.,0.));
#35131=CARTESIAN_POINT('Ctrl Pts',(1.,-13.2664991614216,-20.));
#35132=CARTESIAN_POINT('Ctrl Pts',(0.900048882573979,-13.2664991614216,
-20.));
#35133=CARTESIAN_POINT('Ctrl Pts',(0.785194559069558,-13.231938929479,-20.));
#35134=CARTESIAN_POINT('Ctrl Pts',(0.578534055533547,-13.1132046912743,
-20.));
#35135=CARTESIAN_POINT('Ctrl Pts',(0.463619785305315,-12.9933163967994,
-20.));
#35136=CARTESIAN_POINT('Ctrl Pts',(0.268635888981407,-12.7122458236771,
-20.));
#35137=CARTESIAN_POINT('Ctrl Pts',(0.175093004406055,-12.4864240538002,
-20.));
#35138=CARTESIAN_POINT('Ctrl Pts',(0.0394686624609555,-12.0059148948793,
-20.));
#35139=CARTESIAN_POINT('Ctrl Pts',(-1.0726781973611E-15,-11.6534080045929,
-20.));
#35140=CARTESIAN_POINT('Ctrl Pts',(-4.16333634234433E-16,-11.3578166916006,
-20.));
#35141=CARTESIAN_POINT('Origin',(1.,0.,0.));
#35142=CARTESIAN_POINT('',(0.,11.3578166916005,20.));
#35143=CARTESIAN_POINT('Ctrl Pts',(0.999999999999971,13.2664991614216,20.));
#35144=CARTESIAN_POINT('Ctrl Pts',(0.90004888257395,13.2664991614216,20.));
#35145=CARTESIAN_POINT('Ctrl Pts',(0.785194559069557,13.231938929479,20.));
#35146=CARTESIAN_POINT('Ctrl Pts',(0.578534055533546,13.1132046912743,20.));
#35147=CARTESIAN_POINT('Ctrl Pts',(0.463619785305314,12.9933163967994,20.));
#35148=CARTESIAN_POINT('Ctrl Pts',(0.268635888981406,12.7122458236771,20.));
#35149=CARTESIAN_POINT('Ctrl Pts',(0.175093004406055,12.4864240538002,20.));
#35150=CARTESIAN_POINT('Ctrl Pts',(0.039468662460955,12.0059148948794,20.));
#35151=CARTESIAN_POINT('Ctrl Pts',(-4.16333634234434E-16,11.6534080045929,
20.));
#35152=CARTESIAN_POINT('Ctrl Pts',(-4.16333634234434E-16,11.3578166916006,
20.));
#35153=CARTESIAN_POINT('',(1.73472347597681E-15,11.3578166916005,-20.));
#35154=CARTESIAN_POINT('Ctrl Pts',(-4.16333634234434E-16,11.3578166916006,
-20.));
#35155=CARTESIAN_POINT('Ctrl Pts',(-1.05562532344124E-15,11.6534080045929,
-20.));
#35156=CARTESIAN_POINT('Ctrl Pts',(0.0394686624609556,12.0059148948794,
-20.));
#35157=CARTESIAN_POINT('Ctrl Pts',(0.175093004406055,12.4864240538002,-20.));
#35158=CARTESIAN_POINT('Ctrl Pts',(0.268635888981407,12.7122458236771,-20.));
#35159=CARTESIAN_POINT('Ctrl Pts',(0.463619785305315,12.9933163967994,-20.));
#35160=CARTESIAN_POINT('Ctrl Pts',(0.578534055533547,13.1132046912743,-20.));
#35161=CARTESIAN_POINT('Ctrl Pts',(0.785194559069558,13.231938929479,-20.));
#35162=CARTESIAN_POINT('Ctrl Pts',(0.900048882573979,13.2664991614216,-20.));
#35163=CARTESIAN_POINT('Ctrl Pts',(1.,13.2664991614216,-20.));
#35164=CARTESIAN_POINT('Origin',(0.,0.,0.));
#35165=CARTESIAN_POINT('Origin',(0.,14.,0.));
#35166=CARTESIAN_POINT('',(0.,14.,20.));
#35167=CARTESIAN_POINT('',(0.,14.,-20.));
#35168=CARTESIAN_POINT('Origin',(-32.,11.,0.));
#35169=CARTESIAN_POINT('Origin',(-31.5,11.,0.));
#35170=CARTESIAN_POINT('Origin',(-32.,10.75,0.));
#35171=CARTESIAN_POINT('Origin',(10.,10.75,0.));
#35172=CARTESIAN_POINT('Origin',(9.5,10.75,0.));
#35173=CARTESIAN_POINT('Origin',(1.73472347597681E-15,24.,-20.));
#35174=CARTESIAN_POINT('Origin',(1.73472347597681E-15,24.,20.));
#35175=CARTESIAN_POINT('',(0.,0.,0.));
#35176=CARTESIAN_POINT('',(110.842837782404,4.13590306276514E-21,-1.38777878078145E-14));
#35177=CARTESIAN_POINT('',(0.,0.,0.));
#35178=CARTESIAN_POINT('',(0.,0.,0.));
#35179=CARTESIAN_POINT('Origin',(12.,24.,26.));
#35180=CARTESIAN_POINT('',(12.,-1.77635683940025E-14,21.5));
#35181=CARTESIAN_POINT('Origin',(12.,-1.73472347597681E-14,26.));
#35182=CARTESIAN_POINT('',(12.,24.,21.5));
#35183=CARTESIAN_POINT('',(12.,24.,21.5));
#35184=CARTESIAN_POINT('Origin',(12.,24.,26.));
#35185=CARTESIAN_POINT('Origin',(12.,24.,-26.));
#35186=CARTESIAN_POINT('',(12.,-4.44089209850063E-15,-30.5));
#35187=CARTESIAN_POINT('Origin',(12.,-3.46944695195361E-15,-26.));
#35188=CARTESIAN_POINT('',(12.,24.,-30.5));
#35189=CARTESIAN_POINT('',(12.,24.,-30.5));
#35190=CARTESIAN_POINT('Origin',(12.,24.,-26.));
#35191=CARTESIAN_POINT('Origin',(30.,25.,0.));
#35192=CARTESIAN_POINT('',(24.,25.,12.));
#35193=CARTESIAN_POINT('Origin',(24.,25.,0.));
#35194=CARTESIAN_POINT('',(30.,25.,12.));
#35195=CARTESIAN_POINT('',(30.,25.,12.));
#35196=CARTESIAN_POINT('Origin',(30.,25.,0.));
#35197=CARTESIAN_POINT('Origin',(30.,25.,0.));
#35198=CARTESIAN_POINT('',(22.,25.,7.75));
#35199=CARTESIAN_POINT('Origin',(22.,25.,0.));
#35200=CARTESIAN_POINT('',(24.,25.,7.75));
#35201=CARTESIAN_POINT('',(30.,25.,7.75));
#35202=CARTESIAN_POINT('Origin',(24.,25.,0.));
#35203=CARTESIAN_POINT('Origin',(30.,25.,0.));
#35204=CARTESIAN_POINT('',(6.,25.,6.00000000000001));
#35205=CARTESIAN_POINT('Origin',(6.,25.,0.));
#35206=CARTESIAN_POINT('',(22.,25.,6.00000000000001));
#35207=CARTESIAN_POINT('',(30.,25.,6.00000000000001));
#35208=CARTESIAN_POINT('Origin',(22.,25.,0.));
#35209=CARTESIAN_POINT('Origin',(30.,25.,0.));
#35210=CARTESIAN_POINT('',(3.,25.,7.74999999999999));
#35211=CARTESIAN_POINT('Origin',(3.,25.,0.));
#35212=CARTESIAN_POINT('',(6.,25.,7.74999999999999));
#35213=CARTESIAN_POINT('',(30.,25.,7.74999999999999));
#35214=CARTESIAN_POINT('Origin',(6.,25.,0.));
#35215=CARTESIAN_POINT('Origin',(30.,25.,0.));
#35216=CARTESIAN_POINT('',(0.,25.,12.));
#35217=CARTESIAN_POINT('Origin',(0.,25.,0.));
#35218=CARTESIAN_POINT('',(3.,25.,12.));
#35219=CARTESIAN_POINT('',(30.,25.,12.));
#35220=CARTESIAN_POINT('Origin',(3.,25.,0.));
#35221=CARTESIAN_POINT('Origin',(27.,11.95,-13.05));
#35222=CARTESIAN_POINT('',(26.0987090714587,11.95,-13.05));
#35223=CARTESIAN_POINT('',(27.,11.95,-11.55));
#35224=CARTESIAN_POINT('',(27.,11.95,-11.55));
#35225=CARTESIAN_POINT('',(27.,10.6509618943234,-12.3));
#35226=CARTESIAN_POINT('Origin',(27.,11.95,-13.05));
#35227=CARTESIAN_POINT('',(27.,10.6509618943234,-13.8));
#35228=CARTESIAN_POINT('Origin',(27.,11.95,-13.05));
#35229=CARTESIAN_POINT('',(27.,11.95,-14.55));
#35230=CARTESIAN_POINT('Origin',(27.,11.95,-13.05));
#35231=CARTESIAN_POINT('',(27.,13.2490381056767,-13.8));
#35232=CARTESIAN_POINT('Origin',(27.,11.95,-13.05));
#35233=CARTESIAN_POINT('',(27.,13.2490381056767,-12.3));
#35234=CARTESIAN_POINT('Origin',(27.,11.95,-13.05));
#35235=CARTESIAN_POINT('Origin',(27.,11.95,-13.05));
#35236=CARTESIAN_POINT('Origin',(27.,11.95,13.05));
#35237=CARTESIAN_POINT('',(26.0987090714587,11.95,13.05));
#35238=CARTESIAN_POINT('',(27.,11.95,14.55));
#35239=CARTESIAN_POINT('',(27.,11.95,14.55));
#35240=CARTESIAN_POINT('',(27.,10.6509618943234,13.8));
#35241=CARTESIAN_POINT('Origin',(27.,11.95,13.05));
#35242=CARTESIAN_POINT('',(27.,10.6509618943234,12.3));
#35243=CARTESIAN_POINT('Origin',(27.,11.95,13.05));
#35244=CARTESIAN_POINT('',(27.,11.95,11.55));
#35245=CARTESIAN_POINT('Origin',(27.,11.95,13.05));
#35246=CARTESIAN_POINT('',(27.,13.2490381056767,12.3));
#35247=CARTESIAN_POINT('Origin',(27.,11.95,13.05));
#35248=CARTESIAN_POINT('',(27.,13.2490381056767,13.8));
#35249=CARTESIAN_POINT('Origin',(27.,11.95,13.05));
#35250=CARTESIAN_POINT('Origin',(27.,11.95,13.05));
#35251=CARTESIAN_POINT('Origin',(27.,38.05,-13.05));
#35252=CARTESIAN_POINT('',(26.0987090714587,38.05,-13.05));
#35253=CARTESIAN_POINT('',(27.,38.05,-11.55));
#35254=CARTESIAN_POINT('',(27.,38.05,-11.55));
#35255=CARTESIAN_POINT('',(27.,36.7509618943233,-12.3));
#35256=CARTESIAN_POINT('Origin',(27.,38.05,-13.05));
#35257=CARTESIAN_POINT('',(27.,36.7509618943233,-13.8));
#35258=CARTESIAN_POINT('Origin',(27.,38.05,-13.05));
#35259=CARTESIAN_POINT('',(27.,38.05,-14.55));
#35260=CARTESIAN_POINT('Origin',(27.,38.05,-13.05));
#35261=CARTESIAN_POINT('',(27.,39.3490381056766,-13.8));
#35262=CARTESIAN_POINT('Origin',(27.,38.05,-13.05));
#35263=CARTESIAN_POINT('',(27.,39.3490381056766,-12.3));
#35264=CARTESIAN_POINT('Origin',(27.,38.05,-13.05));
#35265=CARTESIAN_POINT('Origin',(27.,38.05,-13.05));
#35266=CARTESIAN_POINT('Origin',(27.,38.05,13.05));
#35267=CARTESIAN_POINT('',(26.0987090714587,38.05,13.05));
#35268=CARTESIAN_POINT('',(27.,38.05,14.55));
#35269=CARTESIAN_POINT('',(27.,38.05,14.55));
#35270=CARTESIAN_POINT('',(27.,36.7509618943233,13.8));
#35271=CARTESIAN_POINT('Origin',(27.,38.05,13.05));
#35272=CARTESIAN_POINT('',(27.,36.7509618943233,12.3));
#35273=CARTESIAN_POINT('Origin',(27.,38.05,13.05));
#35274=CARTESIAN_POINT('',(27.,38.05,11.55));
#35275=CARTESIAN_POINT('Origin',(27.,38.05,13.05));
#35276=CARTESIAN_POINT('',(27.,39.3490381056766,12.3));
#35277=CARTESIAN_POINT('Origin',(27.,38.05,13.05));
#35278=CARTESIAN_POINT('',(27.,39.3490381056766,13.8));
#35279=CARTESIAN_POINT('Origin',(27.,38.05,13.05));
#35280=CARTESIAN_POINT('Origin',(27.,38.05,13.05));
#35281=CARTESIAN_POINT('Origin',(30.,11.95,13.05));
#35282=CARTESIAN_POINT('',(24.,11.95,9.94999999999999));
#35283=CARTESIAN_POINT('Origin',(24.,11.95,13.05));
#35284=CARTESIAN_POINT('',(30.,11.95,9.94999999999999));
#35285=CARTESIAN_POINT('',(30.,11.95,9.94999999999999));
#35286=CARTESIAN_POINT('Origin',(30.,11.95,13.05));
#35287=CARTESIAN_POINT('Origin',(30.,11.95,-13.05));
#35288=CARTESIAN_POINT('',(24.,11.95,-16.15));
#35289=CARTESIAN_POINT('Origin',(24.,11.95,-13.05));
#35290=CARTESIAN_POINT('',(30.,11.95,-16.15));
#35291=CARTESIAN_POINT('',(30.,11.95,-16.15));
#35292=CARTESIAN_POINT('Origin',(30.,11.95,-13.05));
#35293=CARTESIAN_POINT('Origin',(30.,38.05,-13.05));
#35294=CARTESIAN_POINT('',(24.,38.05,-16.15));
#35295=CARTESIAN_POINT('Origin',(24.,38.05,-13.05));
#35296=CARTESIAN_POINT('',(30.,38.05,-16.15));
#35297=CARTESIAN_POINT('',(30.,38.05,-16.15));
#35298=CARTESIAN_POINT('Origin',(30.,38.05,-13.05));
#35299=CARTESIAN_POINT('Origin',(30.,38.05,13.05));
#35300=CARTESIAN_POINT('',(24.,38.05,9.94999999999999));
#35301=CARTESIAN_POINT('Origin',(24.,38.05,13.05));
#35302=CARTESIAN_POINT('',(30.,38.05,9.94999999999999));
#35303=CARTESIAN_POINT('',(30.,38.05,9.94999999999999));
#35304=CARTESIAN_POINT('Origin',(30.,38.05,13.05));
#35305=CARTESIAN_POINT('Origin',(30.,11.95,-13.05));
#35306=CARTESIAN_POINT('',(30.,11.95,-16.55));
#35307=CARTESIAN_POINT('Origin',(30.,11.95,-13.05));
#35308=CARTESIAN_POINT('',(24.,11.95,-16.55));
#35309=CARTESIAN_POINT('',(30.,11.95,-16.55));
#35310=CARTESIAN_POINT('Origin',(24.,11.95,-13.05));
#35311=CARTESIAN_POINT('Origin',(30.,11.95,13.05));
#35312=CARTESIAN_POINT('',(30.,11.95,9.55));
#35313=CARTESIAN_POINT('Origin',(30.,11.95,13.05));
#35314=CARTESIAN_POINT('',(24.,11.95,9.55));
#35315=CARTESIAN_POINT('',(30.,11.95,9.55));
#35316=CARTESIAN_POINT('Origin',(24.,11.95,13.05));
#35317=CARTESIAN_POINT('Origin',(30.,38.05,-13.05));
#35318=CARTESIAN_POINT('',(30.,38.05,-16.55));
#35319=CARTESIAN_POINT('Origin',(30.,38.05,-13.05));
#35320=CARTESIAN_POINT('',(24.,38.05,-16.55));
#35321=CARTESIAN_POINT('',(30.,38.05,-16.55));
#35322=CARTESIAN_POINT('Origin',(24.,38.05,-13.05));
#35323=CARTESIAN_POINT('Origin',(30.,38.05,13.05));
#35324=CARTESIAN_POINT('',(30.,38.05,9.54999999999998));
#35325=CARTESIAN_POINT('Origin',(30.,38.05,13.05));
#35326=CARTESIAN_POINT('',(24.,38.05,9.54999999999998));
#35327=CARTESIAN_POINT('',(30.,38.05,9.54999999999998));
#35328=CARTESIAN_POINT('Origin',(24.,38.05,13.05));
#35329=CARTESIAN_POINT('Origin',(24.,0.,0.));
#35330=CARTESIAN_POINT('Origin',(24.,0.,0.));
#35331=CARTESIAN_POINT('Origin',(24.,0.,0.));
#35332=CARTESIAN_POINT('Origin',(24.,0.,0.));
#35333=CARTESIAN_POINT('Origin',(24.,0.,0.));
#35334=CARTESIAN_POINT('',(24.,24.,18.0000000000001));
#35335=CARTESIAN_POINT('',(24.,24.,34.5));
#35336=CARTESIAN_POINT('',(24.,24.,18.0000000000001));
#35337=CARTESIAN_POINT('',(24.,23.5,35.));
#35338=CARTESIAN_POINT('',(24.,24.,34.5));
#35339=CARTESIAN_POINT('',(24.,7.70371977754894E-31,35.));
#35340=CARTESIAN_POINT('',(24.,23.5,35.));
#35341=CARTESIAN_POINT('',(24.,1.78732264387927E-14,-35.));
#35342=CARTESIAN_POINT('',(24.,7.70371977754894E-31,35.));
#35343=CARTESIAN_POINT('',(24.,23.5,-35.));
#35344=CARTESIAN_POINT('',(24.,23.5,-35.));
#35345=CARTESIAN_POINT('',(24.,24.,-34.5));
#35346=CARTESIAN_POINT('',(24.,24.,-34.5));
#35347=CARTESIAN_POINT('',(24.,24.,-17.9999999999999));
#35348=CARTESIAN_POINT('',(24.,24.,-17.9999999999999));
#35349=CARTESIAN_POINT('',(24.,42.5,-17.9999999999999));
#35350=CARTESIAN_POINT('',(24.,42.5,-17.9999999999999));
#35351=CARTESIAN_POINT('',(24.,43.,-17.4999999999999));
#35352=CARTESIAN_POINT('',(24.,43.,-17.4999999999999));
#35353=CARTESIAN_POINT('',(24.,43.,17.5));
#35354=CARTESIAN_POINT('',(24.,43.,17.5));
#35355=CARTESIAN_POINT('',(24.,42.5,18.0000000000001));
#35356=CARTESIAN_POINT('',(24.,42.5,18.0000000000001));
#35357=CARTESIAN_POINT('',(24.,42.5,18.0000000000001));
#35358=CARTESIAN_POINT('',(24.,42.75,15.75));
#35359=CARTESIAN_POINT('',(24.,40.75,17.75));
#35360=CARTESIAN_POINT('',(24.,40.75,17.75));
#35361=CARTESIAN_POINT('',(24.,42.75,-15.75));
#35362=CARTESIAN_POINT('',(24.,42.75,15.75));
#35363=CARTESIAN_POINT('',(24.,40.75,-17.75));
#35364=CARTESIAN_POINT('',(24.,42.75,-15.75));
#35365=CARTESIAN_POINT('',(24.,9.25000000000001,-17.75));
#35366=CARTESIAN_POINT('',(24.,40.75,-17.75));
#35367=CARTESIAN_POINT('',(24.,7.25000000000001,-15.75));
#35368=CARTESIAN_POINT('',(24.,9.25000000000001,-17.75));
#35369=CARTESIAN_POINT('',(24.,7.25000000000001,15.75));
#35370=CARTESIAN_POINT('',(24.,7.25000000000001,15.75));
#35371=CARTESIAN_POINT('',(24.,9.25000000000001,17.75));
#35372=CARTESIAN_POINT('',(24.,9.25000000000001,17.75));
#35373=CARTESIAN_POINT('',(24.,40.75,17.75));
#35374=CARTESIAN_POINT('Origin',(24.,24.,18.0000000000001));
#35375=CARTESIAN_POINT('',(0.,24.,18.0000000000001));
#35376=CARTESIAN_POINT('',(0.,24.,34.5));
#35377=CARTESIAN_POINT('',(0.,24.,18.0000000000001));
#35378=CARTESIAN_POINT('',(24.,24.,34.5));
#35379=CARTESIAN_POINT('',(24.,24.,18.0000000000001));
#35380=CARTESIAN_POINT('Origin',(24.,24.,34.5));
#35381=CARTESIAN_POINT('',(0.,23.5,35.));
#35382=CARTESIAN_POINT('',(0.,24.,34.5));
#35383=CARTESIAN_POINT('',(24.,23.5,35.));
#35384=CARTESIAN_POINT('Origin',(24.,23.5,35.));
#35385=CARTESIAN_POINT('',(0.,7.70371977754894E-31,35.));
#35386=CARTESIAN_POINT('',(0.,23.5,35.));
#35387=CARTESIAN_POINT('',(24.,7.70371977754894E-31,35.));
#35388=CARTESIAN_POINT('Origin',(24.,7.70371977754894E-31,35.));
#35389=CARTESIAN_POINT('',(0.,1.78732264387927E-14,-35.));
#35390=CARTESIAN_POINT('',(0.,7.70371977754894E-31,35.));
#35391=CARTESIAN_POINT('',(24.,1.78732264387927E-14,-35.));
#35392=CARTESIAN_POINT('Origin',(24.,23.5,-35.));
#35393=CARTESIAN_POINT('',(0.,23.5,-35.));
#35394=CARTESIAN_POINT('',(0.,23.5,-35.));
#35395=CARTESIAN_POINT('',(24.,23.5,-35.));
#35396=CARTESIAN_POINT('Origin',(24.,24.,-34.5));
#35397=CARTESIAN_POINT('',(0.,24.,-34.5));
#35398=CARTESIAN_POINT('',(0.,24.,-34.5));
#35399=CARTESIAN_POINT('',(24.,24.,-34.5));
#35400=CARTESIAN_POINT('Origin',(24.,24.,-17.9999999999999));
#35401=CARTESIAN_POINT('',(0.,24.,-17.9999999999999));
#35402=CARTESIAN_POINT('',(0.,24.,-17.9999999999999));
#35403=CARTESIAN_POINT('',(24.,24.,-17.9999999999999));
#35404=CARTESIAN_POINT('Origin',(24.,42.5,-17.9999999999999));
#35405=CARTESIAN_POINT('',(0.,42.5,-17.9999999999999));
#35406=CARTESIAN_POINT('',(0.,42.5,-17.9999999999999));
#35407=CARTESIAN_POINT('',(24.,42.5,-17.9999999999999));
#35408=CARTESIAN_POINT('Origin',(24.,43.,-17.4999999999999));
#35409=CARTESIAN_POINT('',(0.,43.,-17.4999999999999));
#35410=CARTESIAN_POINT('',(0.,43.,-17.4999999999999));
#35411=CARTESIAN_POINT('',(24.,43.,-17.4999999999999));
#35412=CARTESIAN_POINT('Origin',(24.,43.,17.5));
#35413=CARTESIAN_POINT('',(0.,43.,17.5));
#35414=CARTESIAN_POINT('',(0.,43.,17.5));
#35415=CARTESIAN_POINT('',(24.,43.,17.5));
#35416=CARTESIAN_POINT('Origin',(24.,42.5,18.0000000000001));
#35417=CARTESIAN_POINT('',(0.,42.5,18.0000000000001));
#35418=CARTESIAN_POINT('',(0.,42.5,18.0000000000001));
#35419=CARTESIAN_POINT('',(24.,42.5,18.0000000000001));
#35420=CARTESIAN_POINT('Origin',(24.,42.5,18.0000000000001));
#35421=CARTESIAN_POINT('',(0.,42.5,18.0000000000001));
#35422=CARTESIAN_POINT('Origin',(0.,0.,0.));
#35423=CARTESIAN_POINT('Origin',(30.,0.,0.));
#35424=CARTESIAN_POINT('',(30.,42.75,-15.75));
#35425=CARTESIAN_POINT('',(30.,42.75,15.75));
#35426=CARTESIAN_POINT('',(30.,42.75,15.75));
#35427=CARTESIAN_POINT('',(30.,40.75,17.75));
#35428=CARTESIAN_POINT('',(30.,40.75,17.75));
#35429=CARTESIAN_POINT('',(30.,9.25000000000001,17.75));
#35430=CARTESIAN_POINT('',(30.,40.75,17.75));
#35431=CARTESIAN_POINT('',(30.,7.25000000000001,15.75));
#35432=CARTESIAN_POINT('',(30.,9.25000000000001,17.75));
#35433=CARTESIAN_POINT('',(30.,7.25000000000001,-15.75));
#35434=CARTESIAN_POINT('',(30.,7.25000000000001,15.75));
#35435=CARTESIAN_POINT('',(30.,9.25000000000001,-17.75));
#35436=CARTESIAN_POINT('',(30.,9.25000000000001,-17.75));
#35437=CARTESIAN_POINT('',(30.,40.75,-17.75));
#35438=CARTESIAN_POINT('',(30.,40.75,-17.75));
#35439=CARTESIAN_POINT('',(30.,42.75,-15.75));
#35440=CARTESIAN_POINT('Origin',(30.,42.75,15.75));
#35441=CARTESIAN_POINT('',(30.,42.75,15.75));
#35442=CARTESIAN_POINT('',(30.,42.75,-15.75));
#35443=CARTESIAN_POINT('Origin',(30.,40.75,17.75));
#35444=CARTESIAN_POINT('',(30.,40.75,17.75));
#35445=CARTESIAN_POINT('Origin',(30.,40.75,17.75));
#35446=CARTESIAN_POINT('',(30.,9.25000000000001,17.75));
#35447=CARTESIAN_POINT('Origin',(30.,9.25000000000001,17.75));
#35448=CARTESIAN_POINT('',(30.,7.25000000000001,15.75));
#35449=CARTESIAN_POINT('Origin',(30.,7.25000000000001,15.75));
#35450=CARTESIAN_POINT('',(30.,7.25000000000001,-15.75));
#35451=CARTESIAN_POINT('Origin',(30.,9.25000000000001,-17.75));
#35452=CARTESIAN_POINT('',(30.,9.25000000000001,-17.75));
#35453=CARTESIAN_POINT('Origin',(30.,40.75,-17.75));
#35454=CARTESIAN_POINT('',(30.,40.75,-17.75));
#35455=CARTESIAN_POINT('Origin',(30.,42.75,-15.75));
#35456=CARTESIAN_POINT('Origin',(30.,38.05,13.05));
#35457=CARTESIAN_POINT('',(30.,39.7820508075689,13.05));
#35458=CARTESIAN_POINT('',(30.,38.9160254037844,14.55));
#35459=CARTESIAN_POINT('',(30.,39.7820508075689,13.05));
#35460=CARTESIAN_POINT('',(30.,38.9160254037844,11.55));
#35461=CARTESIAN_POINT('',(30.,38.9160254037844,11.55));
#35462=CARTESIAN_POINT('',(30.,37.1839745962155,11.55));
#35463=CARTESIAN_POINT('',(30.,37.1839745962155,11.55));
#35464=CARTESIAN_POINT('',(30.,36.3179491924311,13.05));
#35465=CARTESIAN_POINT('',(30.,36.3179491924311,13.05));
#35466=CARTESIAN_POINT('',(30.,37.1839745962155,14.55));
#35467=CARTESIAN_POINT('',(30.,37.1839745962155,14.55));
#35468=CARTESIAN_POINT('',(30.,38.9160254037844,14.55));
#35469=CARTESIAN_POINT('Origin',(30.,38.05,-13.05));
#35470=CARTESIAN_POINT('',(30.,38.9160254037844,-11.55));
#35471=CARTESIAN_POINT('',(30.,37.1839745962155,-11.55));
#35472=CARTESIAN_POINT('',(30.,38.9160254037844,-11.55));
#35473=CARTESIAN_POINT('',(30.,39.7820508075689,-13.05));
#35474=CARTESIAN_POINT('',(30.,39.7820508075689,-13.05));
#35475=CARTESIAN_POINT('',(30.,38.9160254037844,-14.55));
#35476=CARTESIAN_POINT('',(30.,38.9160254037844,-14.55));
#35477=CARTESIAN_POINT('',(30.,37.1839745962156,-14.55));
#35478=CARTESIAN_POINT('',(30.,37.1839745962156,-14.55));
#35479=CARTESIAN_POINT('',(30.,36.3179491924311,-13.05));
#35480=CARTESIAN_POINT('',(30.,36.3179491924311,-13.05));
#35481=CARTESIAN_POINT('',(30.,37.1839745962155,-11.55));
#35482=CARTESIAN_POINT('Origin',(30.,11.95,-13.05));
#35483=CARTESIAN_POINT('',(30.,12.8160254037845,-11.55));
#35484=CARTESIAN_POINT('',(30.,11.0839745962156,-11.55));
#35485=CARTESIAN_POINT('',(30.,12.8160254037845,-11.55));
#35486=CARTESIAN_POINT('',(30.,13.6820508075689,-13.05));
#35487=CARTESIAN_POINT('',(30.,13.6820508075689,-13.05));
#35488=CARTESIAN_POINT('',(30.,12.8160254037845,-14.55));
#35489=CARTESIAN_POINT('',(30.,12.8160254037845,-14.55));
#35490=CARTESIAN_POINT('',(30.,11.0839745962156,-14.55));
#35491=CARTESIAN_POINT('',(30.,11.0839745962156,-14.55));
#35492=CARTESIAN_POINT('',(30.,10.2179491924311,-13.05));
#35493=CARTESIAN_POINT('',(30.,10.2179491924311,-13.05));
#35494=CARTESIAN_POINT('',(30.,11.0839745962156,-11.55));
#35495=CARTESIAN_POINT('Origin',(30.,11.95,13.05));
#35496=CARTESIAN_POINT('',(30.,12.8160254037845,14.55));
#35497=CARTESIAN_POINT('',(30.,11.0839745962156,14.55));
#35498=CARTESIAN_POINT('',(30.,12.8160254037845,14.55));
#35499=CARTESIAN_POINT('',(30.,13.6820508075689,13.05));
#35500=CARTESIAN_POINT('',(30.,13.6820508075689,13.05));
#35501=CARTESIAN_POINT('',(30.,12.8160254037844,11.55));
#35502=CARTESIAN_POINT('',(30.,12.8160254037844,11.55));
#35503=CARTESIAN_POINT('',(30.,11.0839745962156,11.55));
#35504=CARTESIAN_POINT('',(30.,11.0839745962156,11.55));
#35505=CARTESIAN_POINT('',(30.,10.2179491924311,13.05));
#35506=CARTESIAN_POINT('',(30.,10.2179491924311,13.05));
#35507=CARTESIAN_POINT('',(30.,11.0839745962156,14.55));
#35508=CARTESIAN_POINT('Origin',(27.,37.1839745962155,14.55));
#35509=CARTESIAN_POINT('',(27.,36.3179491924311,13.05));
#35510=CARTESIAN_POINT('',(27.,36.3179491924311,13.05));
#35511=CARTESIAN_POINT('',(27.,37.1839745962155,14.55));
#35512=CARTESIAN_POINT('',(27.,37.1839745962155,14.55));
#35513=CARTESIAN_POINT('',(27.,37.1839745962155,14.55));
#35514=CARTESIAN_POINT('',(27.,37.1839745962155,14.55));
#35515=CARTESIAN_POINT('Origin',(27.,38.9160254037844,14.55));
#35516=CARTESIAN_POINT('',(27.,38.9160254037844,14.55));
#35517=CARTESIAN_POINT('',(27.,38.9160254037844,14.55));
#35518=CARTESIAN_POINT('',(27.,38.9160254037844,14.55));
#35519=CARTESIAN_POINT('',(27.,38.9160254037844,14.55));
#35520=CARTESIAN_POINT('Origin',(27.,39.7820508075689,13.05));
#35521=CARTESIAN_POINT('',(27.,39.7820508075689,13.05));
#35522=CARTESIAN_POINT('',(27.,39.7820508075689,13.05));
#35523=CARTESIAN_POINT('',(27.,39.7820508075689,13.05));
#35524=CARTESIAN_POINT('',(27.,39.7820508075689,13.05));
#35525=CARTESIAN_POINT('Origin',(27.,38.9160254037844,11.55));
#35526=CARTESIAN_POINT('',(27.,38.9160254037844,11.55));
#35527=CARTESIAN_POINT('',(27.,38.9160254037844,11.55));
#35528=CARTESIAN_POINT('',(27.,38.9160254037844,11.55));
#35529=CARTESIAN_POINT('',(27.,38.9160254037844,11.55));
#35530=CARTESIAN_POINT('Origin',(27.,37.1839745962155,11.55));
#35531=CARTESIAN_POINT('',(27.,37.1839745962155,11.55));
#35532=CARTESIAN_POINT('',(27.,37.1839745962155,11.55));
#35533=CARTESIAN_POINT('',(27.,37.1839745962155,11.55));
#35534=CARTESIAN_POINT('',(27.,37.1839745962155,11.55));
#35535=CARTESIAN_POINT('Origin',(27.,36.3179491924311,13.05));
#35536=CARTESIAN_POINT('',(27.,36.3179491924311,13.05));
#35537=CARTESIAN_POINT('',(27.,36.3179491924311,13.05));
#35538=CARTESIAN_POINT('Origin',(27.,0.,0.));
#35539=CARTESIAN_POINT('Origin',(27.,0.,0.));
#35540=CARTESIAN_POINT('Origin',(27.,0.,0.));
#35541=CARTESIAN_POINT('Origin',(27.,0.,0.));
#35542=CARTESIAN_POINT('Origin',(27.,0.,0.));
#35543=CARTESIAN_POINT('Origin',(27.,0.,0.));
#35544=CARTESIAN_POINT('Origin',(27.,36.3179491924311,-13.05));
#35545=CARTESIAN_POINT('',(27.,37.1839745962156,-14.55));
#35546=CARTESIAN_POINT('',(27.,37.1839745962156,-14.55));
#35547=CARTESIAN_POINT('',(27.,36.3179491924311,-13.05));
#35548=CARTESIAN_POINT('',(27.,36.3179491924311,-13.05));
#35549=CARTESIAN_POINT('',(27.,36.3179491924311,-13.05));
#35550=CARTESIAN_POINT('',(27.,36.3179491924311,-13.05));
#35551=CARTESIAN_POINT('Origin',(27.,37.1839745962155,-11.55));
#35552=CARTESIAN_POINT('',(27.,37.1839745962155,-11.55));
#35553=CARTESIAN_POINT('',(27.,37.1839745962155,-11.55));
#35554=CARTESIAN_POINT('',(27.,37.1839745962155,-11.55));
#35555=CARTESIAN_POINT('',(27.,37.1839745962155,-11.55));
#35556=CARTESIAN_POINT('Origin',(27.,38.9160254037844,-11.55));
#35557=CARTESIAN_POINT('',(27.,38.9160254037844,-11.55));
#35558=CARTESIAN_POINT('',(27.,38.9160254037844,-11.55));
#35559=CARTESIAN_POINT('',(27.,38.9160254037844,-11.55));
#35560=CARTESIAN_POINT('',(27.,38.9160254037844,-11.55));
#35561=CARTESIAN_POINT('Origin',(27.,39.7820508075689,-13.05));
#35562=CARTESIAN_POINT('',(27.,39.7820508075689,-13.05));
#35563=CARTESIAN_POINT('',(27.,39.7820508075689,-13.05));
#35564=CARTESIAN_POINT('',(27.,39.7820508075689,-13.05));
#35565=CARTESIAN_POINT('',(27.,39.7820508075689,-13.05));
#35566=CARTESIAN_POINT('Origin',(27.,38.9160254037844,-14.55));
#35567=CARTESIAN_POINT('',(27.,38.9160254037844,-14.55));
#35568=CARTESIAN_POINT('',(27.,38.9160254037844,-14.55));
#35569=CARTESIAN_POINT('',(27.,38.9160254037844,-14.55));
#35570=CARTESIAN_POINT('',(27.,38.9160254037844,-14.55));
#35571=CARTESIAN_POINT('Origin',(27.,37.1839745962156,-14.55));
#35572=CARTESIAN_POINT('',(27.,37.1839745962156,-14.55));
#35573=CARTESIAN_POINT('',(27.,37.1839745962156,-14.55));
#35574=CARTESIAN_POINT('Origin',(27.,0.,0.));
#35575=CARTESIAN_POINT('Origin',(27.,0.,0.));
#35576=CARTESIAN_POINT('Origin',(27.,0.,0.));
#35577=CARTESIAN_POINT('Origin',(27.,0.,0.));
#35578=CARTESIAN_POINT('Origin',(27.,0.,0.));
#35579=CARTESIAN_POINT('Origin',(27.,0.,0.));
#35580=CARTESIAN_POINT('Origin',(27.,10.2179491924311,13.05));
#35581=CARTESIAN_POINT('',(27.,11.0839745962156,11.55));
#35582=CARTESIAN_POINT('',(27.,11.0839745962156,11.55));
#35583=CARTESIAN_POINT('',(27.,10.2179491924311,13.05));
#35584=CARTESIAN_POINT('',(27.,10.2179491924311,13.05));
#35585=CARTESIAN_POINT('',(27.,10.2179491924311,13.05));
#35586=CARTESIAN_POINT('',(27.,10.2179491924311,13.05));
#35587=CARTESIAN_POINT('Origin',(27.,11.0839745962156,14.55));
#35588=CARTESIAN_POINT('',(27.,11.0839745962156,14.55));
#35589=CARTESIAN_POINT('',(27.,11.0839745962156,14.55));
#35590=CARTESIAN_POINT('',(27.,11.0839745962156,14.55));
#35591=CARTESIAN_POINT('',(27.,11.0839745962156,14.55));
#35592=CARTESIAN_POINT('Origin',(27.,12.8160254037845,14.55));
#35593=CARTESIAN_POINT('',(27.,12.8160254037845,14.55));
#35594=CARTESIAN_POINT('',(27.,12.8160254037845,14.55));
#35595=CARTESIAN_POINT('',(27.,12.8160254037845,14.55));
#35596=CARTESIAN_POINT('',(27.,12.8160254037845,14.55));
#35597=CARTESIAN_POINT('Origin',(27.,13.6820508075689,13.05));
#35598=CARTESIAN_POINT('',(27.,13.6820508075689,13.05));
#35599=CARTESIAN_POINT('',(27.,13.6820508075689,13.05));
#35600=CARTESIAN_POINT('',(27.,13.6820508075689,13.05));
#35601=CARTESIAN_POINT('',(27.,13.6820508075689,13.05));
#35602=CARTESIAN_POINT('Origin',(27.,12.8160254037844,11.55));
#35603=CARTESIAN_POINT('',(27.,12.8160254037844,11.55));
#35604=CARTESIAN_POINT('',(27.,12.8160254037844,11.55));
#35605=CARTESIAN_POINT('',(27.,12.8160254037844,11.55));
#35606=CARTESIAN_POINT('',(27.,12.8160254037844,11.55));
#35607=CARTESIAN_POINT('Origin',(27.,11.0839745962156,11.55));
#35608=CARTESIAN_POINT('',(27.,11.0839745962156,11.55));
#35609=CARTESIAN_POINT('',(27.,11.0839745962156,11.55));
#35610=CARTESIAN_POINT('Origin',(27.,0.,0.));
#35611=CARTESIAN_POINT('Origin',(27.,0.,0.));
#35612=CARTESIAN_POINT('Origin',(27.,0.,0.));
#35613=CARTESIAN_POINT('Origin',(27.,0.,0.));
#35614=CARTESIAN_POINT('Origin',(27.,0.,0.));
#35615=CARTESIAN_POINT('Origin',(27.,0.,0.));
#35616=CARTESIAN_POINT('Origin',(27.,10.2179491924311,-13.05));
#35617=CARTESIAN_POINT('',(27.,11.0839745962156,-14.55));
#35618=CARTESIAN_POINT('',(27.,11.0839745962156,-14.55));
#35619=CARTESIAN_POINT('',(27.,10.2179491924311,-13.05));
#35620=CARTESIAN_POINT('',(27.,10.2179491924311,-13.05));
#35621=CARTESIAN_POINT('',(27.,10.2179491924311,-13.05));
#35622=CARTESIAN_POINT('',(27.,10.2179491924311,-13.05));
#35623=CARTESIAN_POINT('Origin',(27.,11.0839745962156,-11.55));
#35624=CARTESIAN_POINT('',(27.,11.0839745962156,-11.55));
#35625=CARTESIAN_POINT('',(27.,11.0839745962156,-11.55));
#35626=CARTESIAN_POINT('',(27.,11.0839745962156,-11.55));
#35627=CARTESIAN_POINT('',(27.,11.0839745962156,-11.55));
#35628=CARTESIAN_POINT('Origin',(27.,12.8160254037845,-11.55));
#35629=CARTESIAN_POINT('',(27.,12.8160254037845,-11.55));
#35630=CARTESIAN_POINT('',(27.,12.8160254037845,-11.55));
#35631=CARTESIAN_POINT('',(27.,12.8160254037845,-11.55));
#35632=CARTESIAN_POINT('',(27.,12.8160254037845,-11.55));
#35633=CARTESIAN_POINT('Origin',(27.,13.6820508075689,-13.05));
#35634=CARTESIAN_POINT('',(27.,13.6820508075689,-13.05));
#35635=CARTESIAN_POINT('',(27.,13.6820508075689,-13.05));
#35636=CARTESIAN_POINT('',(27.,13.6820508075689,-13.05));
#35637=CARTESIAN_POINT('',(27.,13.6820508075689,-13.05));
#35638=CARTESIAN_POINT('Origin',(27.,12.8160254037845,-14.55));
#35639=CARTESIAN_POINT('',(27.,12.8160254037845,-14.55));
#35640=CARTESIAN_POINT('',(27.,12.8160254037845,-14.55));
#35641=CARTESIAN_POINT('',(27.,12.8160254037845,-14.55));
#35642=CARTESIAN_POINT('',(27.,12.8160254037845,-14.55));
#35643=CARTESIAN_POINT('Origin',(27.,11.0839745962156,-14.55));
#35644=CARTESIAN_POINT('',(27.,11.0839745962156,-14.55));
#35645=CARTESIAN_POINT('',(27.,11.0839745962156,-14.55));
#35646=CARTESIAN_POINT('Origin',(27.,0.,0.));
#35647=CARTESIAN_POINT('Origin',(27.,0.,0.));
#35648=CARTESIAN_POINT('Origin',(27.,0.,0.));
#35649=CARTESIAN_POINT('Origin',(27.,0.,0.));
#35650=CARTESIAN_POINT('Origin',(27.,0.,0.));
#35651=CARTESIAN_POINT('Origin',(27.,0.,0.));
#35652=CARTESIAN_POINT('Origin',(3.,37.,0.));
#35653=CARTESIAN_POINT('Origin',(6.,32.75,0.));
#35654=CARTESIAN_POINT('Origin',(22.,31.,0.));
#35655=CARTESIAN_POINT('Origin',(24.,32.75,0.));
#35656=CARTESIAN_POINT('',(0.,0.,0.));
#35657=CARTESIAN_POINT('Origin',(5.5,11.,0.));
#35658=CARTESIAN_POINT('',(5.5,5.21225299174935,-1.621));
#35659=CARTESIAN_POINT('Ctrl Pts',(5.5,5.21225299174935,-1.621));
#35660=CARTESIAN_POINT('Ctrl Pts',(5.29509392838307,5.21225299174935,-1.621));
#35661=CARTESIAN_POINT('Ctrl Pts',(5.07744240259474,5.22560045988912,-1.57979528744991));
#35662=CARTESIAN_POINT('Ctrl Pts',(4.67846794933173,5.27287962307746,-1.41399911891084));
#35663=CARTESIAN_POINT('Ctrl Pts',(4.49702782444847,5.30603062902532,-1.28946800905525));
#35664=CARTESIAN_POINT('Ctrl Pts',(4.21057289219421,5.36755449841623,-1.00301307680099));
#35665=CARTESIAN_POINT('Ctrl Pts',(4.08601009499387,5.4000554117724,-0.821556304277599));
#35666=CARTESIAN_POINT('Ctrl Pts',(3.92019054985229,5.44582673671694,-0.422521434885201));
#35667=CARTESIAN_POINT('Ctrl Pts',(3.879,5.4585,-0.204847565255781));
#35668=CARTESIAN_POINT('Ctrl Pts',(3.879,5.4585,0.204847565255781));
#35669=CARTESIAN_POINT('Ctrl Pts',(3.92019054985229,5.44582673671694,0.422521434885201));
#35670=CARTESIAN_POINT('Ctrl Pts',(4.08601009499387,5.4000554117724,0.821556304277599));
#35671=CARTESIAN_POINT('Ctrl Pts',(4.21057289219421,5.36755449841623,1.00301307680099));
#35672=CARTESIAN_POINT('Ctrl Pts',(4.49702782444847,5.30603062902532,1.28946800905525));
#35673=CARTESIAN_POINT('Ctrl Pts',(4.67846794933173,5.27287962307746,1.41399911891084));
#35674=CARTESIAN_POINT('Ctrl Pts',(5.07744240259474,5.22560045988912,1.57979528744991));
#35675=CARTESIAN_POINT('Ctrl Pts',(5.29509392838307,5.21225299174935,1.621));
#35676=CARTESIAN_POINT('Ctrl Pts',(5.70490607161693,5.21225299174935,1.621));
#35677=CARTESIAN_POINT('Ctrl Pts',(5.92255759740526,5.22560045988912,1.57979528744991));
#35678=CARTESIAN_POINT('Ctrl Pts',(6.32153205066828,5.27287962307746,1.41399911891084));
#35679=CARTESIAN_POINT('Ctrl Pts',(6.50297217555153,5.30603062902532,1.28946800905525));
#35680=CARTESIAN_POINT('Ctrl Pts',(6.78942710780579,5.36755449841623,1.00301307680099));
#35681=CARTESIAN_POINT('Ctrl Pts',(6.91398990500613,5.4000554117724,0.8215563042776));
#35682=CARTESIAN_POINT('Ctrl Pts',(7.07980945014771,5.44582673671694,0.422521434885203));
#35683=CARTESIAN_POINT('Ctrl Pts',(7.121,5.4585,0.204847565255782));
#35684=CARTESIAN_POINT('Ctrl Pts',(7.121,5.4585,-0.20484756525578));
#35685=CARTESIAN_POINT('Ctrl Pts',(7.07980945014771,5.44582673671694,-0.422521434885202));
#35686=CARTESIAN_POINT('Ctrl Pts',(6.91398990500613,5.4000554117724,-0.821556304277599));
#35687=CARTESIAN_POINT('Ctrl Pts',(6.78942710780579,5.36755449841623,-1.00301307680099));
#35688=CARTESIAN_POINT('Ctrl Pts',(6.50297217555153,5.30603062902532,-1.28946800905525));
#35689=CARTESIAN_POINT('Ctrl Pts',(6.32153205066828,5.27287962307746,-1.41399911891084));
#35690=CARTESIAN_POINT('Ctrl Pts',(5.92255759740526,5.22560045988912,-1.57979528744991));
#35691=CARTESIAN_POINT('Ctrl Pts',(5.70490607161694,5.21225299174935,-1.621));
#35692=CARTESIAN_POINT('Ctrl Pts',(5.5,5.21225299174935,-1.621));
#35693=CARTESIAN_POINT('',(5.5,10.8799062036398,-1.621));
#35694=CARTESIAN_POINT('',(5.5,11.,-1.621));
#35695=CARTESIAN_POINT('Ctrl Pts',(5.5,10.8799062036398,-1.621));
#35696=CARTESIAN_POINT('Ctrl Pts',(5.7038572300951,10.8799062036398,-1.621));
#35697=CARTESIAN_POINT('Ctrl Pts',(5.92109642242532,10.8862276408641,-1.58019820547013));
#35698=CARTESIAN_POINT('Ctrl Pts',(6.32038751501911,10.9089717931152,-1.41467769063433));
#35699=CARTESIAN_POINT('Ctrl Pts',(6.5024652295479,10.9250563808622,-1.28997495505889));
#35700=CARTESIAN_POINT('Ctrl Pts',(6.78997262190052,10.9551791595233,-1.00246756270627));
#35701=CARTESIAN_POINT('Ctrl Pts',(6.91467718754251,10.9711871972319,-0.82038884065458));
#35702=CARTESIAN_POINT('Ctrl Pts',(7.08019903497012,10.9937557707836,-0.421094309383512));
#35703=CARTESIAN_POINT('Ctrl Pts',(7.121,11.,-0.203853921468213));
#35704=CARTESIAN_POINT('Ctrl Pts',(7.121,11.,0.203853921468214));
#35705=CARTESIAN_POINT('Ctrl Pts',(7.08019903497012,10.9937557707836,0.421094309383513));
#35706=CARTESIAN_POINT('Ctrl Pts',(6.91467718754251,10.9711871972319,0.820388840654582));
#35707=CARTESIAN_POINT('Ctrl Pts',(6.78997262190052,10.9551791595233,1.00246756270627));
#35708=CARTESIAN_POINT('Ctrl Pts',(6.5024652295479,10.9250563808622,1.28997495505889));
#35709=CARTESIAN_POINT('Ctrl Pts',(6.32038751501911,10.9089717931152,1.41467769063433));
#35710=CARTESIAN_POINT('Ctrl Pts',(5.92109642242532,10.8862276408641,1.58019820547013));
#35711=CARTESIAN_POINT('Ctrl Pts',(5.7038572300951,10.8799062036398,1.621));
#35712=CARTESIAN_POINT('Ctrl Pts',(5.29614276990491,10.8799062036398,1.621));
#35713=CARTESIAN_POINT('Ctrl Pts',(5.07890357757468,10.8862276408641,1.58019820547013));
#35714=CARTESIAN_POINT('Ctrl Pts',(4.6796124849809,10.9089717931152,1.41467769063433));
#35715=CARTESIAN_POINT('Ctrl Pts',(4.49753477045211,10.9250563808622,1.28997495505889));
#35716=CARTESIAN_POINT('Ctrl Pts',(4.21002737809948,10.9551791595233,1.00246756270627));
#35717=CARTESIAN_POINT('Ctrl Pts',(4.08532281245749,10.9711871972319,0.820388840654582));
#35718=CARTESIAN_POINT('Ctrl Pts',(3.91980096502989,10.9937557707836,0.421094309383513));
#35719=CARTESIAN_POINT('Ctrl Pts',(3.879,11.,0.203853921468214));
#35720=CARTESIAN_POINT('Ctrl Pts',(3.879,11.,-0.203853921468214));
#35721=CARTESIAN_POINT('Ctrl Pts',(3.91980096502989,10.9937557707836,-0.421094309383514));
#35722=CARTESIAN_POINT('Ctrl Pts',(4.08532281245749,10.9711871972319,-0.820388840654582));
#35723=CARTESIAN_POINT('Ctrl Pts',(4.21002737809948,10.9551791595233,-1.00246756270627));
#35724=CARTESIAN_POINT('Ctrl Pts',(4.49753477045211,10.9250563808622,-1.28997495505889));
#35725=CARTESIAN_POINT('Ctrl Pts',(4.6796124849809,10.9089717931152,-1.41467769063433));
#35726=CARTESIAN_POINT('Ctrl Pts',(5.07890357757468,10.8862276408641,-1.58019820547013));
#35727=CARTESIAN_POINT('Ctrl Pts',(5.29614276990491,10.8799062036398,-1.621));
#35728=CARTESIAN_POINT('Ctrl Pts',(5.5,10.8799062036398,-1.621));
#35729=CARTESIAN_POINT('Origin',(7.4585,0.,0.));
#35730=CARTESIAN_POINT('',(7.4585,6.68473455314583E-16,-5.4585));
#35731=CARTESIAN_POINT('',(7.4585,-6.68473455314583E-16,5.4585));
#35732=CARTESIAN_POINT('Origin',(7.4585,0.,0.));
#35733=CARTESIAN_POINT('',(8.,-7.34788079488412E-16,6.));
#35734=CARTESIAN_POINT('',(7.4585,-6.68473455314583E-16,5.4585));
#35735=CARTESIAN_POINT('Origin',(8.,0.,0.));
#35736=CARTESIAN_POINT('Origin',(7.4585,0.,0.));
#35737=CARTESIAN_POINT('Origin',(0.,0.,0.));
#35738=CARTESIAN_POINT('',(0.541500000000001,-6.68473455314583E-16,-5.4585));
#35739=CARTESIAN_POINT('Origin',(0.5415,0.,0.));
#35740=CARTESIAN_POINT('',(-4.6168096649323E-16,-7.34788079488412E-16,-6.));
#35741=CARTESIAN_POINT('',(0.,-7.34788079488412E-16,-6.));
#35742=CARTESIAN_POINT('Origin',(0.,0.,0.));
#35743=CARTESIAN_POINT('Origin',(0.,0.,0.));
#35744=CARTESIAN_POINT('',(0.,-6.68473455314583E-16,-5.4585));
#35745=CARTESIAN_POINT('Origin',(-0.25,0.,0.));
#35746=CARTESIAN_POINT('',(8.,-2.79641763593266,10.6386112066117));
#35747=CARTESIAN_POINT('',(8.,2.79641763593267,10.6386112066117));
#35748=CARTESIAN_POINT('Origin',(8.,0.,0.));
#35749=CARTESIAN_POINT('',(1.,2.79641763593267,10.6386112066117));
#35750=CARTESIAN_POINT('',(-0.25,2.79641763593267,10.6386112066117));
#35751=CARTESIAN_POINT('',(1.,-2.79641763593267,10.6386112066117));
#35752=CARTESIAN_POINT('Origin',(1.,0.,0.));
#35753=CARTESIAN_POINT('',(-0.25,-2.79641763593267,10.6386112066117));
#35754=CARTESIAN_POINT('Origin',(-0.25,0.,0.));
#35755=CARTESIAN_POINT('',(0.,-1.04094977927525E-15,-8.5));
#35756=CARTESIAN_POINT('Origin',(0.,0.,0.));
#35757=CARTESIAN_POINT('',(1.,-1.04094977927525E-15,-8.5));
#35758=CARTESIAN_POINT('',(-0.25,-1.04094977927525E-15,-8.5));
#35759=CARTESIAN_POINT('Origin',(1.,0.,0.));
#35760=CARTESIAN_POINT('Origin',(-0.25,0.,0.));
#35761=CARTESIAN_POINT('',(8.,-10.6386112066117,-2.79641763593268));
#35762=CARTESIAN_POINT('',(8.,-10.6386112066117,2.79641763593267));
#35763=CARTESIAN_POINT('Origin',(8.,0.,0.));
#35764=CARTESIAN_POINT('',(1.,-10.6386112066117,2.79641763593267));
#35765=CARTESIAN_POINT('',(-0.25,-10.6386112066117,2.79641763593267));
#35766=CARTESIAN_POINT('',(1.,-10.6386112066117,-2.79641763593268));
#35767=CARTESIAN_POINT('Origin',(1.,0.,0.));
#35768=CARTESIAN_POINT('',(-0.25,-10.6386112066117,-2.79641763593268));
#35769=CARTESIAN_POINT('Origin',(-0.25,0.,0.));
#35770=CARTESIAN_POINT('',(8.,2.79641763593267,-10.6386112066117));
#35771=CARTESIAN_POINT('',(8.,-2.79641763593268,-10.6386112066117));
#35772=CARTESIAN_POINT('Origin',(8.,0.,0.));
#35773=CARTESIAN_POINT('',(1.,-2.79641763593268,-10.6386112066117));
#35774=CARTESIAN_POINT('',(-0.25,-2.79641763593268,-10.6386112066117));
#35775=CARTESIAN_POINT('',(1.,2.79641763593267,-10.6386112066117));
#35776=CARTESIAN_POINT('Origin',(1.,0.,0.));
#35777=CARTESIAN_POINT('',(-0.25,2.79641763593267,-10.6386112066117));
#35778=CARTESIAN_POINT('Origin',(-0.25,0.,0.));
#35779=CARTESIAN_POINT('',(8.,10.6386112066117,2.79641763593267));
#35780=CARTESIAN_POINT('',(8.,10.6386112066117,-2.79641763593267));
#35781=CARTESIAN_POINT('Origin',(8.,0.,0.));
#35782=CARTESIAN_POINT('',(1.,10.6386112066117,-2.79641763593267));
#35783=CARTESIAN_POINT('',(-0.25,10.6386112066117,-2.79641763593267));
#35784=CARTESIAN_POINT('',(1.,10.6386112066117,2.79641763593267));
#35785=CARTESIAN_POINT('Origin',(1.,0.,0.));
#35786=CARTESIAN_POINT('',(-0.25,10.6386112066117,2.79641763593267));
#35787=CARTESIAN_POINT('Origin',(0.,0.,0.));
#35788=CARTESIAN_POINT('Origin',(1.,8.5,0.));
#35789=CARTESIAN_POINT('',(1.,-2.4675144212722,10.9675144212722));
#35790=CARTESIAN_POINT('',(1.,10.9675144212722,2.4675144212722));
#35791=CARTESIAN_POINT('',(1.,10.9675144212722,-2.4675144212722));
#35792=CARTESIAN_POINT('',(1.,-2.4675144212722,-10.9675144212722));
#35793=CARTESIAN_POINT('Origin',(8.,11.,0.));
#35794=CARTESIAN_POINT('',(8.,-1.2175144212722,12.2175144212722));
#35795=CARTESIAN_POINT('',(8.,-1.2175144212722,-12.2175144212722));
#35796=CARTESIAN_POINT('',(8.,12.2175144212722,-1.2175144212722));
#35797=CARTESIAN_POINT('',(8.,12.2175144212722,1.2175144212722));
#35798=CARTESIAN_POINT('Origin',(8.,13.4350288425444,2.16840434497101E-16));
#35799=CARTESIAN_POINT('Origin',(8.,1.62630325872825E-16,-13.4350288425444));
#35800=CARTESIAN_POINT('Origin',(8.,1.62630325872825E-16,-13.4350288425444));
#35801=CARTESIAN_POINT('Origin',(8.,-13.4350288425444,-2.65629532258949E-15));
#35802=CARTESIAN_POINT('Origin',(5.5,10.8,0.));
#35803=CARTESIAN_POINT('',(5.5,10.8,2.));
#35804=CARTESIAN_POINT('Origin',(5.5,10.8,0.));
#35805=CARTESIAN_POINT('',(5.5,11.,1.8));
#35806=CARTESIAN_POINT('',(5.5,10.8,2.));
#35807=CARTESIAN_POINT('Origin',(5.5,11.,0.));
#35808=CARTESIAN_POINT('Origin',(5.5,6.,0.));
#35809=CARTESIAN_POINT('',(5.5,6.75,2.));
#35810=CARTESIAN_POINT('',(5.5,6.75,-2.));
#35811=CARTESIAN_POINT('Origin',(5.5,6.75,0.));
#35812=CARTESIAN_POINT('',(5.5,6.,-1.25));
#35813=CARTESIAN_POINT('',(5.5,6.,-1.25));
#35814=CARTESIAN_POINT('Origin',(5.5,6.,0.));
#35815=CARTESIAN_POINT('Origin',(5.5,6.75,0.));
#35816=CARTESIAN_POINT('Origin',(5.5,0.,0.));
#35817=CARTESIAN_POINT('',(5.5,0.,2.));
#35818=CARTESIAN_POINT('Origin',(5.5,6.,-1.25));
#35819=CARTESIAN_POINT('Origin',(5.5,11.,0.));
#35820=CARTESIAN_POINT('',(6.5,11.,-0.577350269189626));
#35821=CARTESIAN_POINT('',(5.5,11.,-1.15470053837925));
#35822=CARTESIAN_POINT('',(6.5,11.,-0.577350269189626));
#35823=CARTESIAN_POINT('',(6.5,11.,0.577350269189626));
#35824=CARTESIAN_POINT('',(6.5,11.,0.577350269189626));
#35825=CARTESIAN_POINT('',(5.5,11.,1.15470053837925));
#35826=CARTESIAN_POINT('',(5.5,11.,1.15470053837925));
#35827=CARTESIAN_POINT('',(4.5,11.,0.577350269189625));
#35828=CARTESIAN_POINT('',(4.5,11.,0.577350269189625));
#35829=CARTESIAN_POINT('',(4.5,11.,-0.577350269189626));
#35830=CARTESIAN_POINT('',(4.5,11.,-0.577350269189626));
#35831=CARTESIAN_POINT('',(5.5,11.,-1.15470053837925));
#35832=CARTESIAN_POINT('Origin',(6.5,9.,-0.577350269189626));
#35833=CARTESIAN_POINT('',(5.5,9.,-1.15470053837925));
#35834=CARTESIAN_POINT('',(5.5,9.,-1.15470053837925));
#35835=CARTESIAN_POINT('',(6.5,9.,-0.577350269189626));
#35836=CARTESIAN_POINT('',(6.5,9.,-0.577350269189626));
#35837=CARTESIAN_POINT('',(6.5,9.,-0.577350269189626));
#35838=CARTESIAN_POINT('Origin',(6.5,9.,0.577350269189626));
#35839=CARTESIAN_POINT('',(6.5,9.,0.577350269189626));
#35840=CARTESIAN_POINT('',(6.5,9.,0.577350269189626));
#35841=CARTESIAN_POINT('',(6.5,9.,0.577350269189626));
#35842=CARTESIAN_POINT('Origin',(5.5,9.,1.15470053837925));
#35843=CARTESIAN_POINT('',(5.5,9.,1.15470053837925));
#35844=CARTESIAN_POINT('',(5.5,9.,1.15470053837925));
#35845=CARTESIAN_POINT('',(5.5,9.,1.15470053837925));
#35846=CARTESIAN_POINT('Origin',(4.5,9.,0.577350269189625));
#35847=CARTESIAN_POINT('',(4.5,9.,0.577350269189625));
#35848=CARTESIAN_POINT('',(4.5,9.,0.577350269189625));
#35849=CARTESIAN_POINT('',(4.5,9.,0.577350269189625));
#35850=CARTESIAN_POINT('Origin',(4.5,9.,-0.577350269189626));
#35851=CARTESIAN_POINT('',(4.5,9.,-0.577350269189626));
#35852=CARTESIAN_POINT('',(4.5,9.,-0.577350269189626));
#35853=CARTESIAN_POINT('',(4.5,9.,-0.577350269189626));
#35854=CARTESIAN_POINT('Origin',(5.5,9.,-1.15470053837925));
#35855=CARTESIAN_POINT('',(5.5,9.,-1.15470053837925));
#35856=CARTESIAN_POINT('Origin',(0.,9.,0.));
#35857=CARTESIAN_POINT('',(0.,0.,0.));
#35858=CARTESIAN_POINT('Origin',(-0.25,0.,0.));
#35859=CARTESIAN_POINT('',(-3.81639164714898E-16,-9.49101269339199E-16,
-7.75));
#35860=CARTESIAN_POINT('Origin',(-3.79470760369927E-16,0.,0.));
#35861=CARTESIAN_POINT('',(5.5,-9.49101269339199E-16,-7.75));
#35862=CARTESIAN_POINT('',(-0.25,-9.49101269339199E-16,-7.75));
#35863=CARTESIAN_POINT('Origin',(5.5,0.,0.));
#35864=CARTESIAN_POINT('Origin',(-0.25,0.,0.));
#35865=CARTESIAN_POINT('',(5.5,-7.34788079488412E-16,-6.));
#35866=CARTESIAN_POINT('Origin',(5.5,0.,0.));
#35867=CARTESIAN_POINT('',(0.,-7.34788079488412E-16,-6.));
#35868=CARTESIAN_POINT('',(-0.25,-7.34788079488412E-16,-6.));
#35869=CARTESIAN_POINT('Origin',(0.,0.,0.));
#35870=CARTESIAN_POINT('Origin',(-1.83697019872103E-16,7.75,0.));
#35871=CARTESIAN_POINT('Origin',(5.5,6.,0.));
#35872=CARTESIAN_POINT('',(0.,0.,0.));
#35873=CARTESIAN_POINT('',(6.00000000000009,25.,-3.95337236253702E-15));
#35874=CARTESIAN_POINT('',(27.5,25.,-3.94430452610506E-28));
#35875=CARTESIAN_POINT('',(22.,25.,-3.94430452610506E-28));
#35876=CARTESIAN_POINT('',(0.,0.,0.));
#35877=CARTESIAN_POINT('',(0.,0.,0.));
#35878=CARTESIAN_POINT('Origin',(10.,24.,26.));
#35879=CARTESIAN_POINT('',(10.,-1.77635683940025E-14,21.5));
#35880=CARTESIAN_POINT('Origin',(10.,-1.73472347597681E-14,26.));
#35881=CARTESIAN_POINT('',(10.,24.,21.5));
#35882=CARTESIAN_POINT('',(10.,24.,21.5));
#35883=CARTESIAN_POINT('Origin',(10.,24.,26.));
#35884=CARTESIAN_POINT('Origin',(10.,24.,-26.));
#35885=CARTESIAN_POINT('',(10.,-4.44089209850063E-15,-30.5));
#35886=CARTESIAN_POINT('Origin',(10.,-3.46944695195361E-15,-26.));
#35887=CARTESIAN_POINT('',(10.,24.,-30.5));
#35888=CARTESIAN_POINT('',(10.,24.,-30.5));
#35889=CARTESIAN_POINT('Origin',(10.,24.,-26.));
#35890=CARTESIAN_POINT('Origin',(20.,25.,0.));
#35891=CARTESIAN_POINT('',(20.,25.,-13.));
#35892=CARTESIAN_POINT('Origin',(20.,25.,0.));
#35893=CARTESIAN_POINT('',(0.,25.,-13.));
#35894=CARTESIAN_POINT('',(20.,25.,-13.));
#35895=CARTESIAN_POINT('Origin',(0.,25.,0.));
#35896=CARTESIAN_POINT('Origin',(20.,0.,0.));
#35897=CARTESIAN_POINT('',(20.,24.,18.0000000000001));
#35898=CARTESIAN_POINT('',(20.,24.,34.5));
#35899=CARTESIAN_POINT('',(20.,24.,18.0000000000001));
#35900=CARTESIAN_POINT('',(20.,23.5,35.));
#35901=CARTESIAN_POINT('',(20.,24.,34.5));
#35902=CARTESIAN_POINT('',(20.,7.70371977754894E-31,35.));
#35903=CARTESIAN_POINT('',(20.,23.5,35.));
#35904=CARTESIAN_POINT('',(20.,1.78732264387927E-14,-35.));
#35905=CARTESIAN_POINT('',(20.,7.70371977754894E-31,35.));
#35906=CARTESIAN_POINT('',(20.,23.5,-35.));
#35907=CARTESIAN_POINT('',(20.,23.5,-35.));
#35908=CARTESIAN_POINT('',(20.,24.,-34.5));
#35909=CARTESIAN_POINT('',(20.,24.,-34.5));
#35910=CARTESIAN_POINT('',(20.,24.,-17.9999999999999));
#35911=CARTESIAN_POINT('',(20.,24.,-17.9999999999999));
#35912=CARTESIAN_POINT('',(20.,42.5,-17.9999999999999));
#35913=CARTESIAN_POINT('',(20.,42.5,-17.9999999999999));
#35914=CARTESIAN_POINT('',(20.,43.,-17.4999999999999));
#35915=CARTESIAN_POINT('',(20.,43.,-17.4999999999999));
#35916=CARTESIAN_POINT('',(20.,43.,17.5));
#35917=CARTESIAN_POINT('',(20.,43.,17.5));
#35918=CARTESIAN_POINT('',(20.,42.5,18.0000000000001));
#35919=CARTESIAN_POINT('',(20.,42.5,18.0000000000001));
#35920=CARTESIAN_POINT('',(20.,42.5,18.0000000000001));
#35921=CARTESIAN_POINT('Origin',(0.,0.,0.));
#35922=CARTESIAN_POINT('',(0.,24.,18.0000000000001));
#35923=CARTESIAN_POINT('',(0.,24.,34.5));
#35924=CARTESIAN_POINT('',(0.,24.,18.0000000000001));
#35925=CARTESIAN_POINT('',(0.,42.5,18.0000000000001));
#35926=CARTESIAN_POINT('',(0.,42.5,18.0000000000001));
#35927=CARTESIAN_POINT('',(0.,43.,17.5));
#35928=CARTESIAN_POINT('',(0.,42.5,18.0000000000001));
#35929=CARTESIAN_POINT('',(0.,43.,-17.4999999999999));
#35930=CARTESIAN_POINT('',(0.,43.,17.5));
#35931=CARTESIAN_POINT('',(0.,42.5,-17.9999999999999));
#35932=CARTESIAN_POINT('',(0.,43.,-17.4999999999999));
#35933=CARTESIAN_POINT('',(0.,24.,-17.9999999999999));
#35934=CARTESIAN_POINT('',(0.,42.5,-17.9999999999999));
#35935=CARTESIAN_POINT('',(0.,24.,-34.5));
#35936=CARTESIAN_POINT('',(0.,24.,-17.9999999999999));
#35937=CARTESIAN_POINT('',(0.,23.5,-35.));
#35938=CARTESIAN_POINT('',(0.,24.,-34.5));
#35939=CARTESIAN_POINT('',(0.,1.78732264387927E-14,-35.));
#35940=CARTESIAN_POINT('',(0.,23.5,-35.));
#35941=CARTESIAN_POINT('',(0.,7.70371977754894E-31,35.));
#35942=CARTESIAN_POINT('',(0.,7.70371977754894E-31,35.));
#35943=CARTESIAN_POINT('',(0.,23.5,35.));
#35944=CARTESIAN_POINT('',(0.,23.5,35.));
#35945=CARTESIAN_POINT('',(0.,24.,34.5));
#35946=CARTESIAN_POINT('Origin',(20.,24.,18.0000000000001));
#35947=CARTESIAN_POINT('',(20.,24.,34.5));
#35948=CARTESIAN_POINT('',(20.,24.,18.0000000000001));
#35949=CARTESIAN_POINT('Origin',(20.,24.,34.5));
#35950=CARTESIAN_POINT('',(20.,23.5,35.));
#35951=CARTESIAN_POINT('Origin',(20.,23.5,35.));
#35952=CARTESIAN_POINT('',(20.,7.70371977754894E-31,35.));
#35953=CARTESIAN_POINT('Origin',(20.,7.70371977754894E-31,35.));
#35954=CARTESIAN_POINT('',(20.,1.78732264387927E-14,-35.));
#35955=CARTESIAN_POINT('Origin',(20.,23.5,-35.));
#35956=CARTESIAN_POINT('',(20.,23.5,-35.));
#35957=CARTESIAN_POINT('Origin',(20.,24.,-34.5));
#35958=CARTESIAN_POINT('',(20.,24.,-34.5));
#35959=CARTESIAN_POINT('Origin',(20.,24.,-17.9999999999999));
#35960=CARTESIAN_POINT('',(20.,24.,-17.9999999999999));
#35961=CARTESIAN_POINT('Origin',(20.,42.5,-17.9999999999999));
#35962=CARTESIAN_POINT('',(20.,42.5,-17.9999999999999));
#35963=CARTESIAN_POINT('Origin',(20.,43.,-17.4999999999999));
#35964=CARTESIAN_POINT('',(20.,43.,-17.4999999999999));
#35965=CARTESIAN_POINT('Origin',(20.,43.,17.5));
#35966=CARTESIAN_POINT('',(20.,43.,17.5));
#35967=CARTESIAN_POINT('Origin',(20.,42.5,18.0000000000001));
#35968=CARTESIAN_POINT('',(20.,42.5,18.0000000000001));
#35969=CARTESIAN_POINT('Origin',(20.,42.5,18.0000000000001));
#35970=CARTESIAN_POINT('Origin',(13.7,25.,0.));
#35971=CARTESIAN_POINT('',(14.,30.3,-6.49062803548096E-16));
#35972=CARTESIAN_POINT('Origin',(14.,25.,0.));
#35973=CARTESIAN_POINT('',(13.7,30.,-6.12323399573676E-16));
#35974=CARTESIAN_POINT('Origin',(13.7,30.3,-6.49062803548097E-16));
#35975=CARTESIAN_POINT('Origin',(13.7,25.,0.));
#35976=CARTESIAN_POINT('Origin',(0.,25.,0.));
#35977=CARTESIAN_POINT('',(6.3,30.,-6.12323399573676E-16));
#35978=CARTESIAN_POINT('',(-8.67361737988403E-16,30.,-6.12323399573676E-16));
#35979=CARTESIAN_POINT('Origin',(6.3,25.,0.));
#35980=CARTESIAN_POINT('Origin',(6.3,25.,0.));
#35981=CARTESIAN_POINT('',(6.,30.3,-6.49062803548097E-16));
#35982=CARTESIAN_POINT('Origin',(6.3,30.3,-6.49062803548097E-16));
#35983=CARTESIAN_POINT('Origin',(6.,25.,0.));
#35984=CARTESIAN_POINT('Origin',(0.,25.,0.));
#35985=CARTESIAN_POINT('',(6.,31.7,-8.20513355428726E-16));
#35986=CARTESIAN_POINT('Origin',(6.,25.,0.));
#35987=CARTESIAN_POINT('',(6.45,31.7,-8.20513355428726E-16));
#35988=CARTESIAN_POINT('',(-1.16226472890446E-15,31.7,-8.20513355428726E-16));
#35989=CARTESIAN_POINT('Origin',(6.45,25.,0.));
#35990=CARTESIAN_POINT('Origin',(0.,25.,0.));
#35991=CARTESIAN_POINT('',(6.45,34.8,-1.20015386316441E-15));
#35992=CARTESIAN_POINT('Origin',(6.45,25.,0.));
#35993=CARTESIAN_POINT('',(6.,34.8,-1.20015386316441E-15));
#35994=CARTESIAN_POINT('',(-1.70002900645727E-15,34.8,-1.20015386316441E-15));
#35995=CARTESIAN_POINT('Origin',(6.,25.,0.));
#35996=CARTESIAN_POINT('Origin',(6.3,25.,0.));
#35997=CARTESIAN_POINT('',(6.,37.7,-1.55530143491714E-15));
#35998=CARTESIAN_POINT('Origin',(6.,25.,0.));
#35999=CARTESIAN_POINT('',(6.3,38.,-1.59204083889156E-15));
#36000=CARTESIAN_POINT('Origin',(6.3,37.7,-1.55530143491714E-15));
#36001=CARTESIAN_POINT('Origin',(6.3,25.,0.));
#36002=CARTESIAN_POINT('Origin',(0.,25.,0.));
#36003=CARTESIAN_POINT('',(13.7,38.,-1.59204083889156E-15));
#36004=CARTESIAN_POINT('',(-2.25514051876985E-15,38.,-1.59204083889156E-15));
#36005=CARTESIAN_POINT('Origin',(13.7,25.,0.));
#36006=CARTESIAN_POINT('Origin',(13.7,25.,0.));
#36007=CARTESIAN_POINT('',(14.,37.7,-1.55530143491714E-15));
#36008=CARTESIAN_POINT('Origin',(13.7,37.7,-1.55530143491714E-15));
#36009=CARTESIAN_POINT('Origin',(14.,25.,0.));
#36010=CARTESIAN_POINT('Origin',(0.,25.,0.));
#36011=CARTESIAN_POINT('',(14.,34.8,-1.20015386316441E-15));
#36012=CARTESIAN_POINT('Origin',(14.,25.,0.));
#36013=CARTESIAN_POINT('',(13.55,34.8,-1.20015386316441E-15));
#36014=CARTESIAN_POINT('',(-1.70002900645727E-15,34.8,-1.20015386316441E-15));
#36015=CARTESIAN_POINT('Origin',(13.55,25.,0.));
#36016=CARTESIAN_POINT('Origin',(0.,25.,0.));
#36017=CARTESIAN_POINT('',(13.55,31.7,-8.20513355428726E-16));
#36018=CARTESIAN_POINT('Origin',(13.55,25.,0.));
#36019=CARTESIAN_POINT('',(14.,31.7,-8.20513355428726E-16));
#36020=CARTESIAN_POINT('',(-1.16226472890446E-15,31.7,-8.20513355428726E-16));
#36021=CARTESIAN_POINT('Origin',(14.,25.,0.));
#36022=CARTESIAN_POINT('Origin',(13.55,31.7,0.));
#36023=CARTESIAN_POINT('Origin',(14.,34.8,0.));
#36024=CARTESIAN_POINT('Origin',(6.,37.7,0.));
#36025=CARTESIAN_POINT('Origin',(6.45,34.8,0.));
#36026=CARTESIAN_POINT('Origin',(6.,31.7,0.));
#36027=CARTESIAN_POINT('Origin',(14.,30.3,0.));
#36028=CARTESIAN_POINT('',(0.,0.,0.));
#36029=CARTESIAN_POINT('Origin',(1.,-6.65,2.1));
#36030=CARTESIAN_POINT('',(1.,-6.65,1.5));
#36031=CARTESIAN_POINT('Origin',(1.,-6.65,2.1));
#36032=CARTESIAN_POINT('',(0.,-6.65,1.5));
#36033=CARTESIAN_POINT('',(1.,-6.65,1.5));
#36034=CARTESIAN_POINT('Origin',(0.,-6.65,2.1));
#36035=CARTESIAN_POINT('Origin',(1.,-6.65,-2.1));
#36036=CARTESIAN_POINT('',(1.,-6.65,-2.7));
#36037=CARTESIAN_POINT('Origin',(1.,-6.65,-2.1));
#36038=CARTESIAN_POINT('',(0.,-6.65,-2.7));
#36039=CARTESIAN_POINT('',(1.,-6.65,-2.7));
#36040=CARTESIAN_POINT('Origin',(0.,-6.65,-2.1));
#36041=CARTESIAN_POINT('Origin',(1.,-0.45,0.));
#36042=CARTESIAN_POINT('',(1.,-5.23330429724056,0.400000000000003));
#36043=CARTESIAN_POINT('',(1.,-5.23330429724056,-0.4));
#36044=CARTESIAN_POINT('Origin',(1.,-0.45,0.));
#36045=CARTESIAN_POINT('',(0.,-5.23330429724056,0.400000000000003));
#36046=CARTESIAN_POINT('',(1.,-5.23330429724056,0.400000000000003));
#36047=CARTESIAN_POINT('',(0.,-5.23330429724056,-0.4));
#36048=CARTESIAN_POINT('Origin',(0.,-0.45,0.));
#36049=CARTESIAN_POINT('',(1.,-5.23330429724056,-0.4));
#36050=CARTESIAN_POINT('Origin',(1.,2.60208521396521E-15,2.71050543121376E-16));
#36051=CARTESIAN_POINT('',(1.,-4.48705828929949,-4.2058064516129));
#36052=CARTESIAN_POINT('',(1.,-4.48705828929949,4.2058064516129));
#36053=CARTESIAN_POINT('Origin',(1.,2.60208521396521E-15,2.71050543121376E-16));
#36054=CARTESIAN_POINT('',(0.,-4.48705828929949,-4.2058064516129));
#36055=CARTESIAN_POINT('',(1.,-4.48705828929949,-4.2058064516129));
#36056=CARTESIAN_POINT('',(0.,-4.48705828929949,4.2058064516129));
#36057=CARTESIAN_POINT('Origin',(0.,2.60208521396521E-15,2.71050543121376E-16));
#36058=CARTESIAN_POINT('',(1.,-4.48705828929949,4.2058064516129));
#36059=CARTESIAN_POINT('Origin',(1.,-0.45,0.));
#36060=CARTESIAN_POINT('',(1.,-8.25,-0.4));
#36061=CARTESIAN_POINT('',(1.,-8.25,-2.1));
#36062=CARTESIAN_POINT('',(1.,-8.25,-2.1));
#36063=CARTESIAN_POINT('',(1.,-6.65,-3.7));
#36064=CARTESIAN_POINT('Origin',(1.,-6.65,-2.1));
#36065=CARTESIAN_POINT('',(1.,-5.65442304749123,-3.7));
#36066=CARTESIAN_POINT('',(1.,-5.65442304749123,-3.7));
#36067=CARTESIAN_POINT('Origin',(1.,-5.65442304749123,-5.3));
#36068=CARTESIAN_POINT('',(1.,-5.65442304749123,3.7));
#36069=CARTESIAN_POINT('Origin',(1.,-5.65442304749123,5.3));
#36070=CARTESIAN_POINT('',(1.,-6.65,3.7));
#36071=CARTESIAN_POINT('',(1.,-5.65442304749123,3.7));
#36072=CARTESIAN_POINT('',(1.,-8.25,2.1));
#36073=CARTESIAN_POINT('Origin',(1.,-6.65,2.1));
#36074=CARTESIAN_POINT('',(1.,-8.25,0.4));
#36075=CARTESIAN_POINT('',(1.,-8.25,2.1));
#36076=CARTESIAN_POINT('',(1.,-5.23330429724056,0.4));
#36077=CARTESIAN_POINT('',(1.,-5.23330429724056,-0.4));
#36078=CARTESIAN_POINT('Origin',(0.,-0.45,0.));
#36079=CARTESIAN_POINT('',(0.,-8.25,-0.4));
#36080=CARTESIAN_POINT('',(0.,-8.25,-2.1));
#36081=CARTESIAN_POINT('',(0.,-8.25,-2.1));
#36082=CARTESIAN_POINT('',(0.,-5.23330429724056,-0.4));
#36083=CARTESIAN_POINT('',(0.,-8.25,0.4));
#36084=CARTESIAN_POINT('',(0.,-5.23330429724056,0.4));
#36085=CARTESIAN_POINT('',(0.,-8.25,2.1));
#36086=CARTESIAN_POINT('',(0.,-8.25,2.1));
#36087=CARTESIAN_POINT('',(0.,-6.65,3.7));
#36088=CARTESIAN_POINT('Origin',(0.,-6.65,2.1));
#36089=CARTESIAN_POINT('',(0.,-5.65442304749123,3.7));
#36090=CARTESIAN_POINT('',(0.,-5.65442304749123,3.7));
#36091=CARTESIAN_POINT('Origin',(0.,-5.65442304749123,5.3));
#36092=CARTESIAN_POINT('',(0.,-5.65442304749123,-3.7));
#36093=CARTESIAN_POINT('Origin',(0.,-5.65442304749123,-5.3));
#36094=CARTESIAN_POINT('',(0.,-6.65,-3.7));
#36095=CARTESIAN_POINT('',(0.,-5.65442304749123,-3.7));
#36096=CARTESIAN_POINT('Origin',(0.,-6.65,-2.1));
#36097=CARTESIAN_POINT('Origin',(1.,-8.25,-2.1));
#36098=CARTESIAN_POINT('',(1.,-8.25,-2.1));
#36099=CARTESIAN_POINT('',(1.,-8.25,-0.4));
#36100=CARTESIAN_POINT('Origin',(1.,-6.65,-2.1));
#36101=CARTESIAN_POINT('',(1.,-6.65,-3.7));
#36102=CARTESIAN_POINT('Origin',(1.,-5.65442304749123,-3.7));
#36103=CARTESIAN_POINT('',(1.,-5.65442304749123,-3.7));
#36104=CARTESIAN_POINT('Origin',(1.,-5.65442304749123,-5.3));
#36105=CARTESIAN_POINT('Origin',(1.,-5.65442304749123,5.3));
#36106=CARTESIAN_POINT('',(1.,-5.65442304749123,3.7));
#36107=CARTESIAN_POINT('Origin',(1.,-5.65442304749123,3.7));
#36108=CARTESIAN_POINT('',(1.,-6.65,3.7));
#36109=CARTESIAN_POINT('Origin',(1.,-6.65,2.1));
#36110=CARTESIAN_POINT('',(1.,-8.25,2.1));
#36111=CARTESIAN_POINT('Origin',(1.,-8.25,2.1));
#36112=CARTESIAN_POINT('',(1.,-8.25,0.4));
#36113=CARTESIAN_POINT('Origin',(1.,-5.23330429724056,0.4));
#36114=CARTESIAN_POINT('Origin',(1.,-5.23330429724056,-0.4));
#36115=CARTESIAN_POINT('',(0.,0.,0.));
#36116=CARTESIAN_POINT('',(6.00000000000001,25.45,4.90783830730734E-17));
#36117=CARTESIAN_POINT('',(0.,0.,0.));
#36118=CARTESIAN_POINT('Origin',(-13.5,0.5,1.));
#36119=CARTESIAN_POINT('',(-16.5,0.5,-4.));
#36120=CARTESIAN_POINT('Origin',(-13.5,0.5,-4.));
#36121=CARTESIAN_POINT('',(-16.5,0.5,1.));
#36122=CARTESIAN_POINT('',(-16.5,0.5,1.));
#36123=CARTESIAN_POINT('Origin',(-13.5,0.5,1.));
#36124=CARTESIAN_POINT('Origin',(11.5,0.5,1.));
#36125=CARTESIAN_POINT('',(8.5,0.5,-4.));
#36126=CARTESIAN_POINT('Origin',(11.5,0.5,-4.));
#36127=CARTESIAN_POINT('',(8.5,0.5,1.));
#36128=CARTESIAN_POINT('',(8.5,0.5,1.));
#36129=CARTESIAN_POINT('Origin',(11.5,0.5,1.));
#36130=CARTESIAN_POINT('Origin',(-27.,0.5,-4.));
#36131=CARTESIAN_POINT('',(-31.25,0.499999999999999,-4.));
#36132=CARTESIAN_POINT('Origin',(-27.,0.5,-4.));
#36133=CARTESIAN_POINT('',(-31.25,0.499999999999999,1.));
#36134=CARTESIAN_POINT('',(-31.25,0.499999999999999,-4.));
#36135=CARTESIAN_POINT('Origin',(-27.,0.5,1.));
#36136=CARTESIAN_POINT('Origin',(25.,0.5,-4.));
#36137=CARTESIAN_POINT('',(20.75,0.499999999999999,-4.));
#36138=CARTESIAN_POINT('Origin',(25.,0.5,-4.));
#36139=CARTESIAN_POINT('',(20.75,0.499999999999999,1.));
#36140=CARTESIAN_POINT('',(20.75,0.499999999999999,-4.));
#36141=CARTESIAN_POINT('Origin',(25.,0.5,1.));
#36142=CARTESIAN_POINT('Origin',(0.,0.,4.));
#36143=CARTESIAN_POINT('',(34.,-3.5,4.));
#36144=CARTESIAN_POINT('',(34.,13.5,4.));
#36145=CARTESIAN_POINT('',(34.,13.5,4.));
#36146=CARTESIAN_POINT('',(36.5,-3.5,4.));
#36147=CARTESIAN_POINT('',(34.,-3.5,4.));
#36148=CARTESIAN_POINT('',(36.5,13.5,4.));
#36149=CARTESIAN_POINT('',(36.5,13.5,4.));
#36150=CARTESIAN_POINT('',(-36.5,13.5,4.));
#36151=CARTESIAN_POINT('Origin',(36.5,13.5,4.));
#36152=CARTESIAN_POINT('',(36.5,-3.5,1.));
#36153=CARTESIAN_POINT('',(36.5,-3.5,1.));
#36154=CARTESIAN_POINT('',(36.5,-13.5,1.));
#36155=CARTESIAN_POINT('',(36.5,-13.5,1.));
#36156=CARTESIAN_POINT('',(36.5,-13.5,-4.));
#36157=CARTESIAN_POINT('',(36.5,-13.5,4.));
#36158=CARTESIAN_POINT('',(36.5,13.5,-4.));
#36159=CARTESIAN_POINT('',(36.5,13.5,-4.));
#36160=CARTESIAN_POINT('',(36.5,13.5,4.));
#36161=CARTESIAN_POINT('Origin',(-36.5,13.5,4.));
#36162=CARTESIAN_POINT('',(34.,13.5,1.));
#36163=CARTESIAN_POINT('',(-36.5,13.5,1.));
#36164=CARTESIAN_POINT('',(-36.5,13.5,1.));
#36165=CARTESIAN_POINT('',(34.,13.5,1.));
#36166=CARTESIAN_POINT('',(-36.5,13.5,-4.));
#36167=CARTESIAN_POINT('',(-36.5,13.5,-4.));
#36168=CARTESIAN_POINT('',(-36.5,13.5,4.));
#36169=CARTESIAN_POINT('Origin',(-36.5,13.5,4.));
#36170=CARTESIAN_POINT('',(-36.5,-11.5,4.));
#36171=CARTESIAN_POINT('',(-36.5,-13.5,4.));
#36172=CARTESIAN_POINT('',(-36.5,13.5,4.));
#36173=CARTESIAN_POINT('',(-36.5,-11.5,1.));
#36174=CARTESIAN_POINT('',(-36.5,-11.5,1.));
#36175=CARTESIAN_POINT('',(-36.5,13.5,1.));
#36176=CARTESIAN_POINT('',(-36.5,-13.5,-4.));
#36177=CARTESIAN_POINT('',(-36.5,13.5,-4.));
#36178=CARTESIAN_POINT('',(-36.5,-13.5,4.));
#36179=CARTESIAN_POINT('Origin',(-36.5,-13.5,4.));
#36180=CARTESIAN_POINT('',(16.5,-13.5,1.));
#36181=CARTESIAN_POINT('',(16.5,-13.5,1.));
#36182=CARTESIAN_POINT('',(16.5,-13.5,4.));
#36183=CARTESIAN_POINT('',(16.5,-13.5,1.));
#36184=CARTESIAN_POINT('',(-36.5,-13.5,4.));
#36185=CARTESIAN_POINT('',(-36.5,-13.5,-4.));
#36186=CARTESIAN_POINT('Origin',(0.,0.,4.));
#36187=CARTESIAN_POINT('',(16.5,-11.5,4.));
#36188=CARTESIAN_POINT('',(16.5,-11.5,4.));
#36189=CARTESIAN_POINT('',(-36.5,-11.5,4.));
#36190=CARTESIAN_POINT('Origin',(0.,0.,-4.));
#36191=CARTESIAN_POINT('Origin',(34.,13.5,1.));
#36192=CARTESIAN_POINT('',(34.,-3.5,1.));
#36193=CARTESIAN_POINT('',(34.,13.5,1.));
#36194=CARTESIAN_POINT('',(34.,-3.5,1.));
#36195=CARTESIAN_POINT('Origin',(34.,-3.5,1.));
#36196=CARTESIAN_POINT('',(34.,-3.5,1.));
#36197=CARTESIAN_POINT('Origin',(16.5,-11.5,1.));
#36198=CARTESIAN_POINT('',(16.5,-11.5,1.));
#36199=CARTESIAN_POINT('',(16.5,-11.5,1.));
#36200=CARTESIAN_POINT('',(16.5,-11.5,1.));
#36201=CARTESIAN_POINT('Origin',(-36.5,-11.5,1.));
#36202=CARTESIAN_POINT('',(-36.5,-11.5,1.));
#36203=CARTESIAN_POINT('Origin',(0.,0.,1.));
#36204=CARTESIAN_POINT('',(0.,0.,0.));
#36205=CARTESIAN_POINT('Origin',(-13.5,0.5,1.));
#36206=CARTESIAN_POINT('',(-16.5,0.5,-4.));
#36207=CARTESIAN_POINT('Origin',(-13.5,0.5,-4.));
#36208=CARTESIAN_POINT('',(-16.5,0.5,1.));
#36209=CARTESIAN_POINT('',(-16.5,0.5,1.));
#36210=CARTESIAN_POINT('Origin',(-13.5,0.5,1.));
#36211=CARTESIAN_POINT('Origin',(11.5,0.5,1.));
#36212=CARTESIAN_POINT('',(8.5,0.5,-4.));
#36213=CARTESIAN_POINT('Origin',(11.5,0.5,-4.));
#36214=CARTESIAN_POINT('',(8.5,0.5,1.));
#36215=CARTESIAN_POINT('',(8.5,0.5,1.));
#36216=CARTESIAN_POINT('Origin',(11.5,0.5,1.));
#36217=CARTESIAN_POINT('Origin',(-27.,0.5,-4.));
#36218=CARTESIAN_POINT('',(-31.25,0.499999999999999,-4.));
#36219=CARTESIAN_POINT('Origin',(-27.,0.5,-4.));
#36220=CARTESIAN_POINT('',(-31.25,0.499999999999999,1.));
#36221=CARTESIAN_POINT('',(-31.25,0.499999999999999,-4.));
#36222=CARTESIAN_POINT('Origin',(-27.,0.5,1.));
#36223=CARTESIAN_POINT('Origin',(25.,0.5,-4.));
#36224=CARTESIAN_POINT('',(20.75,0.5,-4.));
#36225=CARTESIAN_POINT('Origin',(25.,0.5,-4.));
#36226=CARTESIAN_POINT('',(20.75,0.5,1.));
#36227=CARTESIAN_POINT('',(20.75,0.5,-4.));
#36228=CARTESIAN_POINT('Origin',(25.,0.5,1.));
#36229=CARTESIAN_POINT('Origin',(0.,0.,4.));
#36230=CARTESIAN_POINT('',(34.,-1.5,4.));
#36231=CARTESIAN_POINT('',(34.,11.5,4.));
#36232=CARTESIAN_POINT('',(34.,11.5,4.));
#36233=CARTESIAN_POINT('',(36.5,-1.5,4.));
#36234=CARTESIAN_POINT('',(34.,-1.5,4.));
#36235=CARTESIAN_POINT('',(36.5,11.5,4.));
#36236=CARTESIAN_POINT('',(36.5,11.5,4.));
#36237=CARTESIAN_POINT('',(-36.5,11.5,4.));
#36238=CARTESIAN_POINT('Origin',(36.5,11.5,4.));
#36239=CARTESIAN_POINT('',(36.5,-1.5,1.));
#36240=CARTESIAN_POINT('',(36.5,-1.5,1.));
#36241=CARTESIAN_POINT('',(36.5,-11.5,1.));
#36242=CARTESIAN_POINT('',(36.5,-11.5,1.));
#36243=CARTESIAN_POINT('',(36.5,-11.5,-4.));
#36244=CARTESIAN_POINT('',(36.5,-11.5,4.));
#36245=CARTESIAN_POINT('',(36.5,11.5,-4.));
#36246=CARTESIAN_POINT('',(36.5,11.5,-4.));
#36247=CARTESIAN_POINT('',(36.5,11.5,4.));
#36248=CARTESIAN_POINT('Origin',(-36.5,11.5,4.));
#36249=CARTESIAN_POINT('',(34.,11.5,1.));
#36250=CARTESIAN_POINT('',(-36.5,11.5,1.));
#36251=CARTESIAN_POINT('',(-36.5,11.5,1.));
#36252=CARTESIAN_POINT('',(34.,11.5,1.));
#36253=CARTESIAN_POINT('',(-36.5,11.5,-4.));
#36254=CARTESIAN_POINT('',(-36.5,11.5,-4.));
#36255=CARTESIAN_POINT('',(-36.5,11.5,4.));
#36256=CARTESIAN_POINT('Origin',(-36.5,11.5,4.));
#36257=CARTESIAN_POINT('',(-36.5,-9.5,4.));
#36258=CARTESIAN_POINT('',(-36.5,-11.5,4.));
#36259=CARTESIAN_POINT('',(-36.5,11.5,4.));
#36260=CARTESIAN_POINT('',(-36.5,-9.5,1.));
#36261=CARTESIAN_POINT('',(-36.5,-9.5,1.));
#36262=CARTESIAN_POINT('',(-36.5,11.5,1.));
#36263=CARTESIAN_POINT('',(-36.5,-11.5,-4.));
#36264=CARTESIAN_POINT('',(-36.5,11.5,-4.));
#36265=CARTESIAN_POINT('',(-36.5,-11.5,4.));
#36266=CARTESIAN_POINT('Origin',(-36.5,-11.5,4.));
#36267=CARTESIAN_POINT('',(16.5,-11.5,1.));
#36268=CARTESIAN_POINT('',(16.5,-11.5,1.));
#36269=CARTESIAN_POINT('',(16.5,-11.5,4.));
#36270=CARTESIAN_POINT('',(16.5,-11.5,1.));
#36271=CARTESIAN_POINT('',(-36.5,-11.5,4.));
#36272=CARTESIAN_POINT('',(-36.5,-11.5,-4.));
#36273=CARTESIAN_POINT('Origin',(0.,0.,4.));
#36274=CARTESIAN_POINT('',(16.5,-9.5,4.));
#36275=CARTESIAN_POINT('',(16.5,-9.5,4.));
#36276=CARTESIAN_POINT('',(-36.5,-9.5,4.));
#36277=CARTESIAN_POINT('Origin',(0.,0.,-4.));
#36278=CARTESIAN_POINT('Origin',(34.,11.5,1.));
#36279=CARTESIAN_POINT('',(34.,-1.5,1.));
#36280=CARTESIAN_POINT('',(34.,11.5,1.));
#36281=CARTESIAN_POINT('',(34.,-1.5,1.));
#36282=CARTESIAN_POINT('Origin',(34.,-1.5,1.));
#36283=CARTESIAN_POINT('',(34.,-1.5,1.));
#36284=CARTESIAN_POINT('Origin',(16.5,-9.5,1.));
#36285=CARTESIAN_POINT('',(16.5,-9.5,1.));
#36286=CARTESIAN_POINT('',(16.5,-9.5,1.));
#36287=CARTESIAN_POINT('',(16.5,-9.5,1.));
#36288=CARTESIAN_POINT('Origin',(-36.5,-9.5,1.));
#36289=CARTESIAN_POINT('',(-36.5,-9.5,1.));
#36290=CARTESIAN_POINT('Origin',(0.,0.,1.));
#36291=CARTESIAN_POINT('',(0.,0.,0.));
#36292=CARTESIAN_POINT('Origin',(-24.7487373415288,22.2487373415298,5.));
#36293=CARTESIAN_POINT('',(-26.3987373415288,22.2487373415298,-5.));
#36294=CARTESIAN_POINT('Origin',(-24.7487373415288,22.2487373415298,-5.));
#36295=CARTESIAN_POINT('',(-26.3987373415288,22.2487373415298,5.));
#36296=CARTESIAN_POINT('',(-26.3987373415288,22.2487373415298,5.));
#36297=CARTESIAN_POINT('Origin',(-24.7487373415288,22.2487373415298,5.));
#36298=CARTESIAN_POINT('Origin',(-24.7487373415293,-27.2487373415288,5.));
#36299=CARTESIAN_POINT('',(-26.3987373415293,-27.2487373415288,-5.));
#36300=CARTESIAN_POINT('Origin',(-24.7487373415293,-27.2487373415288,-5.));
#36301=CARTESIAN_POINT('',(-26.3987373415293,-27.2487373415288,5.));
#36302=CARTESIAN_POINT('',(-26.3987373415293,-27.2487373415288,5.));
#36303=CARTESIAN_POINT('Origin',(-24.7487373415293,-27.2487373415288,5.));
#36304=CARTESIAN_POINT('Origin',(24.7487373415289,-27.2487373415291,5.));
#36305=CARTESIAN_POINT('',(23.0987373415289,-27.2487373415291,-5.));
#36306=CARTESIAN_POINT('Origin',(24.7487373415289,-27.2487373415291,-5.));
#36307=CARTESIAN_POINT('',(23.0987373415289,-27.2487373415291,5.));
#36308=CARTESIAN_POINT('',(23.0987373415289,-27.2487373415291,5.));
#36309=CARTESIAN_POINT('Origin',(24.7487373415289,-27.2487373415291,5.));
#36310=CARTESIAN_POINT('Origin',(24.7487373415293,22.2487373415293,5.));
#36311=CARTESIAN_POINT('',(23.0987373415293,22.2487373415293,-5.));
#36312=CARTESIAN_POINT('Origin',(24.7487373415293,22.2487373415293,-5.));
#36313=CARTESIAN_POINT('',(23.0987373415293,22.2487373415293,5.));
#36314=CARTESIAN_POINT('',(23.0987373415293,22.2487373415293,5.));
#36315=CARTESIAN_POINT('Origin',(24.7487373415293,22.2487373415293,5.));
#36316=CARTESIAN_POINT('Origin',(-10.,35.,5.));
#36317=CARTESIAN_POINT('',(-13.,35.,-5.));
#36318=CARTESIAN_POINT('Origin',(-10.,35.,-5.));
#36319=CARTESIAN_POINT('',(-13.,35.,5.));
#36320=CARTESIAN_POINT('',(-13.,35.,5.));
#36321=CARTESIAN_POINT('Origin',(-10.,35.,5.));
#36322=CARTESIAN_POINT('Origin',(10.,35.,5.));
#36323=CARTESIAN_POINT('',(7.,35.,-5.));
#36324=CARTESIAN_POINT('Origin',(10.,35.,-5.));
#36325=CARTESIAN_POINT('',(7.,35.,5.));
#36326=CARTESIAN_POINT('',(7.,35.,5.));
#36327=CARTESIAN_POINT('Origin',(10.,35.,5.));
#36328=CARTESIAN_POINT('Origin',(-24.,35.,5.));
#36329=CARTESIAN_POINT('',(-29.5,35.,-1.4));
#36330=CARTESIAN_POINT('Origin',(-24.,35.,-1.4));
#36331=CARTESIAN_POINT('',(-29.5,35.,5.));
#36332=CARTESIAN_POINT('',(-29.5,35.,5.));
#36333=CARTESIAN_POINT('Origin',(-24.,35.,5.));
#36334=CARTESIAN_POINT('Origin',(-24.,35.,5.));
#36335=CARTESIAN_POINT('',(-27.3,35.,-5.));
#36336=CARTESIAN_POINT('Origin',(-24.,35.,-5.));
#36337=CARTESIAN_POINT('',(-27.3,35.,-1.4));
#36338=CARTESIAN_POINT('',(-27.3,35.,5.));
#36339=CARTESIAN_POINT('Origin',(-24.,35.,-1.4));
#36340=CARTESIAN_POINT('Origin',(24.,35.,5.));
#36341=CARTESIAN_POINT('',(18.5,35.,-1.4));
#36342=CARTESIAN_POINT('Origin',(24.,35.,-1.4));
#36343=CARTESIAN_POINT('',(18.5,35.,5.));
#36344=CARTESIAN_POINT('',(18.5,35.,5.));
#36345=CARTESIAN_POINT('Origin',(24.,35.,5.));
#36346=CARTESIAN_POINT('Origin',(24.,35.,5.));
#36347=CARTESIAN_POINT('',(20.7,35.,-5.));
#36348=CARTESIAN_POINT('Origin',(24.,35.,-5.));
#36349=CARTESIAN_POINT('',(20.7,35.,-1.4));
#36350=CARTESIAN_POINT('',(20.7,35.,5.));
#36351=CARTESIAN_POINT('Origin',(24.,35.,-1.4));
#36352=CARTESIAN_POINT('Origin',(-1.20882209737476E-14,-2.49999999999972,
-5.));
#36353=CARTESIAN_POINT('',(-10.,-2.49999999999972,-5.));
#36354=CARTESIAN_POINT('Origin',(-1.20882209737476E-14,-2.49999999999972,
-5.));
#36355=CARTESIAN_POINT('',(-10.,-2.49999999999972,2.));
#36356=CARTESIAN_POINT('',(-10.,-2.49999999999972,-5.));
#36357=CARTESIAN_POINT('Origin',(-1.20882209737476E-14,-2.49999999999972,
2.));
#36358=CARTESIAN_POINT('Origin',(-1.20882209737476E-14,-2.49999999999972,
2.));
#36359=CARTESIAN_POINT('',(-25.,-2.49999999999972,2.));
#36360=CARTESIAN_POINT('Origin',(-1.20882209737476E-14,-2.49999999999972,
2.));
#36361=CARTESIAN_POINT('',(-25.,-2.49999999999972,5.));
#36362=CARTESIAN_POINT('',(-25.,-2.49999999999972,2.));
#36363=CARTESIAN_POINT('Origin',(-1.20882209737476E-14,-2.49999999999972,
5.));
#36364=CARTESIAN_POINT('Origin',(0.,0.,5.));
#36365=CARTESIAN_POINT('',(42.5,-42.5,5.));
#36366=CARTESIAN_POINT('',(42.5,42.5,5.));
#36367=CARTESIAN_POINT('',(42.5,-42.5,5.));
#36368=CARTESIAN_POINT('',(-42.5,42.5,5.));
#36369=CARTESIAN_POINT('',(-42.5,42.5,5.));
#36370=CARTESIAN_POINT('',(-42.5,-42.5,5.));
#36371=CARTESIAN_POINT('',(-42.5,-42.5,5.));
#36372=CARTESIAN_POINT('',(-42.5,-42.5,5.));
#36373=CARTESIAN_POINT('Origin',(42.5,-42.5,5.));
#36374=CARTESIAN_POINT('',(42.5,-42.5,-5.));
#36375=CARTESIAN_POINT('',(42.5,42.5,-5.));
#36376=CARTESIAN_POINT('',(42.5,-42.5,-5.));
#36377=CARTESIAN_POINT('',(42.5,42.5,5.));
#36378=CARTESIAN_POINT('',(42.5,-42.5,5.));
#36379=CARTESIAN_POINT('Origin',(-42.5,42.5,5.));
#36380=CARTESIAN_POINT('',(-42.5,42.5,-5.));
#36381=CARTESIAN_POINT('',(-42.5,42.5,-5.));
#36382=CARTESIAN_POINT('',(-42.5,42.5,5.));
#36383=CARTESIAN_POINT('Origin',(-42.5,-42.5,5.));
#36384=CARTESIAN_POINT('',(-42.5,-42.5,-5.));
#36385=CARTESIAN_POINT('',(-42.5,-42.5,-5.));
#36386=CARTESIAN_POINT('',(-42.5,-42.5,5.));
#36387=CARTESIAN_POINT('Origin',(-42.5,-42.5,5.));
#36388=CARTESIAN_POINT('',(-42.5,-42.5,-5.));
#36389=CARTESIAN_POINT('Origin',(0.,0.,-5.));
#36390=CARTESIAN_POINT('Origin',(-1.20882209737476E-14,-2.49999999999972,
2.));
#36391=CARTESIAN_POINT('Origin',(27.3,35.,-1.4));
#36392=CARTESIAN_POINT('Origin',(-20.7,35.,-1.4));
#36393=CARTESIAN_POINT('',(0.,0.,0.));
#36394=CARTESIAN_POINT('',(0.,0.,0.));
#36395=CARTESIAN_POINT('',(0.,0.,0.));
#36396=CARTESIAN_POINT('Origin',(7.4,0.,0.));
#36397=CARTESIAN_POINT('',(7.4,-12.,9.33005511289567E-11));
#36398=CARTESIAN_POINT('Origin',(7.4,-13.5,1.05000452776949E-10));
#36399=CARTESIAN_POINT('Origin',(7.4,-13.5,1.05000452776949E-10));
#36400=CARTESIAN_POINT('',(6.,-12.,9.33005511289567E-11));
#36401=CARTESIAN_POINT('',(7.4,-12.,9.33005511289567E-11));
#36402=CARTESIAN_POINT('Origin',(6.,-13.5,1.05000452776949E-10));
#36403=CARTESIAN_POINT('Origin',(-6.,0.,0.));
#36404=CARTESIAN_POINT('',(6.,-7.79422863409496,-4.49999999993936));
#36405=CARTESIAN_POINT('Origin',(6.,0.,0.));
#36406=CARTESIAN_POINT('',(-6.,-7.79422863409496,-4.49999999993936));
#36407=CARTESIAN_POINT('',(-6.,-7.79422863409496,-4.49999999993936));
#36408=CARTESIAN_POINT('Origin',(-6.,0.,0.));
#36409=CARTESIAN_POINT('Origin',(-7.4,0.,0.));
#36410=CARTESIAN_POINT('',(-7.4,-5.99999999991914,10.3923048454599));
#36411=CARTESIAN_POINT('Origin',(-7.4,-6.74999999990903,11.6913429511424));
#36412=CARTESIAN_POINT('Origin',(-6.,-6.74999999990903,11.6913429511424));
#36413=CARTESIAN_POINT('',(-6.,-5.99999999991914,10.3923048454599));
#36414=CARTESIAN_POINT('Origin',(-6.,-6.74999999990903,11.6913429511424));
#36415=CARTESIAN_POINT('',(-6.,-5.99999999991914,10.3923048454599));
#36416=CARTESIAN_POINT('Origin',(-5.599999999997,9.91330329119812,16.8993688492357));
#36417=CARTESIAN_POINT('',(-5.73644346284594,10.2877335024464,16.9337808604212));
#36418=CARTESIAN_POINT('',(-5.593361696257,10.1144356127388,17.245059060506));
#36419=CARTESIAN_POINT('Origin',(-5.599999999997,9.91330329119812,16.8993688492357));
#36420=CARTESIAN_POINT('',(-5.99999988457187,9.91329944048963,16.8993703246792));
#36421=CARTESIAN_POINT('Origin',(-5.59998163813197,9.91328781245746,16.899368578592));
#36422=CARTESIAN_POINT('Origin',(-5.6,9.91330329122126,16.8993688492756));
#36423=CARTESIAN_POINT('Ctrl Pts',(-5.71725976045777,6.24680066004962,7.76998179728242));
#36424=CARTESIAN_POINT('Ctrl Pts',(-5.71831534155782,6.59326365245468,8.0322873967129));
#36425=CARTESIAN_POINT('Ctrl Pts',(-5.72040693333068,7.31940961543903,8.6580789671924));
#36426=CARTESIAN_POINT('Ctrl Pts',(-5.72308360876896,8.29718047263615,9.7712913738905));
#36427=CARTESIAN_POINT('Ctrl Pts',(-5.72473138802017,9.14170425907276,11.09270696355));
#36428=CARTESIAN_POINT('Ctrl Pts',(-5.72548313711387,9.77722230302052,12.5261363218648));
#36429=CARTESIAN_POINT('Ctrl Pts',(-5.72532322728419,10.1890896765162,14.0392347180325));
#36430=CARTESIAN_POINT('Ctrl Pts',(-5.72405908827357,10.3627203405144,15.5563821125621));
#36431=CARTESIAN_POINT('Ctrl Pts',(-5.72276356923005,10.3310899357146,16.5600586046216));
#36432=CARTESIAN_POINT('Ctrl Pts',(-5.72204265313815,10.2826264054644,17.0373217472724));
#36433=CARTESIAN_POINT('Ctrl Pts',(-5.89609285952037,6.21373560947317,7.81372501070344));
#36434=CARTESIAN_POINT('Ctrl Pts',(-5.89699918874521,6.55804829801922,8.07502465641679));
#36435=CARTESIAN_POINT('Ctrl Pts',(-5.89878323011297,7.27965106221252,8.69820511837471));
#36436=CARTESIAN_POINT('Ctrl Pts',(-5.90106053656845,8.25103625935808,9.80606453249069));
#36437=CARTESIAN_POINT('Ctrl Pts',(-5.90245598645081,9.09015375604841,11.1204741768065));
#36438=CARTESIAN_POINT('Ctrl Pts',(-5.90309184480868,9.72171466792549,12.5458529340524));
#36439=CARTESIAN_POINT('Ctrl Pts',(-5.90295661080893,10.1313156291003,14.0503359021025));
#36440=CARTESIAN_POINT('Ctrl Pts',(-5.90188725304236,10.3045491222434,15.5587605290979));
#36441=CARTESIAN_POINT('Ctrl Pts',(-5.9007872150631,10.2737083057292,16.5568806432025));
#36442=CARTESIAN_POINT('Ctrl Pts',(-5.90017436173646,10.2258509289961,17.0315264876768));
#36443=CARTESIAN_POINT('Ctrl Pts',(-6.00525587186972,6.12207143860163,7.93499146478545));
#36444=CARTESIAN_POINT('Ctrl Pts',(-6.00574428560245,6.46106668108027,8.19265050892015));
#36445=CARTESIAN_POINT('Ctrl Pts',(-6.00669083800828,7.17158216493795,8.80708017905286));
#36446=CARTESIAN_POINT('Ctrl Pts',(-6.00789177595026,8.12777738756055,9.89880924904528));
#36447=CARTESIAN_POINT('Ctrl Pts',(-6.00861945068644,8.95391379465674,11.1937955392773));
#36448=CARTESIAN_POINT('Ctrl Pts',(-6.00895004139444,9.57571950519377,12.5976933827114));
#36449=CARTESIAN_POINT('Ctrl Pts',(-6.00887976204827,9.97922213092208,14.0795974958299));
#36450=CARTESIAN_POINT('Ctrl Pts',(-6.00832366160711,10.1501988766356,15.565149471362));
#36451=CARTESIAN_POINT('Ctrl Pts',(-6.00774632916138,10.1202032839983,16.5484119161439));
#36452=CARTESIAN_POINT('Ctrl Pts',(-6.00742377484676,10.0732750596108,17.0159525992194));
#36453=CARTESIAN_POINT('Ctrl Pts',(-5.99983168827394,6.00920933186455,8.08430153208114));
#36454=CARTESIAN_POINT('Ctrl Pts',(-5.99980403842103,6.34189025785474,8.33716995126331));
#36455=CARTESIAN_POINT('Ctrl Pts',(-5.99972489362897,7.03929972274239,8.94027820900691));
#36456=CARTESIAN_POINT('Ctrl Pts',(-5.99961167767651,7.97770097450654,10.0116798962465));
#36457=CARTESIAN_POINT('Ctrl Pts',(-5.99952863066508,8.78858003993403,11.2827506176984));
#36458=CARTESIAN_POINT('Ctrl Pts',(-5.99948914891546,9.39881401793521,12.660502777851));
#36459=CARTESIAN_POINT('Ctrl Pts',(-5.99949759662813,9.79487483211952,14.1150785938901));
#36460=CARTESIAN_POINT('Ctrl Pts',(-5.99956378228369,9.96265493708979,15.5729418984143));
#36461=CARTESIAN_POINT('Ctrl Pts',(-5.99962308473657,9.93321402551191,16.5381081995503));
#36462=CARTESIAN_POINT('Ctrl Pts',(-5.99965460768659,9.88715810520574,16.9969550810575));
#36463=CARTESIAN_POINT('',(-5.99998887464722,6.09546019355616,8.13557730976511));
#36464=CARTESIAN_POINT('Ctrl Pts',(-6.,6.09546019494773,8.13557730903106));
#36465=CARTESIAN_POINT('Ctrl Pts',(-6.,6.47284397463733,8.42688307326927));
#36466=CARTESIAN_POINT('Ctrl Pts',(-6.,6.8254268304029,8.74185019914476));
#36467=CARTESIAN_POINT('Ctrl Pts',(-6.,7.15537157648669,9.08219270087464));
#36468=CARTESIAN_POINT('Ctrl Pts',(-6.,7.48531632257071,9.42253520260476));
#36469=CARTESIAN_POINT('Ctrl Pts',(-6.,7.79262295897292,9.78825308018931));
#36470=CARTESIAN_POINT('Ctrl Pts',(-6.,8.07150656503307,10.1733979622484));
#36471=CARTESIAN_POINT('Ctrl Pts',(-6.,8.35039017109301,10.5585428443073));
#36472=CARTESIAN_POINT('Ctrl Pts',(-6.,8.60085074681092,10.9631147308407));
#36473=CARTESIAN_POINT('Ctrl Pts',(-6.,8.82146093284314,11.384374132216));
#36474=CARTESIAN_POINT('Ctrl Pts',(-6.,9.04207111887552,11.8056335335917));
#36475=CARTESIAN_POINT('Ctrl Pts',(-6.,9.23283091522216,12.2435804498092));
#36476=CARTESIAN_POINT('Ctrl Pts',(-6.,9.39100132241203,12.6919789552476));
#36477=CARTESIAN_POINT('Ctrl Pts',(-6.,9.5491717296018,13.1403774606856));
#36478=CARTESIAN_POINT('Ctrl Pts',(-6.,9.67475274763484,13.5992275553444));
#36479=CARTESIAN_POINT('Ctrl Pts',(-6.,9.76681039134521,14.065832740215));
#36480=CARTESIAN_POINT('Ctrl Pts',(-6.,9.85886803505566,14.5324379250859));
#36481=CARTESIAN_POINT('Ctrl Pts',(-6.,9.9174023044434,15.0067982001686));
#36482=CARTESIAN_POINT('Ctrl Pts',(-6.,9.94189523595854,15.4800412482395));
#36483=CARTESIAN_POINT('Ctrl Pts',(-6.,9.9663881501459,15.9532839615094));
#36484=CARTESIAN_POINT('Ctrl Pts',(-6.,9.95683977462647,16.4254094493483));
#36485=CARTESIAN_POINT('Ctrl Pts',(-6.,9.91329811959712,16.8993691888704));
#36486=CARTESIAN_POINT('',(-5.73278802440778,6.65588397732571,8.10254612026116));
#36487=CARTESIAN_POINT('Ctrl Pts',(-5.732788629548,6.65588508129815,8.10254480509131));
#36488=CARTESIAN_POINT('Ctrl Pts',(-5.73461480965429,7.28539041399694,8.63201072418106));
#36489=CARTESIAN_POINT('Ctrl Pts',(-5.73605973935097,7.85267746609106,9.23785132036226));
#36490=CARTESIAN_POINT('Ctrl Pts',(-5.73818934987832,8.82745380303726,10.5699124264369));
#36491=CARTESIAN_POINT('Ctrl Pts',(-5.73887403070899,9.23545520796598,11.295703388267));
#36492=CARTESIAN_POINT('Ctrl Pts',(-5.73948314350432,9.86673753303504,12.8258684760636));
#36493=CARTESIAN_POINT('Ctrl Pts',(-5.73940757546898,10.0903327813959,13.630101659641));
#36494=CARTESIAN_POINT('Ctrl Pts',(-5.73849619057271,10.3386823732913,15.2703413022844));
#36495=CARTESIAN_POINT('Ctrl Pts',(-5.7376603737792,10.3633358169702,16.1063565631604));
#36496=CARTESIAN_POINT('Ctrl Pts',(-5.73644356975675,10.2877321238833,16.9337807346159));
#36497=CARTESIAN_POINT('Ctrl Pts',(-5.99998887464722,6.09546019355616,8.13557730976511));
#36498=CARTESIAN_POINT('Ctrl Pts',(-5.99998547921825,6.11100675442636,8.12982511321127));
#36499=CARTESIAN_POINT('Ctrl Pts',(-5.99924702936141,6.12766659220297,8.12414369074788));
#36500=CARTESIAN_POINT('Ctrl Pts',(-5.99757111922383,6.14539399483326,8.1186593693785));
#36501=CARTESIAN_POINT('Ctrl Pts',(-5.99675849849762,6.1539897151385,8.1160001139005));
#36502=CARTESIAN_POINT('Ctrl Pts',(-5.99572521918872,6.16283590510732,8.11338762463451));
#36503=CARTESIAN_POINT('Ctrl Pts',(-5.99444641739924,6.17192415080112,8.11083892421808));
#36504=CARTESIAN_POINT('Ctrl Pts',(-5.99208335737192,6.18871805138383,8.10612925605431));
#36505=CARTESIAN_POINT('Ctrl Pts',(-5.98888154550485,6.20634057735348,8.10163637476274));
#36506=CARTESIAN_POINT('Ctrl Pts',(-5.98471929678868,6.2247122040356,8.09746910711326));
#36507=CARTESIAN_POINT('Ctrl Pts',(-5.98052075454122,6.24324402566355,8.09326550216895));
#36508=CARTESIAN_POINT('Ctrl Pts',(-5.97534531555817,6.26253869227697,8.08939271396174));
#36509=CARTESIAN_POINT('Ctrl Pts',(-5.96906451712721,6.28247648632352,8.0859850126498));
#36510=CARTESIAN_POINT('Ctrl Pts',(-5.96708036809606,6.28877497769776,8.08490849549504));
#36511=CARTESIAN_POINT('Ctrl Pts',(-5.96498585612993,6.29513733212402,8.08387858902862));
#36512=CARTESIAN_POINT('Ctrl Pts',(-5.96277675262812,6.30155884067799,8.08290011214028));
#36513=CARTESIAN_POINT('Ctrl Pts',(-5.96276819005269,6.30158373070752,8.08289631952388));
#36514=CARTESIAN_POINT('Ctrl Pts',(-5.96275962575552,6.30160862162516,8.08289252768054));
#36515=CARTESIAN_POINT('Ctrl Pts',(-5.96275105973646,6.30163351343065,8.08288873661048));
#36516=CARTESIAN_POINT('Ctrl Pts',(-5.95814393011898,6.31502126957647,8.08084975548942));
#36517=CARTESIAN_POINT('Ctrl Pts',(-5.95303858385639,6.32866657460956,8.07903412755458));
#36518=CARTESIAN_POINT('Ctrl Pts',(-5.94741092738046,6.34252571709171,8.07747974063197));
#36519=CARTESIAN_POINT('Ctrl Pts',(-5.9445970991425,6.34945528833279,8.07670254717067));
#36520=CARTESIAN_POINT('Ctrl Pts',(-5.94165265231472,6.35643830389429,8.07599068280171));
#36521=CARTESIAN_POINT('Ctrl Pts',(-5.93857476871761,6.36346828407662,8.07534936047085));
#36522=CARTESIAN_POINT('Ctrl Pts',(-5.93703582691906,6.36698327416778,8.07502869930542));
#36523=CARTESIAN_POINT('Ctrl Pts',(-5.93546352269515,6.37051000428783,8.07472567506216));
#36524=CARTESIAN_POINT('Ctrl Pts',(-5.93385750052388,6.37404762303365,8.07444096290844));
#36525=CARTESIAN_POINT('Ctrl Pts',(-5.93279072795071,6.37639742537131,8.07425184776279));
#36526=CARTESIAN_POINT('Ctrl Pts',(-5.93143880138408,6.37933801246212,8.07402708026044));
#36527=CARTESIAN_POINT('Ctrl Pts',(-5.93033826070994,6.38170074903567,8.07385531940472));
#36528=CARTESIAN_POINT('Ctrl Pts',(-5.92978194146144,6.38289510365233,8.07376849492615));
#36529=CARTESIAN_POINT('Ctrl Pts',(-5.9292907651449,6.38394211949884,8.07369460520274));
#36530=CARTESIAN_POINT('Ctrl Pts',(-5.92893791716396,6.38469226970929,8.07364245316878));
#36531=CARTESIAN_POINT('Ctrl Pts',(-5.92289625201354,6.39753677110612,8.07274947618402));
#36532=CARTESIAN_POINT('Ctrl Pts',(-5.91606342401493,6.4112632443089,8.07205752186807));
#36533=CARTESIAN_POINT('Ctrl Pts',(-5.90830129090174,6.4257653898265,8.07169387381413));
#36534=CARTESIAN_POINT('Ctrl Pts',(-5.90691979809071,6.42834645993764,8.07162915227884));
#36535=CARTESIAN_POINT('Ctrl Pts',(-5.90550885030405,6.43095199112076,8.07157490355159));
#36536=CARTESIAN_POINT('Ctrl Pts',(-5.90406764675699,6.43358123433491,8.07153194448689));
#36537=CARTESIAN_POINT('Ctrl Pts',(-5.89615881854175,6.44800961466963,8.07129619994988));
#36538=CARTESIAN_POINT('Ctrl Pts',(-5.88733820569935,6.46315548487182,8.07139869495401));
#36539=CARTESIAN_POINT('Ctrl Pts',(-5.87749024056837,6.47888151010761,8.0719744125043));
#36540=CARTESIAN_POINT('Ctrl Pts',(-5.86842267263249,6.49336133414135,8.07250450759804));
#36541=CARTESIAN_POINT('Ctrl Pts',(-5.85848396636633,6.50833316775113,8.07343572352348));
#36542=CARTESIAN_POINT('Ctrl Pts',(-5.84759199118979,6.52365222601063,8.07489256489634));
#36543=CARTESIAN_POINT('Ctrl Pts',(-5.8394675843952,6.53507882761346,8.07597923391242));
#36544=CARTESIAN_POINT('Ctrl Pts',(-5.83081293488375,6.54669795905989,8.07735867445034));
#36545=CARTESIAN_POINT('Ctrl Pts',(-5.8215980603499,6.55843293498189,8.07909108415474));
#36546=CARTESIAN_POINT('Ctrl Pts',(-5.80973305411518,6.57354280565538,8.08132172244159));
#36547=CARTESIAN_POINT('Ctrl Pts',(-5.79693781470784,6.58884594900205,8.08413740289622));
#36548=CARTESIAN_POINT('Ctrl Pts',(-5.78318272732981,6.60416096633479,8.08766122688759));
#36549=CARTESIAN_POINT('Ctrl Pts',(-5.77029728532473,6.61850771399437,8.09096226223757));
#36550=CARTESIAN_POINT('Ctrl Pts',(-5.75656940843594,6.6328650694371,8.09488457325179));
#36551=CARTESIAN_POINT('Ctrl Pts',(-5.74199708174794,6.64704591625766,8.09954446852334));
#36552=CARTESIAN_POINT('Ctrl Pts',(-5.73896289923755,6.64999858663946,8.10051473037897));
#36553=CARTESIAN_POINT('Ctrl Pts',(-5.73589219231249,6.65294345964691,8.10151702941778));
#36554=CARTESIAN_POINT('Ctrl Pts',(-5.7327850837695,6.65587860746633,8.10255251599254));
#36555=CARTESIAN_POINT('Ctrl Pts',(-6.05078733404053,6.21937608458398,8.31745500825333));
#36556=CARTESIAN_POINT('Ctrl Pts',(-6.05137679754613,6.24108609553353,8.30091555233655));
#36557=CARTESIAN_POINT('Ctrl Pts',(-6.04678918860765,6.29703472795143,8.2611303180236));
#36558=CARTESIAN_POINT('Ctrl Pts',(-6.01457192808413,6.39377016385395,8.20334817451699));
#36559=CARTESIAN_POINT('Ctrl Pts',(-5.94621587675347,6.50229665753326,8.15279007607915));
#36560=CARTESIAN_POINT('Ctrl Pts',(-5.84828986776081,6.60216364521869,8.12168124521672));
#36561=CARTESIAN_POINT('Ctrl Pts',(-5.76396986597587,6.65916518418619,8.11648706068094));
#36562=CARTESIAN_POINT('Ctrl Pts',(-5.71704487350945,6.68377535583102,8.11892530572803));
#36563=CARTESIAN_POINT('Ctrl Pts',(-5.71196257432753,6.68636226063928,8.11924826849545));
#36564=CARTESIAN_POINT('Ctrl Pts',(-5.91199258851529,6.05011231896361,8.08989903605235));
#36565=CARTESIAN_POINT('Ctrl Pts',(-5.91253370828238,6.06964670142851,8.07500751342556));
#36566=CARTESIAN_POINT('Ctrl Pts',(-5.90832434009387,6.12024088422482,8.03909466970484));
#36567=CARTESIAN_POINT('Ctrl Pts',(-5.87845614354468,6.20859036946667,7.98674208030229));
#36568=CARTESIAN_POINT('Ctrl Pts',(-5.81472572690307,6.30843918680031,7.94097921734113));
#36569=CARTESIAN_POINT('Ctrl Pts',(-5.72321219984663,6.40070331179899,7.9131149693122));
#36570=CARTESIAN_POINT('Ctrl Pts',(-5.64441899272344,6.45346152161701,7.90887821946799));
#36571=CARTESIAN_POINT('Ctrl Pts',(-5.60062844116605,6.47624545205135,7.91138088985345));
#36572=CARTESIAN_POINT('Ctrl Pts',(-5.59588636767232,6.47864049401491,7.91170558345452));
#36573=CARTESIAN_POINT('Ctrl Pts',(-6.02856994163684,5.87036955877751,7.85795328373691));
#36574=CARTESIAN_POINT('Ctrl Pts',(-6.02941873278482,5.90046478652428,7.83503197831369));
#36575=CARTESIAN_POINT('Ctrl Pts',(-6.02279786501192,5.97674408746066,7.78079086085649));
#36576=CARTESIAN_POINT('Ctrl Pts',(-5.97860852335649,6.10429897334357,7.70442875673926));
#36577=CARTESIAN_POINT('Ctrl Pts',(-5.88754256740064,6.24419084675625,7.63901853366117));
#36578=CARTESIAN_POINT('Ctrl Pts',(-5.75869070430417,6.37188881584455,7.59917623945032));
#36579=CARTESIAN_POINT('Ctrl Pts',(-5.64770213594862,6.4452055625109,7.59265250311272));
#36580=CARTESIAN_POINT('Ctrl Pts',(-5.58549485259654,6.47719013590213,7.59599015744902));
#36581=CARTESIAN_POINT('Ctrl Pts',(-5.57875178789665,6.48055677169745,7.59642913085163));
#36582=CARTESIAN_POINT('Ctrl Pts',(-6.32411122307629,5.79795599112006,7.77364115833111));
#36583=CARTESIAN_POINT('Ctrl Pts',(-6.32542204434578,5.84442666570434,7.73827529736239));
#36584=CARTESIAN_POINT('Ctrl Pts',(-6.31518050053343,5.9605959104862,7.65551810315682));
#36585=CARTESIAN_POINT('Ctrl Pts',(-6.2493862815084,6.14925123617853,7.54144392085583));
#36586=CARTESIAN_POINT('Ctrl Pts',(-6.1169400851386,6.35166156312029,7.44482117005616));
#36587=CARTESIAN_POINT('Ctrl Pts',(-5.93147165227156,6.53460575418067,7.38562894665993));
#36588=CARTESIAN_POINT('Ctrl Pts',(-5.77166730225767,6.63980826589821,7.37507275783575));
#36589=CARTESIAN_POINT('Ctrl Pts',(-5.68156295277533,6.68599000877552,7.37946868324932));
#36590=CARTESIAN_POINT('Ctrl Pts',(-5.67178918527753,6.69085488542317,7.3800595832833));
#36591=CARTESIAN_POINT('',(-5.72001857355568,6.64700964721696,7.39409311766332));
#36592=CARTESIAN_POINT('Origin',(-5.8987579215779,6.95916957771643,7.74135710698279));
#36593=CARTESIAN_POINT('',(-5.99999998746764,6.44014606542557,7.42970690919143));
#36594=CARTESIAN_POINT('Ctrl Pts',(-6.00000002220353,6.44014619802302,7.42970706216311));
#36595=CARTESIAN_POINT('Ctrl Pts',(-5.95906904703314,6.47976101005719,7.41728042107866));
#36596=CARTESIAN_POINT('Ctrl Pts',(-5.91529115572005,6.51678863678942,7.40807178321115));
#36597=CARTESIAN_POINT('Ctrl Pts',(-5.86865681612109,6.55130284293238,7.40207822663037));
#36598=CARTESIAN_POINT('Ctrl Pts',(-5.82202247652213,6.58581704907534,7.3960846700496));
#36599=CARTESIAN_POINT('Ctrl Pts',(-5.77253147336175,6.61781748381247,7.39330579278897));
#36600=CARTESIAN_POINT('Ctrl Pts',(-5.72001867760868,6.6470098289392,7.39409331980232));
#36601=CARTESIAN_POINT('Ctrl Pts',(-5.99998887464722,6.09546019355616,8.13557730976511));
#36602=CARTESIAN_POINT('Ctrl Pts',(-5.99998548962721,6.09908966555976,8.10734133180911));
#36603=CARTESIAN_POINT('Ctrl Pts',(-5.99998569058181,6.10340241851193,8.0796204247349));
#36604=CARTESIAN_POINT('Ctrl Pts',(-5.99998246305821,6.10842621161674,8.05243269583343));
#36605=CARTESIAN_POINT('Ctrl Pts',(-5.99998128988673,6.11025230849801,8.04255023731652));
#36606=CARTESIAN_POINT('Ctrl Pts',(-5.99997935490184,6.11217188802552,8.03273815173794));
#36607=CARTESIAN_POINT('Ctrl Pts',(-5.99997573731162,6.11418488655801,8.02299697961942));
#36608=CARTESIAN_POINT('Ctrl Pts',(-5.99996193796901,6.12186349433934,7.98583915817959));
#36609=CARTESIAN_POINT('Ctrl Pts',(-5.99992695587156,6.13090233978705,7.94971604561126));
#36610=CARTESIAN_POINT('Ctrl Pts',(-5.99991596216633,6.14126851094962,7.91458364660781));
#36611=CARTESIAN_POINT('Ctrl Pts',(-5.99990553965583,6.15109609186687,7.8812766050195));
#36612=CARTESIAN_POINT('Ctrl Pts',(-5.99990306372909,6.1621404443772,7.84887553209668));
#36613=CARTESIAN_POINT('Ctrl Pts',(-5.99990503429433,6.17439332140972,7.81739276335889));
#36614=CARTESIAN_POINT('Ctrl Pts',(-5.99990615565766,6.18136590304599,7.79947728321676));
#36615=CARTESIAN_POINT('Ctrl Pts',(-5.99990893829224,6.1887300454836,7.78185864041553));
#36616=CARTESIAN_POINT('Ctrl Pts',(-5.99991563402973,6.19649203440266,7.7645342226708));
#36617=CARTESIAN_POINT('Ctrl Pts',(-5.99991845242869,6.1997592445525,7.75724195337154));
#36618=CARTESIAN_POINT('Ctrl Pts',(-5.99992643742721,6.20320569045125,7.74975283151406));
#36619=CARTESIAN_POINT('Ctrl Pts',(-5.99993172356156,6.20668978085882,7.74241141820367));
#36620=CARTESIAN_POINT('Ctrl Pts',(-5.99993707718041,6.21021835029205,7.73497628203515));
#36621=CARTESIAN_POINT('Ctrl Pts',(-5.99993939007667,6.21378540141034,7.72769295558882));
#36622=CARTESIAN_POINT('Ctrl Pts',(-5.99994434414875,6.21719223499444,7.72090801999296));
#36623=CARTESIAN_POINT('Ctrl Pts',(-5.99994517942683,6.2177666419404,7.71976405036899));
#36624=CARTESIAN_POINT('Ctrl Pts',(-5.99994612554702,6.21833638344123,7.71863421773668));
#36625=CARTESIAN_POINT('Ctrl Pts',(-5.99994725311684,6.21890037837763,7.71752014509275));
#36626=CARTESIAN_POINT('Ctrl Pts',(-5.9999739635128,6.23226055161525,7.69112947638033));
#36627=CARTESIAN_POINT('Ctrl Pts',(-5.99995992531238,6.24654172946454,7.66574054511034));
#36628=CARTESIAN_POINT('Ctrl Pts',(-5.99993534254208,6.26167056867004,7.64131941866416));
#36629=CARTESIAN_POINT('Ctrl Pts',(-5.9999120470352,6.27600719443074,7.61817709123521));
#36630=CARTESIAN_POINT('Ctrl Pts',(-5.9998806732924,6.29110549459433,7.59590273476373));
#36631=CARTESIAN_POINT('Ctrl Pts',(-5.99986484539969,6.30694581008885,7.57447640629471));
#36632=CARTESIAN_POINT('Ctrl Pts',(-5.99984908651931,6.32271705907836,7.55314350030978));
#36633=CARTESIAN_POINT('Ctrl Pts',(-5.99985008116883,6.33922486146098,7.53265019329587));
#36634=CARTESIAN_POINT('Ctrl Pts',(-5.99987209092983,6.35648736495212,7.51299767308082));
#36635=CARTESIAN_POINT('Ctrl Pts',(-5.99989343825301,6.37323031099825,7.49393664373473));
#36636=CARTESIAN_POINT('Ctrl Pts',(-5.99993510456538,6.39068433272936,7.47566639388829));
#36637=CARTESIAN_POINT('Ctrl Pts',(-5.99996736242159,6.40888164182049,7.45821957055967));
#36638=CARTESIAN_POINT('Ctrl Pts',(-5.99998541956038,6.41906803901105,7.44845327647471));
#36639=CARTESIAN_POINT('Ctrl Pts',(-5.99999986746529,6.42948753754744,7.43894559930852));
#36640=CARTESIAN_POINT('Ctrl Pts',(-5.99999986894896,6.44014594987542,7.42970677588644));
#36641=CARTESIAN_POINT('Ctrl Pts',(6.05076594298383,10.3129892342082,1.22620019878532));
#36642=CARTESIAN_POINT('Ctrl Pts',(6.05141715339522,10.3095618497228,1.25273481980966));
#36643=CARTESIAN_POINT('Ctrl Pts',(6.04716023846436,10.3030216335477,1.32055479041099));
#36644=CARTESIAN_POINT('Ctrl Pts',(6.01566436669805,10.3011133365561,1.43300903845304));
#36645=CARTESIAN_POINT('Ctrl Pts',(5.94752234234302,10.3114150966028,1.55314313783514));
#36646=CARTESIAN_POINT('Ctrl Pts',(5.84909941351561,10.3344537772754,1.65630672975824));
#36647=CARTESIAN_POINT('Ctrl Pts',(5.76414056613767,10.358630474181,1.70872457384661));
#36648=CARTESIAN_POINT('Ctrl Pts',(5.71688012150772,10.3731536343596,1.72893354987749));
#36649=CARTESIAN_POINT('Ctrl Pts',(5.71193038493101,10.3746858130558,1.73095764713588));
#36650=CARTESIAN_POINT('Ctrl Pts',(5.91195398463708,10.0312610302219,1.19351178706232));
#36651=CARTESIAN_POINT('Ctrl Pts',(5.91255178532836,10.0281685311092,1.21738790649602));
#36652=CARTESIAN_POINT('Ctrl Pts',(5.90864761849278,10.0223078652808,1.27867029765757));
#36653=CARTESIAN_POINT('Ctrl Pts',(5.8794545808466,10.0209225268295,1.38114550802042));
#36654=CARTESIAN_POINT('Ctrl Pts',(5.81592995132105,10.0310514474921,1.4912833203987));
#36655=CARTESIAN_POINT('Ctrl Pts',(5.7239554292842,10.053099985886,1.58614623982501));
#36656=CARTESIAN_POINT('Ctrl Pts',(5.64456681575892,10.075974957363,1.6343728591383));
#36657=CARTESIAN_POINT('Ctrl Pts',(5.60046479938737,10.0896338081727,1.65295820241385));
#36658=CARTESIAN_POINT('Ctrl Pts',(5.59584656161539,10.0910739675031,1.65481961370909));
#36659=CARTESIAN_POINT('Ctrl Pts',(6.02852441748326,9.74057618693592,1.15323046382272));
#36660=CARTESIAN_POINT('Ctrl Pts',(6.02946196048018,9.735828951765,1.19002894035524));
#36661=CARTESIAN_POINT('Ctrl Pts',(6.02330619665441,9.72690801122379,1.28256626988032));
#36662=CARTESIAN_POINT('Ctrl Pts',(5.98006577432888,9.72424621979883,1.43102946984614));
#36663=CARTESIAN_POINT('Ctrl Pts',(5.88925233756573,9.73731875155346,1.58604362930984));
#36664=CARTESIAN_POINT('Ctrl Pts',(5.75974090924188,9.76671869076749,1.71798797258565));
#36665=CARTESIAN_POINT('Ctrl Pts',(5.64791671092265,9.79794966063946,1.78532744029789));
#36666=CARTESIAN_POINT('Ctrl Pts',(5.5852625769881,9.81697297564258,1.81150815891621));
#36667=CARTESIAN_POINT('Ctrl Pts',(5.57869530741879,9.81898275134499,1.81413330240522));
#36668=CARTESIAN_POINT('Ctrl Pts',(6.32406684675164,9.63147436024286,1.13176005092088));
#36669=CARTESIAN_POINT('Ctrl Pts',(6.32551458769723,9.62416742424068,1.18859131639995));
#36670=CARTESIAN_POINT('Ctrl Pts',(6.31597877248707,9.61045235182775,1.32968892101247));
#36671=CARTESIAN_POINT('Ctrl Pts',(6.25154861315667,9.60555139342322,1.54996264460781));
#36672=CARTESIAN_POINT('Ctrl Pts',(6.11942760311156,9.62275449059315,1.7753099581504));
#36673=CARTESIAN_POINT('Ctrl Pts',(5.93299887882128,9.66302863226776,1.96541145925877));
#36674=CARTESIAN_POINT('Ctrl Pts',(5.77199435470564,9.70679608296843,2.06263963985118));
#36675=CARTESIAN_POINT('Ctrl Pts',(5.68123821408197,9.73389630361412,2.10065607808985));
#36676=CARTESIAN_POINT('Ctrl Pts',(5.67171894552347,9.73676395577024,2.1044707560063));
#36677=CARTESIAN_POINT('',(5.73278523421135,10.3449523238712,1.71289271684915));
#36678=CARTESIAN_POINT('',(5.72001553852396,9.72697684558834,2.05943436519823));
#36679=CARTESIAN_POINT('Origin',(5.89875809739164,10.1838003793526,2.15614465708099));
#36680=CARTESIAN_POINT('',(5.999999988605,9.65438797224885,1.86247647806753));
#36681=CARTESIAN_POINT('Ctrl Pts',(6.00000005199597,9.65438817668948,1.86247651750723));
#36682=CARTESIAN_POINT('Ctrl Pts',(5.95914560526064,9.66341676699531,1.90292211689277));
#36683=CARTESIAN_POINT('Ctrl Pts',(5.91541907066705,9.67394092583593,1.93956812259589));
#36684=CARTESIAN_POINT('Ctrl Pts',(5.86878902309983,9.6860048617978,1.97246300793595));
#36685=CARTESIAN_POINT('Ctrl Pts',(5.8221589755326,9.69806879775966,2.005357893276));
#36686=CARTESIAN_POINT('Ctrl Pts',(5.7726251819321,9.7116719571993,2.0345015539125));
#36687=CARTESIAN_POINT('Ctrl Pts',(5.72001606109123,9.72697818110479,2.05943464798176));
#36688=CARTESIAN_POINT('',(5.99998738510661,10.0933419068162,1.21103477369025));
#36689=CARTESIAN_POINT('Ctrl Pts',(5.99998738510661,10.0933419068162,1.21103477369025));
#36690=CARTESIAN_POINT('Ctrl Pts',(5.99998486187685,10.0708534763626,1.22818435848599));
#36691=CARTESIAN_POINT('Ctrl Pts',(5.99998575125151,10.0491424232848,1.24566234602253));
#36692=CARTESIAN_POINT('Ctrl Pts',(5.99998220172071,10.0282383838849,1.26348392485136));
#36693=CARTESIAN_POINT('Ctrl Pts',(5.9999810788975,10.0216258083253,1.26912142554399));
#36694=CARTESIAN_POINT('Ctrl Pts',(5.9999792883417,10.0150937600636,1.27479302580716));
#36695=CARTESIAN_POINT('Ctrl Pts',(5.99997621692473,10.0086425621615,1.28049853326882));
#36696=CARTESIAN_POINT('Ctrl Pts',(5.99996211490628,9.97902271150216,1.30669464157516));
#36697=CARTESIAN_POINT('Ctrl Pts',(5.99992503046489,9.95111114927153,1.33360519795231));
#36698=CARTESIAN_POINT('Ctrl Pts',(5.99991423108135,9.92484903553856,1.36122131801052));
#36699=CARTESIAN_POINT('Ctrl Pts',(5.99990487784502,9.90210368572874,1.38513935893827));
#36700=CARTESIAN_POINT('Ctrl Pts',(5.99990278201543,9.88061743467843,1.4095991312432));
#36701=CARTESIAN_POINT('Ctrl Pts',(5.99990421744039,9.86039663880491,1.43458775228001));
#36702=CARTESIAN_POINT('Ctrl Pts',(5.9999051516139,9.84723695980441,1.45085032837081));
#36703=CARTESIAN_POINT('Ctrl Pts',(5.99990793441967,9.83461274768095,1.46733727486941));
#36704=CARTESIAN_POINT('Ctrl Pts',(5.99991541529783,9.82252505006016,1.48405677334895));
#36705=CARTESIAN_POINT('Ctrl Pts',(5.99991831505952,9.81783957843132,1.49053763829377));
#36706=CARTESIAN_POINT('Ctrl Pts',(5.99992637047857,9.8130737739939,1.49727174220381));
#36707=CARTESIAN_POINT('Ctrl Pts',(5.99993172018365,9.80845502960049,1.50396438277711));
#36708=CARTESIAN_POINT('Ctrl Pts',(5.99993713803762,9.80377744788307,1.51074227965135));
#36709=CARTESIAN_POINT('Ctrl Pts',(5.99993950798813,9.79925089617219,1.51747738340903));
#36710=CARTESIAN_POINT('Ctrl Pts',(5.99994451737579,9.79507593996524,1.52382456677347));
#36711=CARTESIAN_POINT('Ctrl Pts',(5.99994535116368,9.79438103908289,1.52488102415929));
#36712=CARTESIAN_POINT('Ctrl Pts',(5.99994629295769,9.79369579857702,1.52592665612043));
#36713=CARTESIAN_POINT('Ctrl Pts',(5.99994741064945,9.7930210497323,1.52695978247457));
#36714=CARTESIAN_POINT('Ctrl Pts',(5.99997420500895,9.7768453349225,1.55172686047367));
#36715=CARTESIAN_POINT('Ctrl Pts',(5.99996028565684,9.76199767903545,1.57679079684059));
#36716=CARTESIAN_POINT('Ctrl Pts',(5.99993572431047,9.74841211997671,1.60210482022966));
#36717=CARTESIAN_POINT('Ctrl Pts',(5.99991395264929,9.73636961284882,1.62454366914126));
#36718=CARTESIAN_POINT('Ctrl Pts',(5.99988491856912,9.72531845430559,1.64718009827664));
#36719=CARTESIAN_POINT('Ctrl Pts',(5.9998683047256,9.71523554983366,1.67000758547262));
#36720=CARTESIAN_POINT('Ctrl Pts',(5.99985059014724,9.70448461185646,1.69434748670864));
#36721=CARTESIAN_POINT('Ctrl Pts',(5.99984847396064,9.69483366624625,1.71890568866634));
#36722=CARTESIAN_POINT('Ctrl Pts',(5.99986814609526,9.68629032422623,1.74369683123673));
#36723=CARTESIAN_POINT('Ctrl Pts',(5.99988721410777,9.67800934426949,1.76772664933938));
#36724=CARTESIAN_POINT('Ctrl Pts',(5.99992732030898,9.67076938299242,1.79197637886837));
#36725=CARTESIAN_POINT('Ctrl Pts',(5.99996104571487,9.66461289211092,1.81645815869563));
#36726=CARTESIAN_POINT('Ctrl Pts',(5.99998205295574,9.6607780713449,1.83170763107814));
#36727=CARTESIAN_POINT('Ctrl Pts',(5.99999988350975,9.65736434128087,1.84704704982016));
#36728=CARTESIAN_POINT('Ctrl Pts',(5.99999988745995,9.6543877773096,1.86247644046082));
#36729=CARTESIAN_POINT('Ctrl Pts',(5.99998738510661,10.0933419068162,1.21103477369025));
#36730=CARTESIAN_POINT('Ctrl Pts',(5.99998441904465,10.0961480732035,1.22745270725951));
#36731=CARTESIAN_POINT('Ctrl Pts',(5.99923974683307,10.0995757628645,1.24479982112044));
#36732=CARTESIAN_POINT('Ctrl Pts',(5.99754903871016,10.1037122322766,1.26297222218984));
#36733=CARTESIAN_POINT('Ctrl Pts',(5.99682966762832,10.1054722382975,1.27070430772234));
#36734=CARTESIAN_POINT('Ctrl Pts',(5.99593880558416,10.1073606499676,1.27858524270412));
#36735=CARTESIAN_POINT('Ctrl Pts',(5.99485951760923,10.109384630221,1.28660438308776));
#36736=CARTESIAN_POINT('Ctrl Pts',(5.99246751490685,10.1138703340814,1.30437703127238));
#36737=CARTESIAN_POINT('Ctrl Pts',(5.98914967992163,10.1190220691058,1.32283170632383));
#36738=CARTESIAN_POINT('Ctrl Pts',(5.98476329112109,10.1249037655265,1.34182449996128));
#36739=CARTESIAN_POINT('Ctrl Pts',(5.98056287386319,10.130536093228,1.3600120482608));
#36740=CARTESIAN_POINT('Ctrl Pts',(5.97538295501154,10.1368376689458,1.37869350108863));
#36741=CARTESIAN_POINT('Ctrl Pts',(5.96909418209851,10.1438652718173,1.39769699124418));
#36742=CARTESIAN_POINT('Ctrl Pts',(5.96738486869547,10.1457754021314,1.40286221518796));
#36743=CARTESIAN_POINT('Ctrl Pts',(5.96559359347928,10.1477391785027,1.40805094260893));
#36744=CARTESIAN_POINT('Ctrl Pts',(5.96371764325191,10.1497577676557,1.41325904326785));
#36745=CARTESIAN_POINT('Ctrl Pts',(5.96344414271051,10.1500520639639,1.41401834824787));
#36746=CARTESIAN_POINT('Ctrl Pts',(5.96316884223256,10.1503475253814,1.41477806446667));
#36747=CARTESIAN_POINT('Ctrl Pts',(5.96289173637458,10.1506441544023,1.41553818059405));
#36748=CARTESIAN_POINT('Ctrl Pts',(5.95830642825136,10.1555525149422,1.42811592499401));
#36749=CARTESIAN_POINT('Ctrl Pts',(5.9532266748501,10.1607806414693,1.44080394687483));
#36750=CARTESIAN_POINT('Ctrl Pts',(5.94762863090485,10.1663393817787,1.45354595744594));
#36751=CARTESIAN_POINT('Ctrl Pts',(5.94482960893222,10.1691187519334,1.4599169627315));
#36752=CARTESIAN_POINT('Ctrl Pts',(5.94190097307532,10.1719807843508,1.46630144268669));
#36753=CARTESIAN_POINT('Ctrl Pts',(5.9388399270167,10.1749267438764,1.47269125767461));
#36754=CARTESIAN_POINT('Ctrl Pts',(5.93730940398739,10.1763997236392,1.47588616516857));
#36755=CARTESIAN_POINT('Ctrl Pts',(5.93574577516673,10.1778936858389,1.47908240474024));
#36756=CARTESIAN_POINT('Ctrl Pts',(5.93414868741022,10.1794087883726,1.48227891189157));
#36757=CARTESIAN_POINT('Ctrl Pts',(5.93308462549516,10.1804182275201,1.4844085891789));
#36758=CARTESIAN_POINT('Ctrl Pts',(5.93173682914368,10.1816910636254,1.4870663279203));
#36759=CARTESIAN_POINT('Ctrl Pts',(5.93064071602891,10.1827204106847,1.48919534164818));
#36760=CARTESIAN_POINT('Ctrl Pts',(5.93009163462014,10.1832360466403,1.49026183911203));
#36761=CARTESIAN_POINT('Ctrl Pts',(5.92960660183023,10.1836902190877,1.49119622911705));
#36762=CARTESIAN_POINT('Ctrl Pts',(5.92925668657071,10.1840176761403,1.49186814347237));
#36763=CARTESIAN_POINT('Ctrl Pts',(5.92324503182682,10.1896434917922,1.50341184444495));
#36764=CARTESIAN_POINT('Ctrl Pts',(5.91644346846693,10.1958846454291,1.51562382600558));
#36765=CARTESIAN_POINT('Ctrl Pts',(5.90871316153225,10.2027984780577,1.5283486336031));
#36766=CARTESIAN_POINT('Ctrl Pts',(5.90756562565091,10.2038248113049,1.53023758489891));
#36767=CARTESIAN_POINT('Ctrl Pts',(5.9063976103785,10.2048659743285,1.53213774426546));
#36768=CARTESIAN_POINT('Ctrl Pts',(5.90520864835011,10.2059221612598,1.53404850168093));
#36769=CARTESIAN_POINT('Ctrl Pts',(5.89737762539582,10.2128786694627,1.54663358415056));
#36770=CARTESIAN_POINT('Ctrl Pts',(5.88863728924836,10.2204871202784,1.55968229442971));
#36771=CARTESIAN_POINT('Ctrl Pts',(5.87887072452031,10.2287962590974,1.57300928454709));
#36772=CARTESIAN_POINT('Ctrl Pts',(5.86988433341336,10.2364416465257,1.58527168681525));
#36773=CARTESIAN_POINT('Ctrl Pts',(5.86002895799353,10.244680267378,1.5977698555925));
#36774=CARTESIAN_POINT('Ctrl Pts',(5.84922133220102,10.2535479575985,1.6103174241131));
#36775=CARTESIAN_POINT('Ctrl Pts',(5.84083255094556,10.260430978433,1.62005673315545));
#36776=CARTESIAN_POINT('Ctrl Pts',(5.83187017546044,10.2676929521663,1.62982514960955));
#36777=CARTESIAN_POINT('Ctrl Pts',(5.82229987253264,10.2753496142587,1.63951416959187));
#36778=CARTESIAN_POINT('Ctrl Pts',(5.81046704628954,10.2848163942369,1.65149377888759));
#36779=CARTESIAN_POINT('Ctrl Pts',(5.79770347959874,10.2948870147308,1.66335292667562));
#36780=CARTESIAN_POINT('Ctrl Pts',(5.78397884046087,10.3055776305931,1.67487325685049));
#36781=CARTESIAN_POINT('Ctrl Pts',(5.77112683449969,10.3155885210371,1.68566110712435));
#36782=CARTESIAN_POINT('Ctrl Pts',(5.75743196461773,10.3261430317943,1.6961520930176));
#36783=CARTESIAN_POINT('Ctrl Pts',(5.74289155719727,10.3372485293759,1.70612653191595));
#36784=CARTESIAN_POINT('Ctrl Pts',(5.73956598976375,10.3397884912919,1.70840780700054));
#36785=CARTESIAN_POINT('Ctrl Pts',(5.73619629460833,10.3423572505822,1.71066187634557));
#36786=CARTESIAN_POINT('Ctrl Pts',(5.73278262924252,10.3449548518058,1.71288576550861));
#36787=CARTESIAN_POINT('Ctrl Pts',(5.99928507670662,19.6591035996724,0.0581387347865464));
#36788=CARTESIAN_POINT('Ctrl Pts',(5.99928507670662,19.6322147711509,0.0775485171687107));
#36789=CARTESIAN_POINT('Ctrl Pts',(5.99928507670662,19.20584634456,0.382071892402484));
#36790=CARTESIAN_POINT('Ctrl Pts',(5.99928507670662,18.3334692836715,0.906208303978892));
#36791=CARTESIAN_POINT('Ctrl Pts',(5.99928507670662,16.9710191689203,1.46998611787121));
#36792=CARTESIAN_POINT('Ctrl Pts',(5.99928507670662,15.5398231880517,1.82605992904551));
#36793=CARTESIAN_POINT('Ctrl Pts',(5.99928507670662,14.0709530321673,1.9661847991881));
#36794=CARTESIAN_POINT('Ctrl Pts',(5.99928507670662,12.5966749488329,1.88736642753476));
#36795=CARTESIAN_POINT('Ctrl Pts',(5.99928507670662,11.233524511613,1.60731006115195));
#36796=CARTESIAN_POINT('Ctrl Pts',(5.99928507670662,10.3852007283801,1.30897054759059));
#36797=CARTESIAN_POINT('Ctrl Pts',(5.99928507670662,10.0105704034592,1.15061624350596));
#36798=CARTESIAN_POINT('Ctrl Pts',(6.0106308768628,19.7700374649892,0.211790355550257));
#36799=CARTESIAN_POINT('Ctrl Pts',(6.0106308768628,19.7426318213209,0.231572972437534));
#36800=CARTESIAN_POINT('Ctrl Pts',(6.0106308768628,19.3080752298907,0.541942236510507));
#36801=CARTESIAN_POINT('Ctrl Pts',(6.0106308768628,18.4191308604644,1.07604164186386));
#36802=CARTESIAN_POINT('Ctrl Pts',(6.0106308768628,17.030425424612,1.6506818513714));
#36803=CARTESIAN_POINT('Ctrl Pts',(6.0106308768628,15.5719791864793,2.01353171875612));
#36804=CARTESIAN_POINT('Ctrl Pts',(6.0106308768628,14.0748590038713,2.15635960358311));
#36805=CARTESIAN_POINT('Ctrl Pts',(6.0106308768628,12.5724428536086,2.07602891618263));
#36806=CARTESIAN_POINT('Ctrl Pts',(6.0106308768628,11.1830961575752,1.79059626133241));
#36807=CARTESIAN_POINT('Ctrl Pts',(6.0106308768628,10.3186145483331,1.48657404108104));
#36808=CARTESIAN_POINT('Ctrl Pts',(6.0106308768628,9.93678102105085,1.32517327201325));
#36809=CARTESIAN_POINT('Ctrl Pts',(5.90351527164667,19.8620727363884,0.339266023847184));
#36810=CARTESIAN_POINT('Ctrl Pts',(5.90351527164667,19.8342383217458,0.359357959490708));
#36811=CARTESIAN_POINT('Ctrl Pts',(5.90351527164667,19.3928884938992,0.674577212014692));
#36812=CARTESIAN_POINT('Ctrl Pts',(5.90351527164667,18.4901992077698,1.21694232444669));
#36813=CARTESIAN_POINT('Ctrl Pts',(5.90351527164667,17.0797112838011,1.80059442158608));
#36814=CARTESIAN_POINT('Ctrl Pts',(5.90351527164667,15.5986571178186,2.16906598231467));
#36815=CARTESIAN_POINT('Ctrl Pts',(5.90351527164667,14.0780995577289,2.31413639866398));
#36816=CARTESIAN_POINT('Ctrl Pts',(5.90351527164667,12.5523389164164,2.23255103227451));
#36817=CARTESIAN_POINT('Ctrl Pts',(5.90351527164667,11.1412587327508,1.94265798864203));
#36818=CARTESIAN_POINT('Ctrl Pts',(5.90351527164667,10.2633719302693,1.63392116252431));
#36819=CARTESIAN_POINT('Ctrl Pts',(5.90351527164667,9.87556233172656,1.46999292151928));
#36820=CARTESIAN_POINT('Ctrl Pts',(5.72195021115539,19.8960951816937,0.386389630772639));
#36821=CARTESIAN_POINT('Ctrl Pts',(5.72195021115539,19.8681022643737,0.406595911496531));
#36822=CARTESIAN_POINT('Ctrl Pts',(5.72195021115539,19.4242411980539,0.723608046948767));
#36823=CARTESIAN_POINT('Ctrl Pts',(5.72195021115539,18.5164708634373,1.2690287223504));
#36824=CARTESIAN_POINT('Ctrl Pts',(5.72195021115539,17.0979306623425,1.85601222112912));
#36825=CARTESIAN_POINT('Ctrl Pts',(5.72195021115539,15.608519081026,2.22656193897816));
#36826=CARTESIAN_POINT('Ctrl Pts',(5.72195021115539,14.0792974850575,2.37246134626695));
#36827=CARTESIAN_POINT('Ctrl Pts',(5.72195021115539,12.5449071449564,2.29041216587778));
#36828=CARTESIAN_POINT('Ctrl Pts',(5.72195021115539,11.1257927980475,1.99887026163753));
#36829=CARTESIAN_POINT('Ctrl Pts',(5.72195021115539,10.2429505317845,1.68839059912861));
#36830=CARTESIAN_POINT('Ctrl Pts',(5.72195021115539,9.85293177413904,1.52352803398365));
#36831=CARTESIAN_POINT('',(6.,19.5919343770476,0.135488060647564));
#36832=CARTESIAN_POINT('Ctrl Pts',(5.99999999999968,19.5919343770476,0.135488060647564));
#36833=CARTESIAN_POINT('Ctrl Pts',(5.99999999999968,19.4672328159283,0.223609584749507));
#36834=CARTESIAN_POINT('Ctrl Pts',(6.00000000003741,19.3409290210282,0.30857593928506));
#36835=CARTESIAN_POINT('Ctrl Pts',(5.99999999795218,19.2129689489122,0.390478679261728));
#36836=CARTESIAN_POINT('Ctrl Pts',(5.99999999586003,19.0845842822652,0.472653187258653));
#36837=CARTESIAN_POINT('Ctrl Pts',(5.99999999148612,18.9545319213896,0.551743936355476));
#36838=CARTESIAN_POINT('Ctrl Pts',(5.99999999087353,18.8227278694456,0.627799960860205));
#36839=CARTESIAN_POINT('Ctrl Pts',(5.99999999026193,18.6911386719661,0.70373200604732));
#36840=CARTESIAN_POINT('Ctrl Pts',(5.9999999969562,18.5578030768095,0.776639422345871));
#36841=CARTESIAN_POINT('Ctrl Pts',(5.99999999953308,18.4226144050266,0.846524611534863));
#36842=CARTESIAN_POINT('Ctrl Pts',(5.99999999982098,18.4075105210493,0.854332497915586));
#36843=CARTESIAN_POINT('Ctrl Pts',(5.99999999999968,18.3923834863004,0.862102610062003));
#36844=CARTESIAN_POINT('Ctrl Pts',(5.99999999999968,18.3772331375584,0.869834913416259));
#36845=CARTESIAN_POINT('Ctrl Pts',(5.99999999999968,18.3604577106659,0.878396610037155));
#36846=CARTESIAN_POINT('Ctrl Pts',(5.99999999977969,18.3436541191937,0.886912855498554));
#36847=CARTESIAN_POINT('Ctrl Pts',(5.99999999940206,18.3268228429537,0.895383270618578));
#36848=CARTESIAN_POINT('Ctrl Pts',(5.99999999572729,18.1630329068859,0.97781128921898));
#36849=CARTESIAN_POINT('Ctrl Pts',(5.99999998184252,17.9966189014925,1.0558956786728));
#36850=CARTESIAN_POINT('Ctrl Pts',(5.99999998033329,17.8280125915752,1.12938237918269));
#36851=CARTESIAN_POINT('Ctrl Pts',(5.99999997882266,17.6592495761256,1.20293737946452));
#36852=CARTESIAN_POINT('Ctrl Pts',(5.99999998730998,17.4882905775836,1.27188592951145));
#36853=CARTESIAN_POINT('Ctrl Pts',(5.99999999411981,17.3155939777246,1.33601879718248));
#36854=CARTESIAN_POINT('Ctrl Pts',(5.99999999739296,17.2325870839331,1.36684436143596));
#36855=CARTESIAN_POINT('Ctrl Pts',(5.99999999999968,17.1491790978227,1.39655807182192));
#36856=CARTESIAN_POINT('Ctrl Pts',(5.99999999999968,17.0654225833735,1.42514064586644));
#36857=CARTESIAN_POINT('Ctrl Pts',(5.99999999999968,17.0325894366093,1.43634521729203));
#36858=CARTESIAN_POINT('Ctrl Pts',(5.99999999960408,16.9997023256303,1.44737475909724));
#36859=CARTESIAN_POINT('Ctrl Pts',(5.99999999898859,16.9667622518599,1.45822900233135));
#36860=CARTESIAN_POINT('Ctrl Pts',(5.99999999507854,16.7575009061637,1.52718372178683));
#36861=CARTESIAN_POINT('Ctrl Pts',(5.99999998615649,16.5461037121443,1.5890678586064));
#36862=CARTESIAN_POINT('Ctrl Pts',(5.99999998771978,16.332871847101,1.64383796968629));
#36863=CARTESIAN_POINT('Ctrl Pts',(5.99999998928308,16.1196399820578,1.69860808076618));
#36864=CARTESIAN_POINT('Ctrl Pts',(5.99999999999968,15.9045728433345,1.74626433387793));
#36865=CARTESIAN_POINT('Ctrl Pts',(5.99999999999968,15.687957017083,1.7867113382546));
#36866=CARTESIAN_POINT('Ctrl Pts',(5.99999999999968,15.6384082465009,1.79596319845002));
#36867=CARTESIAN_POINT('Ctrl Pts',(5.99999999934663,15.5887787586434,1.80484044751495));
#36868=CARTESIAN_POINT('Ctrl Pts',(5.99999999845568,15.5390764076834,1.81334072030503));
#36869=CARTESIAN_POINT('Ctrl Pts',(5.99999999449756,15.3182715860499,1.85110354602646));
#36870=CARTESIAN_POINT('Ctrl Pts',(5.99999998895126,15.0960278363158,1.88142224228069));
#36871=CARTESIAN_POINT('Ctrl Pts',(5.99999999115147,14.8730346667746,1.90421141085561));
#36872=CARTESIAN_POINT('Ctrl Pts',(5.99999999312714,14.6727988930678,1.92467484841795));
#36873=CARTESIAN_POINT('Ctrl Pts',(5.99999999999968,14.4719593375783,1.93906781008501));
#36874=CARTESIAN_POINT('Ctrl Pts',(5.99999999999968,14.2710197375948,1.94736399718564));
#36875=CARTESIAN_POINT('Ctrl Pts',(5.99999999999968,14.2042157464008,1.95012213152083));
#36876=CARTESIAN_POINT('Ctrl Pts',(5.99999999913621,14.1374011154746,1.95220403825653));
#36877=CARTESIAN_POINT('Ctrl Pts',(5.99999999780769,14.0705840962199,1.95360927362166));
#36878=CARTESIAN_POINT('Ctrl Pts',(5.99999999336877,13.8473330129415,1.95830448931711));
#36879=CARTESIAN_POINT('Ctrl Pts',(5.99999998477708,13.6240549671328,1.95544941068481));
#36880=CARTESIAN_POINT('Ctrl Pts',(5.99999998688347,13.4010803985336,1.94504158174669));
#36881=CARTESIAN_POINT('Ctrl Pts',(5.99999998863002,13.2161971643747,1.93641174971364));
#36882=CARTESIAN_POINT('Ctrl Pts',(5.99999999999968,13.0315224106363,1.9225883059491));
#36883=CARTESIAN_POINT('Ctrl Pts',(5.99999999999968,12.847248931914,1.90354302871283));
#36884=CARTESIAN_POINT('Ctrl Pts',(5.99999999999968,12.7639691565099,1.89493578679314));
#36885=CARTESIAN_POINT('Ctrl Pts',(5.99999999683349,12.6807681678412,1.88527287357867));
#36886=CARTESIAN_POINT('Ctrl Pts',(5.9999999931907,12.5976921209349,1.87455549616479));
#36887=CARTESIAN_POINT('Ctrl Pts',(5.99999998466661,12.4032953145046,1.84947698051374));
#36888=CARTESIAN_POINT('Ctrl Pts',(5.99999997595973,12.2095833836002,1.81862087709688));
#36889=CARTESIAN_POINT('Ctrl Pts',(5.99999997954448,12.0171092535684,1.78211738648701));
#36890=CARTESIAN_POINT('Ctrl Pts',(5.99999998312923,11.8246351235367,1.74561389587715));
#36891=CARTESIAN_POINT('Ctrl Pts',(5.99999999999968,11.6333993074508,1.7034631726462));
#36892=CARTESIAN_POINT('Ctrl Pts',(5.99999999999968,11.4439401120787,1.65585043723543));
#36893=CARTESIAN_POINT('Ctrl Pts',(5.99999999999968,11.3471384627997,1.63152334503285));
#36894=CARTESIAN_POINT('Ctrl Pts',(5.99999999545162,11.2508119173546,1.6057505968365));
#36895=CARTESIAN_POINT('Ctrl Pts',(5.99999999307287,11.1549261368173,1.57853425346852));
#36896=CARTESIAN_POINT('Ctrl Pts',(5.99999998940933,11.0072519921261,1.53661823415922));
#36897=CARTESIAN_POINT('Ctrl Pts',(5.99999999031157,10.8606225700356,1.49128052602001));
#36898=CARTESIAN_POINT('Ctrl Pts',(5.99999999276237,10.7149492997484,1.44250629149568));
#36899=CARTESIAN_POINT('Ctrl Pts',(5.99999999520022,10.5700458283645,1.39398980056541));
#36900=CARTESIAN_POINT('Ctrl Pts',(5.99999999786777,10.4260879908288,1.34207286643751));
#36901=CARTESIAN_POINT('Ctrl Pts',(5.99999999875688,10.2830048093639,1.2866921338031));
#36902=CARTESIAN_POINT('Ctrl Pts',(5.99999999915078,10.2196135091128,1.26215635947515));
#36903=CARTESIAN_POINT('Ctrl Pts',(5.9999999993187,10.1563941419572,1.2369400707568));
#36904=CARTESIAN_POINT('Ctrl Pts',(5.99999999931442,10.0933419069091,1.21103477539414));
#36905=CARTESIAN_POINT('',(5.73644276520376,19.8089520716694,0.442549441855652));
#36906=CARTESIAN_POINT('Origin',(5.6,19.5919343769637,0.135488060672991));
#36907=CARTESIAN_POINT('Ctrl Pts',(5.73644276397656,19.8089520717766,0.442549442640921));
#36908=CARTESIAN_POINT('Ctrl Pts',(5.7370879225674,19.446718951205,0.69823623580988));
#36909=CARTESIAN_POINT('Ctrl Pts',(5.73762563118613,19.0680988842184,0.930502845521264));
#36910=CARTESIAN_POINT('Ctrl Pts',(5.73805595552339,18.676590268373,1.13733219036651));
#36911=CARTESIAN_POINT('Ctrl Pts',(5.73812189681018,18.61659695709,1.1690259431105));
#36912=CARTESIAN_POINT('Ctrl Pts',(5.73818531654776,18.556300916891,1.20012244044563));
#36913=CARTESIAN_POINT('Ctrl Pts',(5.73824621494312,18.4957146397251,1.23061447416638));
#36914=CARTESIAN_POINT('Ctrl Pts',(5.73865147315783,18.092533465989,1.43352864087569));
#36915=CARTESIAN_POINT('Ctrl Pts',(5.73894507726634,17.6765033902989,1.6096732180909));
#36916=CARTESIAN_POINT('Ctrl Pts',(5.7391270730799,17.2512590699236,1.75775966272543));
#36917=CARTESIAN_POINT('Ctrl Pts',(5.73915087282255,17.1956495194054,1.77712504923241));
#36918=CARTESIAN_POINT('Ctrl Pts',(5.73917276390775,17.1398823261237,1.79601063417806));
#36919=CARTESIAN_POINT('Ctrl Pts',(5.73919274639726,17.0839655556887,1.81441355455165));
#36920=CARTESIAN_POINT('Ctrl Pts',(5.73934700323792,16.652310413593,1.9564767521763));
#36921=CARTESIAN_POINT('Ctrl Pts',(5.73938752575625,16.2117458758467,2.06977630384664));
#36922=CARTESIAN_POINT('Ctrl Pts',(5.73931432087029,15.7661154481004,2.15354915603658));
#36923=CARTESIAN_POINT('Ctrl Pts',(5.73930537008875,15.7116280931828,2.16379208570551));
#36924=CARTESIAN_POINT('Ctrl Pts',(5.73929471903249,15.6570649397863,2.17359359951341));
#36925=CARTESIAN_POINT('Ctrl Pts',(5.73928236767428,15.6024329608079,2.1829523100585));
#36926=CARTESIAN_POINT('Ctrl Pts',(5.73918135759826,15.1556496796064,2.25948835146391));
#36927=CARTESIAN_POINT('Ctrl Pts',(5.73896663327029,14.7042676165308,2.30640958123039));
#36928=CARTESIAN_POINT('Ctrl Pts',(5.73863815933754,14.2522694751224,2.32359660893901));
#36929=CARTESIAN_POINT('Ctrl Pts',(5.73859603617049,14.1943056876852,2.32580065610097));
#36930=CARTESIAN_POINT('Ctrl Pts',(5.73855204231838,14.136331698548,2.32751571530993));
#36931=CARTESIAN_POINT('Ctrl Pts',(5.73850617766838,14.0783558454309,2.32874153312007));
#36932=CARTESIAN_POINT('Ctrl Pts',(5.73815298353712,13.6318958576921,2.33818130114516));
#36933=CARTESIAN_POINT('Ctrl Pts',(5.73768884856023,13.185329276007,2.31860847900135));
#36934=CARTESIAN_POINT('Ctrl Pts',(5.73711370893554,12.7423972566153,2.27028161135825));
#36935=CARTESIAN_POINT('Ctrl Pts',(5.73703020600255,12.6780891805479,2.26326516697304));
#36936=CARTESIAN_POINT('Ctrl Pts',(5.73694436300473,12.6138576339778,2.2556425960222));
#36937=CARTESIAN_POINT('Ctrl Pts',(5.73685617975576,12.5497139832806,2.24741467936474));
#36938=CARTESIAN_POINT('Ctrl Pts',(5.73622837211831,12.0930527208357,2.18883724001976));
#36939=CARTESIAN_POINT('Ctrl Pts',(5.73548194777951,11.6408504952097,2.09957923971377));
#36940=CARTESIAN_POINT('Ctrl Pts',(5.73461684134438,11.1969963232995,1.98082349864726));
#36941=CARTESIAN_POINT('Ctrl Pts',(5.73452245641432,11.1485709004022,1.96786699773642));
#36942=CARTESIAN_POINT('Ctrl Pts',(5.73442665879326,11.1002447987416,1.95455935976749));
#36943=CARTESIAN_POINT('Ctrl Pts',(5.73432944840997,11.0520230339019,1.94090210805598));
#36944=CARTESIAN_POINT('Ctrl Pts',(5.73384873497255,10.813562392646,1.87336586147213));
#36945=CARTESIAN_POINT('Ctrl Pts',(5.73333347377677,10.5776535681786,1.79728037334161));
#36946=CARTESIAN_POINT('Ctrl Pts',(5.73278365815296,10.34495385425,1.71288850793682));
#36947=CARTESIAN_POINT('Ctrl Pts',(5.99999999997507,19.5919300856952,-0.135488304642611));
#36948=CARTESIAN_POINT('Ctrl Pts',(5.99999999997507,19.5922326969838,-0.0451632714418701));
#36949=CARTESIAN_POINT('Ctrl Pts',(5.99999999997507,19.592232706457,0.045163275375177));
#36950=CARTESIAN_POINT('Ctrl Pts',(5.99999999997507,19.591929935039,0.135488872436178));
#36951=CARTESIAN_POINT('Ctrl Pts',(6.00000263486111,19.8293406274304,-0.136284098535555));
#36952=CARTESIAN_POINT('Ctrl Pts',(6.00000263486111,19.8296450131565,-0.0454285037137862));
#36953=CARTESIAN_POINT('Ctrl Pts',(6.00000263486111,19.8296450228453,0.0454285076464987));
#36954=CARTESIAN_POINT('Ctrl Pts',(6.00000263486111,19.8293404729502,0.136284669412338));
#36955=CARTESIAN_POINT('Ctrl Pts',(5.83074066841606,19.9958175555672,-0.136842124818485));
#36956=CARTESIAN_POINT('Ctrl Pts',(5.83074066841606,19.9961231855639,-0.0456144897847192));
#36957=CARTESIAN_POINT('Ctrl Pts',(5.83074066841606,19.9961231954044,0.0456144937168433));
#36958=CARTESIAN_POINT('Ctrl Pts',(5.83074066841606,19.9958173984079,0.136842697860198));
#36959=CARTESIAN_POINT('Ctrl Pts',(5.5933611004422,19.9918771871015,-0.136828916807151));
#36960=CARTESIAN_POINT('Ctrl Pts',(5.5933611004422,19.9921827876475,-0.0456100876498413));
#36961=CARTESIAN_POINT('Ctrl Pts',(5.5933611004422,19.9921827974873,0.045610091584508));
#36962=CARTESIAN_POINT('Ctrl Pts',(5.5933611004422,19.9918770300063,0.136829489796775));
#36963=CARTESIAN_POINT('',(5.99999999995612,19.5919320087503,-0.135481052873273));
#36964=CARTESIAN_POINT('',(5.59336167795915,19.9918770519504,-0.136828613280939));
#36965=CARTESIAN_POINT('Origin',(5.6,19.5919343769583,-0.135488060981343));
#36966=CARTESIAN_POINT('',(5.59336169562657,19.9918770422848,0.136828655448858));
#36967=CARTESIAN_POINT('Origin',(5.59336169594597,15.0903027128352,0.0604604316820303));
#36968=CARTESIAN_POINT('Origin',(5.6,19.5919343771351,0.13548806067611));
#36969=CARTESIAN_POINT('Ctrl Pts',(5.99999999999164,19.5919320204865,-0.135477553132434));
#36970=CARTESIAN_POINT('Ctrl Pts',(5.99999999999169,19.592033064822,-0.105317242394998));
#36971=CARTESIAN_POINT('Ctrl Pts',(5.9999999999997,19.5921021554901,-0.0751629212119529));
#36972=CARTESIAN_POINT('Ctrl Pts',(5.9999999999997,19.5921363906261,-0.0450478988915754));
#36973=CARTESIAN_POINT('Ctrl Pts',(5.9999999999997,19.5921706257621,-0.014932876571189));
#36974=CARTESIAN_POINT('Ctrl Pts',(5.9999999999997,19.5921700053662,0.0151428468865298));
#36975=CARTESIAN_POINT('Ctrl Pts',(5.9999999999997,19.5921361540918,0.0452268832839701));
#36976=CARTESIAN_POINT('Ctrl Pts',(5.9999999999997,19.5921023028175,0.0753109196814013));
#36977=CARTESIAN_POINT('Ctrl Pts',(5.9999999999997,19.5920352206648,0.105403269018554));
#36978=CARTESIAN_POINT('Ctrl Pts',(5.9999999999997,19.5919343770476,0.135488060647564));
#36979=CARTESIAN_POINT('Origin',(5.6,19.5919343769637,0.135488060672991));
#36980=CARTESIAN_POINT('Origin',(5.600000004204,19.5919343763224,0.135488059063745));
#36981=CARTESIAN_POINT('Ctrl Pts',(-5.69266556774165,19.9935543480601,0.076560747550209));
#36982=CARTESIAN_POINT('Ctrl Pts',(-5.6579015041137,19.9929008980439,0.0929956066630459));
#36983=CARTESIAN_POINT('Ctrl Pts',(-5.54372918028186,19.9908051431839,0.146474485765011));
#36984=CARTESIAN_POINT('Ctrl Pts',(-5.34117686668071,19.9873503305864,0.238480887060544));
#36985=CARTESIAN_POINT('Ctrl Pts',(-5.07577939190903,19.9832027490848,0.353603093965685));
#36986=CARTESIAN_POINT('Ctrl Pts',(-4.78282515660807,19.9789919207889,0.474026380935749));
#36987=CARTESIAN_POINT('Ctrl Pts',(-4.45930905769162,19.9747249819138,0.598869507096236));
#36988=CARTESIAN_POINT('Ctrl Pts',(-4.10061553943856,19.9704191073005,0.727257554679413));
#36989=CARTESIAN_POINT('Ctrl Pts',(-3.70134298961707,19.9661195200363,0.857723092138966));
#36990=CARTESIAN_POINT('Ctrl Pts',(-3.25666212542464,19.9619190254675,0.987529865804192));
#36991=CARTESIAN_POINT('Ctrl Pts',(-2.76257283838323,19.9579585252344,1.11255112813169));
#36992=CARTESIAN_POINT('Ctrl Pts',(-2.21448293057545,19.9544123316413,1.22757275325379));
#36993=CARTESIAN_POINT('Ctrl Pts',(-1.60537183762896,19.9514853648295,1.3262010465794));
#36994=CARTESIAN_POINT('Ctrl Pts',(-0.938804294807327,19.9494592496166,
1.39847259929471));
#36995=CARTESIAN_POINT('Ctrl Pts',(-0.236508776779611,19.9485851832705,
1.43363032242854));
#36996=CARTESIAN_POINT('Ctrl Pts',(0.464364601123389,19.948749328727,1.4264261030562));
#36997=CARTESIAN_POINT('Ctrl Pts',(1.12896559565999,19.9499401821903,1.38089160685135));
#36998=CARTESIAN_POINT('Ctrl Pts',(1.73422006980435,19.9520479706928,1.30699167215705));
#36999=CARTESIAN_POINT('Ctrl Pts',(2.27384587626356,19.9547877813634,1.21535231751198));
#37000=CARTESIAN_POINT('Ctrl Pts',(2.75210517028745,19.9579163355911,1.11403613854411));
#37001=CARTESIAN_POINT('Ctrl Pts',(3.17956446864321,19.9612849529054,1.00748451984042));
#37002=CARTESIAN_POINT('Ctrl Pts',(3.56234892004249,19.9647715292712,0.8992365099518));
#37003=CARTESIAN_POINT('Ctrl Pts',(3.90388903433588,19.9682667685621,0.792414560653075));
#37004=CARTESIAN_POINT('Ctrl Pts',(4.20698277151624,19.9716805654084,0.689557632968514));
#37005=CARTESIAN_POINT('Ctrl Pts',(4.47552350917186,19.9749594106943,0.592122104802372));
#37006=CARTESIAN_POINT('Ctrl Pts',(4.7143736486654,19.9780870462951,0.500500697884532));
#37007=CARTESIAN_POINT('Ctrl Pts',(4.92834373472852,19.9810702092344,0.414472289313536));
#37008=CARTESIAN_POINT('Ctrl Pts',(5.12117579191345,19.9839201644114,0.333751104062619));
#37009=CARTESIAN_POINT('Ctrl Pts',(5.29544459285731,19.9866447487504,0.258203140894221));
#37010=CARTESIAN_POINT('Ctrl Pts',(5.45302136069377,19.989249786509,0.187774421799672));
#37011=CARTESIAN_POINT('Ctrl Pts',(5.58355472894304,19.9915339342793,0.127841695660172));
#37012=CARTESIAN_POINT('Ctrl Pts',(5.66171727448302,19.9929727783557,0.0911904475355778));
#37013=CARTESIAN_POINT('Ctrl Pts',(5.69263920831736,19.9935543971865,0.0765659156944554));
#37014=CARTESIAN_POINT('Ctrl Pts',(-5.75649916782382,19.9991143710642,0.213746605759207));
#37015=CARTESIAN_POINT('Ctrl Pts',(-5.72140302733699,19.9983747379508,0.230339439268123));
#37016=CARTESIAN_POINT('Ctrl Pts',(-5.60614021201479,19.9959920716916,0.284332231538033));
#37017=CARTESIAN_POINT('Ctrl Pts',(-5.40164894966011,19.9920036394875,0.377223723225483));
#37018=CARTESIAN_POINT('Ctrl Pts',(-5.13368112668697,19.9871027056259,0.493463372834317));
#37019=CARTESIAN_POINT('Ctrl Pts',(-4.83783506997635,19.982026814529,0.615073150075648));
#37020=CARTESIAN_POINT('Ctrl Pts',(-4.51104954848351,19.976794518307,0.74116897376691));
#37021=CARTESIAN_POINT('Ctrl Pts',(-4.14863414602773,19.9714329010045,0.870871691441195));
#37022=CARTESIAN_POINT('Ctrl Pts',(-3.74509982337592,19.965998699662,1.00270211695211));
#37023=CARTESIAN_POINT('Ctrl Pts',(-3.29553136101948,19.9606049310289,1.13389675931631));
#37024=CARTESIAN_POINT('Ctrl Pts',(-2.79585032994363,19.9554249629654,1.26028299192613));
#37025=CARTESIAN_POINT('Ctrl Pts',(-2.24138300365344,19.9506788186159,1.37658388105494));
#37026=CARTESIAN_POINT('Ctrl Pts',(-1.62500802081888,19.9466357126787,1.47632451499044));
#37027=CARTESIAN_POINT('Ctrl Pts',(-0.950336100057744,19.9437046353406,
1.54941651962382));
#37028=CARTESIAN_POINT('Ctrl Pts',(-0.239411452580767,19.9423138347391,
1.58496955781237));
#37029=CARTESIAN_POINT('Ctrl Pts',(0.470068367955475,19.9425938101752,1.57768516782441));
#37030=CARTESIAN_POINT('Ctrl Pts',(1.14282032186782,19.9444142574433,1.53163591167869));
#37031=CARTESIAN_POINT('Ctrl Pts',(1.75540154182604,19.9474213041126,1.45689782413783));
#37032=CARTESIAN_POINT('Ctrl Pts',(2.30143868160016,19.9511828297409,1.3642271613645));
#37033=CARTESIAN_POINT('Ctrl Pts',(2.78525552181212,19.9553643975143,1.26178540691853));
#37034=CARTESIAN_POINT('Ctrl Pts',(3.21756459443667,19.9597777818374,1.1540687684985));
#37035=CARTESIAN_POINT('Ctrl Pts',(3.60458630024707,19.9642729470882,1.04465768021273));
#37036=CARTESIAN_POINT('Ctrl Pts',(3.94981603924592,19.9687180881684,0.936708354815534));
#37037=CARTESIAN_POINT('Ctrl Pts',(4.2561086909295,19.973006668013,0.832784704953047));
#37038=CARTESIAN_POINT('Ctrl Pts',(4.52742310268015,19.9770781627105,0.734355145957688));
#37039=CARTESIAN_POINT('Ctrl Pts',(4.76869242285065,19.9809173370862,0.641812973636067));
#37040=CARTESIAN_POINT('Ctrl Pts',(4.98479244425756,19.9845356429339,0.554931532203396));
#37041=CARTESIAN_POINT('Ctrl Pts',(5.17951571609395,19.9879485183431,0.473419145840954));
#37042=CARTESIAN_POINT('Ctrl Pts',(5.35547336786553,19.9911666293176,0.397137560135068));
#37043=CARTESIAN_POINT('Ctrl Pts',(5.5145642915736,19.9941992385701,0.326029401375756));
#37044=CARTESIAN_POINT('Ctrl Pts',(5.64634618113553,19.9968207967888,0.265520382202669));
#37045=CARTESIAN_POINT('Ctrl Pts',(5.7252551879899,19.9984564343695,0.228516946253832));
#37046=CARTESIAN_POINT('Ctrl Pts',(5.75647210573555,19.9991166589352,0.213751969958807));
#37047=CARTESIAN_POINT('Ctrl Pts',(-5.8136196818812,19.9261275467547,0.33332821073875));
#37048=CARTESIAN_POINT('Ctrl Pts',(-5.77819705107185,19.9253120907747,0.350030686003675));
#37049=CARTESIAN_POINT('Ctrl Pts',(-5.66186629696485,19.9226772399395,0.404374549031671));
#37050=CARTESIAN_POINT('Ctrl Pts',(-5.45549726798606,19.9182211259577,0.497839527211375));
#37051=CARTESIAN_POINT('Ctrl Pts',(-5.18506580575754,19.9126623370125,0.614749759844558));
#37052=CARTESIAN_POINT('Ctrl Pts',(-4.88647423531625,19.9068337910618,0.737027952359146));
#37053=CARTESIAN_POINT('Ctrl Pts',(-4.55661570515206,19.9007648007416,0.863793230857175));
#37054=CARTESIAN_POINT('Ctrl Pts',(-4.19074002651519,19.8944919190027,0.994166830412173));
#37055=CARTESIAN_POINT('Ctrl Pts',(-3.78329010948032,19.8880827064613,1.1266635068718));
#37056=CARTESIAN_POINT('Ctrl Pts',(-3.32928741344157,19.8816683464093,1.25850416200931));
#37057=CARTESIAN_POINT('Ctrl Pts',(-2.82459972123038,19.8754505103237,1.38549071493382));
#37058=CARTESIAN_POINT('Ctrl Pts',(-2.26449815900478,19.8696881919514,1.50231378248865));
#37059=CARTESIAN_POINT('Ctrl Pts',(-1.64179011342992,19.8647044795955,1.60246108002828));
#37060=CARTESIAN_POINT('Ctrl Pts',(-0.960140287927844,19.8610141389188,
1.67580351036708));
#37061=CARTESIAN_POINT('Ctrl Pts',(-0.241865765896076,19.8591912733021,
1.71143169382191));
#37062=CARTESIAN_POINT('Ctrl Pts',(0.474899624177775,19.8595680072199,1.7041381423012));
#37063=CARTESIAN_POINT('Ctrl Pts',(1.15461838959442,19.861915384356,1.65796695719522));
#37064=CARTESIAN_POINT('Ctrl Pts',(1.77352632078311,19.8656777419918,1.58295803460786));
#37065=CARTESIAN_POINT('Ctrl Pts',(2.32516508950545,19.8703010047203,1.48990196940852));
#37066=CARTESIAN_POINT('Ctrl Pts',(2.8138948184701,19.8753745609343,1.38699877184857));
#37067=CARTESIAN_POINT('Ctrl Pts',(3.25054101930003,19.880676768205,1.27877256646152));
#37068=CARTESIAN_POINT('Ctrl Pts',(3.64139477654928,19.8860335761906,1.16882675566282));
#37069=CARTESIAN_POINT('Ctrl Pts',(3.98999701978794,19.8912934545324,1.06033726777782));
#37070=CARTESIAN_POINT('Ctrl Pts',(4.29924266842479,19.8963351143492,0.955883447536127));
#37071=CARTESIAN_POINT('Ctrl Pts',(4.57314066596504,19.9010912851556,0.85694242225947));
#37072=CARTESIAN_POINT('Ctrl Pts',(4.81668173987254,19.9055469579917,0.763909702030878));
#37073=CARTESIAN_POINT('Ctrl Pts',(5.03479661632215,19.9097171082138,0.676556823383301));
#37074=CARTESIAN_POINT('Ctrl Pts',(5.23132099559656,19.913620337409,0.594589356922334));
#37075=CARTESIAN_POINT('Ctrl Pts',(5.40889737389929,19.9172693946253,0.517866823966847));
#37076=CARTESIAN_POINT('Ctrl Pts',(5.56944911393839,19.9206762302772,0.446330460231254));
#37077=CARTESIAN_POINT('Ctrl Pts',(5.70244460071722,19.9235937945899,0.385440459384885));
#37078=CARTESIAN_POINT('Ctrl Pts',(5.78208503334231,19.925402421831,0.348196348162051));
#37079=CARTESIAN_POINT('Ctrl Pts',(5.81359216867338,19.9261317941967,0.333334948402759));
#37080=CARTESIAN_POINT('Ctrl Pts',(-5.847868485275,19.7956126342212,0.401492685916237));
#37081=CARTESIAN_POINT('Ctrl Pts',(-5.8122174502919,19.7947531586782,0.418225605367972));
#37082=CARTESIAN_POINT('Ctrl Pts',(-5.69514385494066,19.7919721680002,0.472658902359452));
#37083=CARTESIAN_POINT('Ctrl Pts',(-5.4874901169821,19.7872465641152,0.566224573560217));
#37084=CARTESIAN_POINT('Ctrl Pts',(-5.21539943498523,19.7813114381313,0.683170401131284));
#37085=CARTESIAN_POINT('Ctrl Pts',(-4.91498607991476,19.7750554590008,0.805411723710539));
#37086=CARTESIAN_POINT('Ctrl Pts',(-4.58312097074267,19.7685149979094,0.932075987565472));
#37087=CARTESIAN_POINT('Ctrl Pts',(-4.21502610849436,19.761732954918,1.06228930799929));
#37088=CARTESIAN_POINT('Ctrl Pts',(-3.80511493092991,19.7547839595059,1.19456777190076));
#37089=CARTESIAN_POINT('Ctrl Pts',(-3.34838603989262,19.7478101772206,1.32613267716697));
#37090=CARTESIAN_POINT('Ctrl Pts',(-2.84069310068318,19.7410294174041,1.45278803968532));
#37091=CARTESIAN_POINT('Ctrl Pts',(-2.27729398886718,19.7347218891001,1.56923145151833));
#37092=CARTESIAN_POINT('Ctrl Pts',(-1.65097444995275,19.7292389106163,1.66896750324683));
#37093=CARTESIAN_POINT('Ctrl Pts',(-0.965445840826782,19.7251495498199,
1.74192179778576));
#37094=CARTESIAN_POINT('Ctrl Pts',(-0.243178106912335,19.7231013691965,
1.77728502764766));
#37095=CARTESIAN_POINT('Ctrl Pts',(0.477492972686614,19.7235284512799,1.77005561694156));
#37096=CARTESIAN_POINT('Ctrl Pts',(1.1610251436121,19.7261512068074,1.72418821081852));
#37097=CARTESIAN_POINT('Ctrl Pts',(1.78347110445064,19.7303114963596,1.64955010159841));
#37098=CARTESIAN_POINT('Ctrl Pts',(2.33831781824055,19.7353929949862,1.55686100196852));
#37099=CARTESIAN_POINT('Ctrl Pts',(2.82992627546618,19.7409454228058,1.45428842720372));
#37100=CARTESIAN_POINT('Ctrl Pts',(3.26917005572502,19.7467292925962,1.3463497158952));
#37101=CARTESIAN_POINT('Ctrl Pts',(3.66236643296839,19.752557244967,1.23664639117856));
#37102=CARTESIAN_POINT('Ctrl Pts',(4.01306968582882,19.7582663860018,1.1283545242984));
#37103=CARTESIAN_POINT('Ctrl Pts',(4.32418661922986,19.7637265282549,1.02405503991256));
#37104=CARTESIAN_POINT('Ctrl Pts',(4.59974676808851,19.7688658335805,0.925227997173997));
#37105=CARTESIAN_POINT('Ctrl Pts',(4.84476901005903,19.7736686618163,0.832272126158535));
#37106=CARTESIAN_POINT('Ctrl Pts',(5.06421316650717,19.7781513272396,0.744961377308228));
#37107=CARTESIAN_POINT('Ctrl Pts',(5.26193851821112,19.7823336930188,0.663002481750077));
#37108=CARTESIAN_POINT('Ctrl Pts',(5.44060507025142,19.7862292581127,0.586255387133592));
#37109=CARTESIAN_POINT('Ctrl Pts',(5.60215053682224,19.7898511514179,0.51466232923396));
#37110=CARTESIAN_POINT('Ctrl Pts',(5.73598092682063,19.7929396095604,0.453693790309014));
#37111=CARTESIAN_POINT('Ctrl Pts',(5.81613053652334,19.794848500999,0.416388245022623));
#37112=CARTESIAN_POINT('Ctrl Pts',(5.84784089926276,19.7956180079236,0.401501580201476));
#37113=CARTESIAN_POINT('',(-5.593361696257,19.9918770425327,0.136828655009776));
#37114=CARTESIAN_POINT('Ctrl Pts',(-5.593361696257,19.9918770425327,0.136828655009776));
#37115=CARTESIAN_POINT('Ctrl Pts',(-5.53989250493793,19.9909063803029,0.161641904267682));
#37116=CARTESIAN_POINT('Ctrl Pts',(-5.47940098468457,19.9898415697195,0.189256606818882));
#37117=CARTESIAN_POINT('Ctrl Pts',(-5.37813021090341,19.9881276870329,0.234751190678744));
#37118=CARTESIAN_POINT('Ctrl Pts',(-5.34261770407618,19.9875368930449,0.250586413051278));
#37119=CARTESIAN_POINT('Ctrl Pts',(-5.28671557048504,19.9866244477965,0.275255229834141));
#37120=CARTESIAN_POINT('Ctrl Pts',(-5.25810616035191,19.9861616644341,0.287817888230927));
#37121=CARTESIAN_POINT('Ctrl Pts',(-5.22850923521242,19.985689657541,0.300699531939207));
#37122=CARTESIAN_POINT('Ctrl Pts',(-5.20855850400689,19.9853730116806,0.309355137583069));
#37123=CARTESIAN_POINT('Ctrl Pts',(-5.19652326398584,19.9851830455075,0.314557421644312));
#37124=CARTESIAN_POINT('Ctrl Pts',(-5.12232129830657,19.984016616942,0.346539419230699));
#37125=CARTESIAN_POINT('Ctrl Pts',(-5.04967091219916,19.9829067581425,0.37727618564664));
#37126=CARTESIAN_POINT('Ctrl Pts',(-4.93065570811597,19.9811527268843,0.426450734116511));
#37127=CARTESIAN_POINT('Ctrl Pts',(-4.88931070260123,19.9805531897341,0.443349812440991));
#37128=CARTESIAN_POINT('Ctrl Pts',(-4.8247832880986,19.9796344794417,0.469375730136451));
#37129=CARTESIAN_POINT('Ctrl Pts',(-4.79189210428965,19.9791702786294,0.482557659797516));
#37130=CARTESIAN_POINT('Ctrl Pts',(-4.7524209725367,19.9786209356004,0.498210233032642));
#37131=CARTESIAN_POINT('Ctrl Pts',(-4.73526946950489,19.9783839180811,0.504974530200582));
#37132=CARTESIAN_POINT('Ctrl Pts',(-4.72378284443722,19.9782255634798,0.50949622404512));
#37133=CARTESIAN_POINT('Ctrl Pts',(-4.71687145440915,19.9781305474126,0.512210984265389));
#37134=CARTESIAN_POINT('Ctrl Pts',(-4.56330035730193,19.9760235555773,0.572436934549734));
#37135=CARTESIAN_POINT('Ctrl Pts',(-4.38742083373183,19.9737389649771,0.638489520363415));
#37136=CARTESIAN_POINT('Ctrl Pts',(-4.08315840426839,19.9701290451024,0.744581222725977));
#37137=CARTESIAN_POINT('Ctrl Pts',(-3.9749970704292,19.9688956929681,0.781076603721506));
#37138=CARTESIAN_POINT('Ctrl Pts',(-3.80264428364334,19.9670302858359,0.836644690767833));
#37139=CARTESIAN_POINT('Ctrl Pts',(-3.71394019374364,19.9660938405529,0.864631898693615));
#37140=CARTESIAN_POINT('Ctrl Pts',(-3.60602861997382,19.9650025232388,0.897417528954085));
#37141=CARTESIAN_POINT('Ctrl Pts',(-3.5509669658672,19.9644582409819,0.913813976195473));
#37142=CARTESIAN_POINT('Ctrl Pts',(-3.52713214255971,19.9642253903256,0.9208385631156));
#37143=CARTESIAN_POINT('Ctrl Pts',(-3.51118960001082,19.9640702618073,0.925520708479307));
#37144=CARTESIAN_POINT('Ctrl Pts',(-3.50199535538248,19.9639811993776,0.928210295796779));
#37145=CARTESIAN_POINT('Ctrl Pts',(-3.27669483698199,19.9618064517119,0.993913481638213));
#37146=CARTESIAN_POINT('Ctrl Pts',(-3.03027743164036,19.9596513714663,1.05988700948767));
#37147=CARTESIAN_POINT('Ctrl Pts',(-2.61873506056166,19.956611727738,1.15466812421503));
#37148=CARTESIAN_POINT('Ctrl Pts',(-2.47456822635772,19.9556313892423,1.18554057428783));
#37149=CARTESIAN_POINT('Ctrl Pts',(-2.24783890928523,19.954248203717,1.22962014666199));
#37150=CARTESIAN_POINT('Ctrl Pts',(-2.17051595929998,19.9538017251389,1.24394054524097));
#37151=CARTESIAN_POINT('Ctrl Pts',(-2.01237703740728,19.9529444659006,1.27163039886662));
#37152=CARTESIAN_POINT('Ctrl Pts',(-1.93359205710365,19.9525432774048,1.2846852665418));
#37153=CARTESIAN_POINT('Ctrl Pts',(-1.51062468474186,19.9505469283039,1.3501935639087));
#37154=CARTESIAN_POINT('Ctrl Pts',(-1.1559767801875,19.9493606967916,1.39097553980188));
#37155=CARTESIAN_POINT('Ctrl Pts',(-0.599593913358566,19.9483503734994,
1.42761012316683));
#37156=CARTESIAN_POINT('Ctrl Pts',(-0.410064456082688,19.9481405087443,
1.43573575542328));
#37157=CARTESIAN_POINT('Ctrl Pts',(-0.119667517669528,19.9480101389945,
1.44096891640077));
#37158=CARTESIAN_POINT('Ctrl Pts',(-0.0218514127819169,19.9479967936825,
1.44155464996756));
#37159=CARTESIAN_POINT('Ctrl Pts',(0.126398432674336,19.9480202849448,1.44059804455932));
#37160=CARTESIAN_POINT('Ctrl Pts',(0.200904777433672,19.9480432708496,1.43966102024194));
#37161=CARTESIAN_POINT('Ctrl Pts',(0.275983255239822,19.9480843551756,1.43801840811879));
#37162=CARTESIAN_POINT('Ctrl Pts',(0.326162714454324,19.9481158958946,1.43676464195432));
#37163=CARTESIAN_POINT('Ctrl Pts',(0.353068789789541,19.948135131383,1.43600374167174));
#37164=CARTESIAN_POINT('Ctrl Pts',(0.751958403002702,19.9484512736903,1.42356233146255));
#37165=CARTESIAN_POINT('Ctrl Pts',(1.10849134902751,19.9492390334456,1.39470318783279));
#37166=CARTESIAN_POINT('Ctrl Pts',(1.61495190962454,19.9510613632109,1.33320111122525));
#37167=CARTESIAN_POINT('Ctrl Pts',(1.861097475313,19.9521283565705,1.29790236789663));
#37168=CARTESIAN_POINT('Ctrl Pts',(2.13586905138197,19.9535982703747,1.25041701195131));
#37169=CARTESIAN_POINT('Ctrl Pts',(2.2509715302899,19.954270867413,1.22889001763999));
#37170=CARTESIAN_POINT('Ctrl Pts',(2.32711612334435,19.9547281407377,1.2142965170218));
#37171=CARTESIAN_POINT('Ctrl Pts',(2.36665276250411,19.9549723509007,1.20652523542265));
#37172=CARTESIAN_POINT('Ctrl Pts',(2.68815404361998,19.9570070374924,1.14194197153519));
#37173=CARTESIAN_POINT('Ctrl Pts',(2.94945525817411,19.9590254177359,1.07926628440836));
#37174=CARTESIAN_POINT('Ctrl Pts',(3.30469052701535,19.9621143428657,0.984758426877155));
#37175=CARTESIAN_POINT('Ctrl Pts',(3.41698285779743,19.9631547324302,0.953157125885748));
#37176=CARTESIAN_POINT('Ctrl Pts',(3.57624221572307,19.9647049245996,0.906369256589431));
#37177=CARTESIAN_POINT('Ctrl Pts',(3.65357711012402,19.9654774786032,0.883126997595109));
#37178=CARTESIAN_POINT('Ctrl Pts',(3.73978528060851,19.9663691056251,0.856422973430396));
#37179=CARTESIAN_POINT('Ctrl Pts',(3.77587109517688,19.9667486282055,0.845081023173003));
#37180=CARTESIAN_POINT('Ctrl Pts',(3.7997370728423,19.9670010068933,0.837544087199959));
#37181=CARTESIAN_POINT('Ctrl Pts',(3.80983216252252,19.967108252225,0.834343254624691));
#37182=CARTESIAN_POINT('Ctrl Pts',(4.03906084107691,19.9695588041822,0.761263843168769));
#37183=CARTESIAN_POINT('Ctrl Pts',(4.23305855301844,19.9718597199617,0.69347956345791));
#37184=CARTESIAN_POINT('Ctrl Pts',(4.49143473088391,19.975118797674,0.598683154613398));
#37185=CARTESIAN_POINT('Ctrl Pts',(4.57212339183127,19.976174096764,0.568208397480002));
#37186=CARTESIAN_POINT('Ctrl Pts',(4.68500128574059,19.9776937772282,0.524633828361888));
#37187=CARTESIAN_POINT('Ctrl Pts',(4.73940145831732,19.9784378450774,0.503378483467561));
#37188=CARTESIAN_POINT('Ctrl Pts',(4.79930047116214,19.9792750322337,0.479583707595788));
#37189=CARTESIAN_POINT('Ctrl Pts',(4.82420693627534,19.9796268695674,0.469606904472261));
#37190=CARTESIAN_POINT('Ctrl Pts',(4.84064134848598,19.979859844406,0.463005422732545));
#37191=CARTESIAN_POINT('Ctrl Pts',(4.84712299735739,19.9799519755852,0.460396313650406));
#37192=CARTESIAN_POINT('Ctrl Pts',(4.93440424623526,19.9811980255666,0.425138847862602));
#37193=CARTESIAN_POINT('Ctrl Pts',(5.00681738689788,19.9822679591127,0.395120032136794));
#37194=CARTESIAN_POINT('Ctrl Pts',(5.10768181038188,19.9837998500125,0.352584597767958));
#37195=CARTESIAN_POINT('Ctrl Pts',(5.15617520024639,19.984547618408,0.33193633916448));
#37196=CARTESIAN_POINT('Ctrl Pts',(5.20935788346942,19.9853851093829,0.309001644883203));
#37197=CARTESIAN_POINT('Ctrl Pts',(5.23142340378951,19.9857362363002,0.299424863669381));
#37198=CARTESIAN_POINT('Ctrl Pts',(5.24597218217979,19.9859685524309,0.293096892180794));
#37199=CARTESIAN_POINT('Ctrl Pts',(5.25210470606373,19.9860667644056,0.290424720766036));
#37200=CARTESIAN_POINT('Ctrl Pts',(5.39106103618176,19.9883011364273,0.229721734798504));
#37201=CARTESIAN_POINT('Ctrl Pts',(5.50208873233516,19.9902201029699,0.179185362360739));
#37202=CARTESIAN_POINT('Ctrl Pts',(5.593361696298,19.9918770423734,0.136828655185692));
#37203=CARTESIAN_POINT('',(-5.73644346265602,19.8089511587379,0.442548130347095));
#37204=CARTESIAN_POINT('Origin',(-5.599999999997,19.5919343769627,0.135488060674723));
#37205=CARTESIAN_POINT('Ctrl Pts',(-5.73644387762282,19.8089519016962,0.442549068003705));
#37206=CARTESIAN_POINT('Ctrl Pts',(-5.73644352459338,19.8089518943027,0.442549230097738));
#37207=CARTESIAN_POINT('Ctrl Pts',(-5.73644317156369,19.8089518869092,0.442549392191867));
#37208=CARTESIAN_POINT('Ctrl Pts',(-5.73644281853377,19.8089518795157,0.442549554286092));
#37209=CARTESIAN_POINT('Ctrl Pts',(-5.67992286962499,19.8077681857041,0.468500774395627));
#37210=CARTESIAN_POINT('Ctrl Pts',(-5.61717023492195,19.8064997493133,0.496914686516317));
#37211=CARTESIAN_POINT('Ctrl Pts',(-5.54808233593107,19.8051527504546,0.52755683616938));
#37212=CARTESIAN_POINT('Ctrl Pts',(-5.52952171320869,19.8047908761178,0.535788920042535));
#37213=CARTESIAN_POINT('Ctrl Pts',(-5.51050375561706,19.80442329013,0.54418155326481));
#37214=CARTESIAN_POINT('Ctrl Pts',(-5.49102627418781,19.8040500071028,0.552729586232965));
#37215=CARTESIAN_POINT('Ctrl Pts',(-5.42196512499331,19.8027264604764,0.583038277953587));
#37216=CARTESIAN_POINT('Ctrl Pts',(-5.34712803363965,19.8013311509866,0.615304462994705));
#37217=CARTESIAN_POINT('Ctrl Pts',(-5.26640545181662,19.7998746698034,0.649262108181634));
#37218=CARTESIAN_POINT('Ctrl Pts',(-5.25085819544196,19.7995941499557,0.655802387291616));
#37219=CARTESIAN_POINT('Ctrl Pts',(-5.23509257167142,19.7993113637113,0.662405262900947));
#37220=CARTESIAN_POINT('Ctrl Pts',(-5.21910773525063,19.799026390464,0.669068618256093));
#37221=CARTESIAN_POINT('Ctrl Pts',(-5.19133151721783,19.7985312037231,0.680647267314643));
#37222=CARTESIAN_POINT('Ctrl Pts',(-5.16289340246033,19.7980294106306,0.692408572678255));
#37223=CARTESIAN_POINT('Ctrl Pts',(-5.13378891178081,19.7975215466356,0.704340798761004));
#37224=CARTESIAN_POINT('Ctrl Pts',(-5.06602882589204,19.7963391549454,0.732121001930149));
#37225=CARTESIAN_POINT('Ctrl Pts',(-4.99465703432228,19.7951237786661,0.760829138131545));
#37226=CARTESIAN_POINT('Ctrl Pts',(-4.91961387572591,19.7938829721629,0.790301960627574));
#37227=CARTESIAN_POINT('Ctrl Pts',(-4.82892309834609,19.7923834389814,0.825920306573258));
#37228=CARTESIAN_POINT('Ctrl Pts',(-4.73287029248815,19.7908466413634,0.86265704234701));
#37229=CARTESIAN_POINT('Ctrl Pts',(-4.63134530184612,19.7892891516912,0.900178764352119));
#37230=CARTESIAN_POINT('Ctrl Pts',(-4.61739621649649,19.7890751594886,0.905334083248527));
#37231=CARTESIAN_POINT('Ctrl Pts',(-4.60334382008669,19.7888607816979,0.910504140875635));
#37232=CARTESIAN_POINT('Ctrl Pts',(-4.58918781805959,19.7886460662023,0.915687994968418));
#37233=CARTESIAN_POINT('Ctrl Pts',(-4.55700503480212,19.7881579239823,0.927473162305002));
#37234=CARTESIAN_POINT('Ctrl Pts',(-4.52428676573379,19.7876680341698,0.939329672314043));
#37235=CARTESIAN_POINT('Ctrl Pts',(-4.49102962640135,19.7871769736762,0.951246087558308));
#37236=CARTESIAN_POINT('Ctrl Pts',(-4.45062022386591,19.7865803059666,0.965725240908554));
#37237=CARTESIAN_POINT('Ctrl Pts',(-4.40941525025059,19.785981907784,0.980292870178383));
#37238=CARTESIAN_POINT('Ctrl Pts',(-4.36740858669668,19.7853828849297,0.994927388978708));
#37239=CARTESIAN_POINT('Ctrl Pts',(-4.34640525491973,19.7850833735025,1.00224464837887));
#37240=CARTESIAN_POINT('Ctrl Pts',(-4.3252014967549,19.7847836982241,1.00957861859033));
#37241=CARTESIAN_POINT('Ctrl Pts',(-4.30379654745358,19.784484014967,1.01692648002813));
#37242=CARTESIAN_POINT('Ctrl Pts',(-4.29309407280291,19.7843341733384,1.02060041074704));
#37243=CARTESIAN_POINT('Ctrl Pts',(-4.28234130011502,19.7841843292229,1.02427781353311));
#37244=CARTESIAN_POINT('Ctrl Pts',(-4.27153813309606,19.7840345010304,1.02795832991866));
#37245=CARTESIAN_POINT('Ctrl Pts',(-4.26343575783185,19.783922129886,1.03071871720782));
#37246=CARTESIAN_POINT('Ctrl Pts',(-4.25530503573597,19.7838097676575,1.03348085583515));
#37247=CARTESIAN_POINT('Ctrl Pts',(-4.24714592611223,19.783697422145,1.03624459284066));
#37248=CARTESIAN_POINT('Ctrl Pts',(-4.24442622290431,19.7836599736408,1.03716583850916));
#37249=CARTESIAN_POINT('Ctrl Pts',(-4.24040661893564,19.7836047149147,1.0385256585289));
#37250=CARTESIAN_POINT('Ctrl Pts',(-4.23897735248378,19.7835850825318,1.03900885687057));
#37251=CARTESIAN_POINT('Ctrl Pts',(-4.23364029621417,19.7835117728056,1.04081317875577));
#37252=CARTESIAN_POINT('Ctrl Pts',(-4.22827896813906,19.7834382575236,1.04262230666689));
#37253=CARTESIAN_POINT('Ctrl Pts',(-4.22289334196019,19.7833645409097,1.04443615539268));
#37254=CARTESIAN_POINT('Ctrl Pts',(-4.1421104893463,19.7822588127816,1.07164336759298));
#37255=CARTESIAN_POINT('Ctrl Pts',(-4.05586117002453,19.7811075541515,1.09991688725499));
#37256=CARTESIAN_POINT('Ctrl Pts',(-3.96405547488631,19.7799263402454,1.12894309340335));
#37257=CARTESIAN_POINT('Ctrl Pts',(-3.91582473643939,19.7793057815875,1.14419220572412));
#37258=CARTESIAN_POINT('Ctrl Pts',(-3.86606035830127,19.7786770017245,1.15964822680068));
#37259=CARTESIAN_POINT('Ctrl Pts',(-3.81474889150123,19.7780425864392,1.17525989420485));
#37260=CARTESIAN_POINT('Ctrl Pts',(-3.71991638549903,19.7768700767626,1.20411296809142));
#37261=CARTESIAN_POINT('Ctrl Pts',(-3.61979927953566,19.7756781491646,1.23350071191893));
#37262=CARTESIAN_POINT('Ctrl Pts',(-3.51431514211601,19.7744850775374,1.26306249208537));
#37263=CARTESIAN_POINT('Ctrl Pts',(-3.46378927585294,19.7739136079407,1.27722229457061));
#37264=CARTESIAN_POINT('Ctrl Pts',(-3.41203205809547,19.7733419177578,1.29142128195551));
#37265=CARTESIAN_POINT('Ctrl Pts',(-3.35903461288398,19.7727722569973,1.30561555713677));
#37266=CARTESIAN_POINT('Ctrl Pts',(-3.24836436657796,19.7715826808503,1.33525630536862));
#37267=CARTESIAN_POINT('Ctrl Pts',(-3.13228530905258,19.7704017483376,1.3648801206481));
#37268=CARTESIAN_POINT('Ctrl Pts',(-3.01072581908244,19.7692520506645,1.39404921923668));
#37269=CARTESIAN_POINT('Ctrl Pts',(-2.9685701696663,19.768853346688,1.40416477906823));
#37270=CARTESIAN_POINT('Ctrl Pts',(-2.92501774452437,19.7684516393367,1.41439775540621));
#37271=CARTESIAN_POINT('Ctrl Pts',(-2.88136966635236,19.7680601552779,1.42441930906165));
#37272=CARTESIAN_POINT('Ctrl Pts',(-2.8718037250264,19.7679743573758,1.42661563930751));
#37273=CARTESIAN_POINT('Ctrl Pts',(-2.86223323801364,19.76788904089,1.42880200705198));
#37274=CARTESIAN_POINT('Ctrl Pts',(-2.85267198306032,19.7678043285989,1.43097527914219));
#37275=CARTESIAN_POINT('Ctrl Pts',(-2.83185440261412,19.7676198857676,1.43570711265048));
#37276=CARTESIAN_POINT('Ctrl Pts',(-2.81108054715055,19.7674383160755,1.44037668862943));
#37277=CARTESIAN_POINT('Ctrl Pts',(-2.79049311401335,19.7672607865354,1.44495366167414));
#37278=CARTESIAN_POINT('Ctrl Pts',(-2.6196797742614,19.7657878290548,1.48292867519389));
#37279=CARTESIAN_POINT('Ctrl Pts',(-2.45352912167896,19.7645067104381,1.51637189968607));
#37280=CARTESIAN_POINT('Ctrl Pts',(-2.29228332637382,19.7633930739181,1.54580449579569));
#37281=CARTESIAN_POINT('Ctrl Pts',(-2.12993500746006,19.7622718228706,1.57543833828207));
#37282=CARTESIAN_POINT('Ctrl Pts',(-1.97255885581796,19.761320314212,1.60100751447628));
#37283=CARTESIAN_POINT('Ctrl Pts',(-1.82036290435247,19.7605129043991,1.62305465711288));
#37284=CARTESIAN_POINT('Ctrl Pts',(-1.76978200408601,19.7602445693034,1.63038181865774));
#37285=CARTESIAN_POINT('Ctrl Pts',(-1.71977283800279,19.7599921471886,1.63731986544404));
#37286=CARTESIAN_POINT('Ctrl Pts',(-1.6703418370121,19.7597546916422,1.64388836755662));
#37287=CARTESIAN_POINT('Ctrl Pts',(-1.52110170714283,19.7590377752158,1.66371973023757));
#37288=CARTESIAN_POINT('Ctrl Pts',(-1.3771352506761,19.7584572456274,1.68018464462649));
#37289=CARTESIAN_POINT('Ctrl Pts',(-1.23859807970654,19.7579867069053,1.69382332829766));
#37290=CARTESIAN_POINT('Ctrl Pts',(-1.14893751809387,19.7576821766064,1.7026502159052));
#37291=CARTESIAN_POINT('Ctrl Pts',(-1.06155007351066,19.7574237245106,1.71029278196188));
#37292=CARTESIAN_POINT('Ctrl Pts',(-0.976468268211634,19.7572043404281,
1.71689112254408));
#37293=CARTESIAN_POINT('Ctrl Pts',(-0.844577106193146,19.7568642580631,
1.7271196644012));
#37294=CARTESIAN_POINT('Ctrl Pts',(-0.71822817214218,19.7566180411509,1.73484113748309));
#37295=CARTESIAN_POINT('Ctrl Pts',(-0.597515581883815,19.75644118749,1.74056201975772));
#37296=CARTESIAN_POINT('Ctrl Pts',(-0.480867236251215,19.7562702882746,
1.74609028695394));
#37297=CARTESIAN_POINT('Ctrl Pts',(-0.369481483391001,19.7561641382709,
1.74975029480863));
#37298=CARTESIAN_POINT('Ctrl Pts',(-0.263414069157,19.756101348382,1.75196323556012));
#37299=CARTESIAN_POINT('Ctrl Pts',(-0.25575142503431,19.7560968122427,1.7521231053709));
#37300=CARTESIAN_POINT('Ctrl Pts',(-0.248116526890297,19.756092502804,1.75227540725386));
#37301=CARTESIAN_POINT('Ctrl Pts',(-0.240509390808347,19.7560884122148,
1.75242029269565));
#37302=CARTESIAN_POINT('Ctrl Pts',(-0.202051679845121,19.7560677323299,
1.75315275789451));
#37303=CARTESIAN_POINT('Ctrl Pts',(-0.164303537530501,19.75605264159,1.75369573568429));
#37304=CARTESIAN_POINT('Ctrl Pts',(-0.12726676960698,19.756042009416,1.75406883492907));
#37305=CARTESIAN_POINT('Ctrl Pts',(-0.105085352581457,19.7560356417792,
1.75429228504106));
#37306=CARTESIAN_POINT('Ctrl Pts',(-0.083159099614591,19.756030865463,1.75445479314168));
#37307=CARTESIAN_POINT('Ctrl Pts',(-0.0614883187664068,19.7560274595648,
1.75456043379643));
#37308=CARTESIAN_POINT('Ctrl Pts',(-0.0416894052580165,19.7560243478595,
1.75465694947812));
#37309=CARTESIAN_POINT('Ctrl Pts',(-0.023098772166832,19.7560224658573,
1.75470533215409));
#37310=CARTESIAN_POINT('Ctrl Pts',(-0.00298939254024861,19.7560213847532,
1.75471055941785));
#37311=CARTESIAN_POINT('Ctrl Pts',(-0.00108817250963598,19.7560212825414,
1.75471105362397));
#37312=CARTESIAN_POINT('Ctrl Pts',(0.000826622955876557,19.7560211896314,
1.75471112377803));
#37313=CARTESIAN_POINT('Ctrl Pts',(0.00275729841146969,19.7560211070343,
1.75471074952977));
#37314=CARTESIAN_POINT('Ctrl Pts',(0.115372251369809,19.7560162891981,1.75468891989025));
#37315=CARTESIAN_POINT('Ctrl Pts',(0.233541293580167,19.756051648623,1.75316490828795));
#37316=CARTESIAN_POINT('Ctrl Pts',(0.357210305664608,19.7561526751189,1.74966615574549));
#37317=CARTESIAN_POINT('Ctrl Pts',(0.400712688642062,19.7561882126658,1.74843541838874));
#37318=CARTESIAN_POINT('Ctrl Pts',(0.444895373831161,19.7562318941872,1.7469599398188));
#37319=CARTESIAN_POINT('Ctrl Pts',(0.489755120375023,19.7562848885263,1.74521788431246));
#37320=CARTESIAN_POINT('Ctrl Pts',(0.617020182699277,19.7564352310579,1.74027575200749));
#37321=CARTESIAN_POINT('Ctrl Pts',(0.749737195266465,19.7566605042835,1.7331905062554));
#37322=CARTESIAN_POINT('Ctrl Pts',(0.887807199413158,19.7569855787757,1.72345410257963));
#37323=CARTESIAN_POINT('Ctrl Pts',(0.982313920912144,19.7572080870946,1.71678968914476));
#37324=CARTESIAN_POINT('Ctrl Pts',(1.0793279137614,19.757477368534,1.70888243905592));
#37325=CARTESIAN_POINT('Ctrl Pts',(1.17880639802586,19.7578014745625,1.69956056995609));
#37326=CARTESIAN_POINT('Ctrl Pts',(1.32359504506791,19.7582732034364,1.6859928037718));
#37327=CARTESIAN_POINT('Ctrl Pts',(1.47360658000716,19.7588610528274,1.66942884858532));
#37328=CARTESIAN_POINT('Ctrl Pts',(1.62867912020213,19.759591057639,1.64933425855342));
#37329=CARTESIAN_POINT('Ctrl Pts',(1.68661969450315,19.7598638132022,1.6418262104791));
#37330=CARTESIAN_POINT('Ctrl Pts',(1.745266335463,19.7601564163829,1.63382506353029));
#37331=CARTESIAN_POINT('Ctrl Pts',(1.80460884493939,19.7604702288167,1.62530222939973));
#37332=CARTESIAN_POINT('Ctrl Pts',(1.96234369330212,19.7613043552649,1.60264818323506));
#37333=CARTESIAN_POINT('Ctrl Pts',(2.12499858771291,19.7622883739304,1.57630875695046));
#37334=CARTESIAN_POINT('Ctrl Pts',(2.29235845918953,19.7634470127006,1.54575752526289));
#37335=CARTESIAN_POINT('Ctrl Pts',(2.31272979552248,19.7635880442386,1.54203877589601));
#37336=CARTESIAN_POINT('Ctrl Pts',(2.33317077852849,19.7637316621987,1.53825761547812));
#37337=CARTESIAN_POINT('Ctrl Pts',(2.35368096675343,19.7638779104546,1.53441308861661));
#37338=CARTESIAN_POINT('Ctrl Pts',(2.36244932396459,19.763940433379,1.53276950619505));
#37339=CARTESIAN_POINT('Ctrl Pts',(2.37123032943377,19.7640034370317,1.53111434247959));
#37340=CARTESIAN_POINT('Ctrl Pts',(2.38002394991334,19.7640669248047,1.52944752508434));
#37341=CARTESIAN_POINT('Ctrl Pts',(2.44796163818883,19.7645574181728,1.51657003953969));
#37342=CARTESIAN_POINT('Ctrl Pts',(2.516652401437,19.7650768099106,1.50299696253616));
#37343=CARTESIAN_POINT('Ctrl Pts',(2.58608013114986,19.7656266494358,1.48869496643244));
#37344=CARTESIAN_POINT('Ctrl Pts',(2.6207939960063,19.7659015691984,1.48154396838058));
#37345=CARTESIAN_POINT('Ctrl Pts',(2.65569210204061,19.7661840995595,1.47421073840017));
#37346=CARTESIAN_POINT('Ctrl Pts',(2.69077227963222,19.766474432379,1.46669112701405));
#37347=CARTESIAN_POINT('Ctrl Pts',(2.70831236842803,19.7666195987888,1.46293132132099));
#37348=CARTESIAN_POINT('Ctrl Pts',(2.72589797509413,19.766766715751,1.45912492017669));
#37349=CARTESIAN_POINT('Ctrl Pts',(2.74352882315658,19.7669158068842,1.45527140537114));
#37350=CARTESIAN_POINT('Ctrl Pts',(2.75885335747361,19.7670453952159,1.45192197375732));
#37351=CARTESIAN_POINT('Ctrl Pts',(2.77563086515661,19.7671886585484,1.44822226782758));
#37352=CARTESIAN_POINT('Ctrl Pts',(2.79016150548294,19.7673138554393,1.44499224823921));
#37353=CARTESIAN_POINT('Ctrl Pts',(2.79234833966799,19.7673326973371,1.44450613633391));
#37354=CARTESIAN_POINT('Ctrl Pts',(2.79448430511413,19.767351125253,1.4440307576573));
#37355=CARTESIAN_POINT('Ctrl Pts',(2.79655681221918,19.7673690262237,1.44356900191366));
#37356=CARTESIAN_POINT('Ctrl Pts',(2.81154965113721,19.7674985246312,1.44022858900649));
#37357=CARTESIAN_POINT('Ctrl Pts',(2.82653642438921,19.7676292907192,1.43686249766563));
#37358=CARTESIAN_POINT('Ctrl Pts',(2.84151705021888,19.7677613187565,1.43347080813785));
#37359=CARTESIAN_POINT('Ctrl Pts',(2.98776394153726,19.7690502295293,1.40035977156335));
#37360=CARTESIAN_POINT('Ctrl Pts',(3.13342495769287,19.7704594133585,1.3648091206432));
#37361=CARTESIAN_POINT('Ctrl Pts',(3.2784330609518,19.7719831585219,1.32690145389342));
#37362=CARTESIAN_POINT('Ctrl Pts',(3.40982133405652,19.7733637865086,1.29255425011828));
#37363=CARTESIAN_POINT('Ctrl Pts',(3.54067358326317,19.7748384660325,1.25627200018786));
#37364=CARTESIAN_POINT('Ctrl Pts',(3.67094621226374,19.7764026120794,1.21812030633583));
#37365=CARTESIAN_POINT('Ctrl Pts',(3.7881200872732,19.7778094851487,1.18380471877831));
#37366=CARTESIAN_POINT('Ctrl Pts',(3.90482504209593,19.7792887378654,1.1479767276728));
#37367=CARTESIAN_POINT('Ctrl Pts',(4.02103364167433,19.7808367149258,1.11068613714232));
#37368=CARTESIAN_POINT('Ctrl Pts',(4.12467629572365,19.7822173051019,1.07742787753273));
#37369=CARTESIAN_POINT('Ctrl Pts',(4.2279241350384,19.7836525606924,1.04300622655274));
#37370=CARTESIAN_POINT('Ctrl Pts',(4.33076048984269,19.785139615806,1.0074574580962));
#37371=CARTESIAN_POINT('Ctrl Pts',(4.42239072069803,19.7864646258533,0.975782454966282));
#37372=CARTESIAN_POINT('Ctrl Pts',(4.51369425993899,19.7878307615007,0.943212595677556));
#37373=CARTESIAN_POINT('Ctrl Pts',(4.60466112206805,19.7892357879126,0.909773922350126));
#37374=CARTESIAN_POINT('Ctrl Pts',(4.68608243726572,19.7904933788162,0.879844113878531));
#37375=CARTESIAN_POINT('Ctrl Pts',(4.76723402584457,19.7917821269742,0.849218261921288));
#37376=CARTESIAN_POINT('Ctrl Pts',(4.8481099504637,19.7931003253408,0.817915114826047));
#37377=CARTESIAN_POINT('Ctrl Pts',(4.92103350007437,19.7942889077828,0.789689946323553));
#37378=CARTESIAN_POINT('Ctrl Pts',(4.99373293117401,19.7955014337815,0.760914129013177));
#37379=CARTESIAN_POINT('Ctrl Pts',(5.06620476601318,19.7967367222911,0.7316012532215));
#37380=CARTESIAN_POINT('Ctrl Pts',(5.13210508904211,19.7978599988302,0.704946374290041));
#37381=CARTESIAN_POINT('Ctrl Pts',(5.19781721936355,19.7990020970862,0.677847418887374));
#37382=CARTESIAN_POINT('Ctrl Pts',(5.26333917796051,19.8001625171985,0.650314189646983));
#37383=CARTESIAN_POINT('Ctrl Pts',(5.32292135272205,19.8012177413617,0.62527693936511));
#37384=CARTESIAN_POINT('Ctrl Pts',(5.38234627172783,19.8022881159988,0.599880583260539));
#37385=CARTESIAN_POINT('Ctrl Pts',(5.44161281821192,19.8033742625133,0.574131675940057));
#37386=CARTESIAN_POINT('Ctrl Pts',(5.4953806268887,19.804359636581,0.550771746864127));
#37387=CARTESIAN_POINT('Ctrl Pts',(5.54901808656126,19.8053579912684,0.527121650695065));
#37388=CARTESIAN_POINT('Ctrl Pts',(5.60252433633247,19.8063718735624,0.503184808992108));
#37389=CARTESIAN_POINT('Ctrl Pts',(5.64725600054545,19.8072194874863,0.483173412754208));
#37390=CARTESIAN_POINT('Ctrl Pts',(5.69189596083383,19.8080779529814,0.462961605831743));
#37391=CARTESIAN_POINT('Ctrl Pts',(5.73644276371326,19.8089520713578,0.442549442048373));
#37392=CARTESIAN_POINT('Ctrl Pts',(-5.843530256069,19.9729830063932,0.275592041905464));
#37393=CARTESIAN_POINT('Ctrl Pts',(-3.895686837379,19.9313476995223,1.19822036162746));
#37394=CARTESIAN_POINT('Ctrl Pts',(0.0001633689301563,19.8897491923651,
2.12096446775537));
#37395=CARTESIAN_POINT('Ctrl Pts',(3.896013575239,19.9313511884663,1.19814296951903));
#37396=CARTESIAN_POINT('Ctrl Pts',(5.844020362859,19.9729934829082,0.27535988496917));
#37397=CARTESIAN_POINT('Ctrl Pts',(-5.843530256069,19.2592933206554,0.803936154133969));
#37398=CARTESIAN_POINT('Ctrl Pts',(-3.895686837379,19.2409363277008,1.65690464245717));
#37399=CARTESIAN_POINT('Ctrl Pts',(0.0001633689301563,19.2238042428705,
2.51235960005451));
#37400=CARTESIAN_POINT('Ctrl Pts',(3.896013575239,19.2409377645976,1.65683289399886));
#37401=CARTESIAN_POINT('Ctrl Pts',(5.844020362859,19.2592979397557,0.803721525417513));
#37402=CARTESIAN_POINT('Ctrl Pts',(-5.843530256069,17.6858134778517,1.67939840409943));
#37403=CARTESIAN_POINT('Ctrl Pts',(-3.895686837379,17.747795303743,2.42360809969946));
#37404=CARTESIAN_POINT('Ctrl Pts',(0.0001633689301563,17.8092308148508,
3.16660344766129));
#37405=CARTESIAN_POINT('Ctrl Pts',(3.896013575239,17.7477901510419,2.42354578341948));
#37406=CARTESIAN_POINT('Ctrl Pts',(5.844020362859,17.6857978816304,1.67921114184714));
#37407=CARTESIAN_POINT('Ctrl Pts',(-5.843530256069,15.061425464425,2.34071387945854));
#37408=CARTESIAN_POINT('Ctrl Pts',(-3.895686837379,15.2991206306999,3.03320174206447));
#37409=CARTESIAN_POINT('Ctrl Pts',(0.0001633689301563,15.5368877409622,
3.72636654306873));
#37410=CARTESIAN_POINT('Ctrl Pts',(3.896013575239,15.2991006887715,3.03314360515765));
#37411=CARTESIAN_POINT('Ctrl Pts',(5.844020362859,15.0613656542254,2.34053963176309));
#37412=CARTESIAN_POINT('Ctrl Pts',(-5.843530256069,12.4568749910185,2.30089104535593));
#37413=CARTESIAN_POINT('Ctrl Pts',(-3.895686837379,12.8710990247508,3.06727942102254));
#37414=CARTESIAN_POINT('Ctrl Pts',(0.0001633689301563,13.2856337337471,
3.83244175204731));
#37415=CARTESIAN_POINT('Ctrl Pts',(3.896013575239,12.8710642570284,3.06721524556422));
#37416=CARTESIAN_POINT('Ctrl Pts',(5.844020362859,12.4567707616288,2.30069820237451));
#37417=CARTESIAN_POINT('Ctrl Pts',(-5.843530256069,10.8186489886147,1.86225011026657));
#37418=CARTESIAN_POINT('Ctrl Pts',(-3.895686837379,11.3231612494621,2.74792678860542));
#37419=CARTESIAN_POINT('Ctrl Pts',(0.0001633689301563,11.8270703511712,
3.63585972809697));
#37420=CARTESIAN_POINT('Ctrl Pts',(3.896013575239,11.3231189857497,2.74785231616274));
#37421=CARTESIAN_POINT('Ctrl Pts',(5.844020362859,10.8185220403858,1.86202725132894));
#37422=CARTESIAN_POINT('Ctrl Pts',(-5.843530256069,10.0864302299624,1.57297372755727));
#37423=CARTESIAN_POINT('Ctrl Pts',(-3.895686837379,10.6220961848295,2.52888112716319));
#37424=CARTESIAN_POINT('Ctrl Pts',(0.0001633689301563,11.1575638447486,
3.48561783754201));
#37425=CARTESIAN_POINT('Ctrl Pts',(3.896013575239,10.6220512742479,2.52880088403233));
#37426=CARTESIAN_POINT('Ctrl Pts',(5.844020362859,10.0862954426721,1.57273319675619));
#37427=CARTESIAN_POINT('',(-5.73278769720861,10.3449530899586,1.712890664259));
#37428=CARTESIAN_POINT('Ctrl Pts',(-5.73644356954166,19.8089503607377,0.442546999707748));
#37429=CARTESIAN_POINT('Ctrl Pts',(-5.73766037024446,19.1301825683204,0.92173330072201));
#37430=CARTESIAN_POINT('Ctrl Pts',(-5.73849618482638,18.3938460451307,1.3183902211696));
#37431=CARTESIAN_POINT('Ctrl Pts',(-5.73940756701135,16.8491829816311,1.92343296529744));
#37432=CARTESIAN_POINT('Ctrl Pts',(-5.739483134547,16.0408992661184,2.13191056540138));
#37433=CARTESIAN_POINT('Ctrl Pts',(-5.73887402246419,14.4000963224447,2.35028699819193));
#37434=CARTESIAN_POINT('Ctrl Pts',(-5.73818934284575,13.5675419891499,2.35984313691093));
#37435=CARTESIAN_POINT('Ctrl Pts',(-5.73605973645477,11.9265541605029,2.18169283770349));
#37436=CARTESIAN_POINT('Ctrl Pts',(-5.73461480968224,11.1182366055945,1.99332811253109));
#37437=CARTESIAN_POINT('Ctrl Pts',(-5.732787914148,10.3449528797153,1.71289124180765));
#37438=CARTESIAN_POINT('Ctrl Pts',(5.73278688072817,10.3449507250975,1.71289711535081));
#37439=CARTESIAN_POINT('Ctrl Pts',(5.37900915639315,10.4448363651221,1.88168165915975));
#37440=CARTESIAN_POINT('Ctrl Pts',(5.01621168019062,10.5336327228737,2.03732074407881));
#37441=CARTESIAN_POINT('Ctrl Pts',(4.64600744793163,10.6117450667191,2.17807213827088));
#37442=CARTESIAN_POINT('Ctrl Pts',(4.37165126939791,10.6696336651907,2.28238216843503));
#37443=CARTESIAN_POINT('Ctrl Pts',(4.0932271486741,10.7216541652371,2.3785116388909));
#37444=CARTESIAN_POINT('Ctrl Pts',(3.81139161388638,10.7679952015392,2.4657654271308));
#37445=CARTESIAN_POINT('Ctrl Pts',(3.57235159836392,10.8072995498901,2.53977010120772));
#37446=CARTESIAN_POINT('Ctrl Pts',(3.33085752862551,10.8425181299936,2.60738913673008));
#37447=CARTESIAN_POINT('Ctrl Pts',(3.08730997420282,10.8737883242848,2.66823233499462));
#37448=CARTESIAN_POINT('Ctrl Pts',(3.04370746675433,10.8793866514071,2.6791251399411));
#37449=CARTESIAN_POINT('Ctrl Pts',(3.00003914097686,10.8848584940772,2.68980088077536));
#37450=CARTESIAN_POINT('Ctrl Pts',(2.95630729545765,10.890204737468,2.7002574814574));
#37451=CARTESIAN_POINT('Ctrl Pts',(2.75784869263507,10.9144664163677,2.74771036932422));
#37452=CARTESIAN_POINT('Ctrl Pts',(2.55807717076884,10.9362024498221,2.79066539146926));
#37453=CARTESIAN_POINT('Ctrl Pts',(2.35725950625594,10.9553925153308,2.82890669523075));
#37454=CARTESIAN_POINT('Ctrl Pts',(2.16328572644567,10.9739285816203,2.86584473179981));
#37455=CARTESIAN_POINT('Ctrl Pts',(1.96833589422108,10.9900892362504,2.8983848066184));
#37456=CARTESIAN_POINT('Ctrl Pts',(1.77265042967068,11.0038798224107,2.92637432499266));
#37457=CARTESIAN_POINT('Ctrl Pts',(1.58005635303568,11.0174525484887,2.953921672258));
#37458=CARTESIAN_POINT('Ctrl Pts',(1.3867497031393,11.0287294251743,2.9770609588758));
#37459=CARTESIAN_POINT('Ctrl Pts',(1.19295968484454,11.0377396538332,2.99568970691917));
#37460=CARTESIAN_POINT('Ctrl Pts',(0.994821339892144,11.046952057082,3.01473645317746));
#37461=CARTESIAN_POINT('Ctrl Pts',(0.79617769120483,11.0537947132516,3.02906753346601));
#37462=CARTESIAN_POINT('Ctrl Pts',(0.597273721365771,11.0583268153071,3.03862354819703));
#37463=CARTESIAN_POINT('Ctrl Pts',(0.408482784336276,11.0626284880916,3.04769369886722));
#37464=CARTESIAN_POINT('Ctrl Pts',(0.219457324631945,11.0648487064693,3.05246221354261));
#37465=CARTESIAN_POINT('Ctrl Pts',(0.030406825010438,11.0650633093697,3.05292359624673));
#37466=CARTESIAN_POINT('Ctrl Pts',(0.0202798881170744,11.0650748050814,
3.0529483113019));
#37467=CARTESIAN_POINT('Ctrl Pts',(0.0101528793726079,11.0650805518247,
3.0529606781068));
#37468=CARTESIAN_POINT('Ctrl Pts',(2.58309765375194E-5,11.0650805633313,
3.0529606995424));
#37469=CARTESIAN_POINT('Ctrl Pts',(1.72206505356609E-5,11.0650805633411,
3.05296069956063));
#37470=CARTESIAN_POINT('Ctrl Pts',(8.6103245629562E-6,11.0650805633467,
3.05296069956993));
#37471=CARTESIAN_POINT('Ctrl Pts',(-1.38233868796078E-12,11.0650805633482,
3.05296069957031));
#37472=CARTESIAN_POINT('Ctrl Pts',(-0.189404607484898,11.0650805961548,
3.05296070785262));
#37473=CARTESIAN_POINT('Ctrl Pts',(-0.378795525024171,11.0630723256102,
3.0486385112057));
#37474=CARTESIAN_POINT('Ctrl Pts',(-0.567962091433974,11.0589781342605,
3.03999720067297));
#37475=CARTESIAN_POINT('Ctrl Pts',(-0.769360885412324,11.0546191969715,
3.03079711023038));
#37476=CARTESIAN_POINT('Ctrl Pts',(-0.970505375368339,11.0478956606748,
3.01670092928917));
#37477=CARTESIAN_POINT('Ctrl Pts',(-1.17114133412378,11.0387447797368,2.99776792292822));
#37478=CARTESIAN_POINT('Ctrl Pts',(-1.36695479531859,11.0298138499047,2.97928999140808));
#37479=CARTESIAN_POINT('Ctrl Pts',(-1.56228387768899,11.0185711098174,2.95620541448577));
#37480=CARTESIAN_POINT('Ctrl Pts',(-1.75689224881912,11.0049856060652,2.92861833910982));
#37481=CARTESIAN_POINT('Ctrl Pts',(-1.95868984781945,10.9908982262547,2.90001214122645));
#37482=CARTESIAN_POINT('Ctrl Pts',(-2.15971250294576,10.974291784558,2.86656464096982));
#37483=CARTESIAN_POINT('Ctrl Pts',(-2.35969671049328,10.9551601078216,2.82844251062265));
#37484=CARTESIAN_POINT('Ctrl Pts',(-2.5596809180408,10.9360284310852,2.79032038027548));
#37485=CARTESIAN_POINT('Ctrl Pts',(-2.75862667800953,10.9143716955401,2.74752395482592));
#37486=CARTESIAN_POINT('Ctrl Pts',(-2.95627048669471,10.8902100153768,2.70026650193579));
#37487=CARTESIAN_POINT('Ctrl Pts',(-3.19876727229057,10.8605651212961,2.6422845165777));
#37488=CARTESIAN_POINT('Ctrl Pts',(-3.43931126880089,10.8270560244705,2.57756053855471));
#37489=CARTESIAN_POINT('Ctrl Pts',(-3.6775105439921,10.7895434778164,2.50646830223344));
#37490=CARTESIAN_POINT('Ctrl Pts',(-3.96232663863318,10.7446895334477,2.42146295076009));
#37491=CARTESIAN_POINT('Ctrl Pts',(-4.24379045999574,10.6941119076844,2.3273536438739));
#37492=CARTESIAN_POINT('Ctrl Pts',(-4.5212319950369,10.6376130683546,2.22484295869238));
#37493=CARTESIAN_POINT('Ctrl Pts',(-4.88826612190385,10.5628693852961,2.08922909026223));
#37494=CARTESIAN_POINT('Ctrl Pts',(-5.24826073085707,10.4777633055356,1.93891800459309));
#37495=CARTESIAN_POINT('Ctrl Pts',(-5.59966454915396,10.3818999325314,1.77558871976231));
#37496=CARTESIAN_POINT('Ctrl Pts',(-5.64417852204767,10.3697564686154,1.75489903177615));
#37497=CARTESIAN_POINT('Ctrl Pts',(-5.68855464299647,10.3574404414096,1.73400040081192));
#37498=CARTESIAN_POINT('Ctrl Pts',(-5.73278975875473,10.3449510884962,1.71289616977594));
#37499=CARTESIAN_POINT('Ctrl Pts',(5.84420424599312,10.3325630763309,1.66676549536465));
#37500=CARTESIAN_POINT('Ctrl Pts',(5.38649680477895,10.4714443877546,1.89197696257757));
#37501=CARTESIAN_POINT('Ctrl Pts',(4.35413199008094,10.731355617357,2.33432632451635));
#37502=CARTESIAN_POINT('Ctrl Pts',(2.6892293910766,10.9922428541574,2.81982521043073));
#37503=CARTESIAN_POINT('Ctrl Pts',(0.897914376059795,11.1229571043403,3.07976795890079));
#37504=CARTESIAN_POINT('Ctrl Pts',(-0.894835170638287,11.123066538772,3.07999087254476));
#37505=CARTESIAN_POINT('Ctrl Pts',(-2.68616412898614,10.9925867227746,2.82049345526273));
#37506=CARTESIAN_POINT('Ctrl Pts',(-4.35222081536794,10.7317832826312,2.33508087721848));
#37507=CARTESIAN_POINT('Ctrl Pts',(-5.38563860711213,10.47170896242,1.89240417822602));
#37508=CARTESIAN_POINT('Ctrl Pts',(-5.84432042005851,10.3325278530965,1.66670829119904));
#37509=CARTESIAN_POINT('Ctrl Pts',(5.72538510600853,10.0514967496063,1.59489562708686));
#37510=CARTESIAN_POINT('Ctrl Pts',(5.27689078630208,10.1880792428534,1.81386477497724));
#37511=CARTESIAN_POINT('Ctrl Pts',(4.26533502063675,10.4437816859558,2.2441276685875));
#37512=CARTESIAN_POINT('Ctrl Pts',(2.63420875168904,10.7005792227098,2.71656172834629));
#37513=CARTESIAN_POINT('Ctrl Pts',(0.879504392503219,10.8292887596862,2.96954569268241));
#37514=CARTESIAN_POINT('Ctrl Pts',(-0.876488283445119,10.8293965289089,
2.96976264371174));
#37515=CARTESIAN_POINT('Ctrl Pts',(-2.63120592811252,10.700917777909,2.7172120634047));
#37516=CARTESIAN_POINT('Ctrl Pts',(-4.26346240346891,10.4442025274368,2.24486177732035));
#37517=CARTESIAN_POINT('Ctrl Pts',(-5.27604986041985,10.188339433728,1.81428014237951));
#37518=CARTESIAN_POINT('Ctrl Pts',(-5.72549894105245,10.0514621102988,1.59484001174331));
#37519=CARTESIAN_POINT('Ctrl Pts',(5.71943960541124,9.77839678543227,1.74872366789884));
#37520=CARTESIAN_POINT('Ctrl Pts',(5.27224638947531,9.91364416277643,1.9653747050709));
#37521=CARTESIAN_POINT('Ctrl Pts',(4.26336592362135,10.1670212916803,2.39142245426171));
#37522=CARTESIAN_POINT('Ctrl Pts',(2.63459204266588,10.4218933752604,2.86015313741059));
#37523=CARTESIAN_POINT('Ctrl Pts',(0.879984211070912,10.5498274753047,3.11161319304617));
#37524=CARTESIAN_POINT('Ctrl Pts',(-0.876966788137325,10.5499346576453,
3.11182899606998));
#37525=CARTESIAN_POINT('Ctrl Pts',(-2.63159126948949,10.4222297095009,2.86079911077524));
#37526=CARTESIAN_POINT('Ctrl Pts',(-4.26149794683647,10.1674385327164,2.39214984759134));
#37527=CARTESIAN_POINT('Ctrl Pts',(-5.27140792789829,9.91390180831679,1.96578563564803));
#37528=CARTESIAN_POINT('Ctrl Pts',(-5.71955311537339,9.77836248755778,1.74866863471185));
#37529=CARTESIAN_POINT('Ctrl Pts',(5.83022484041109,9.69039160441613,2.02848103772045));
#37530=CARTESIAN_POINT('Ctrl Pts',(5.3755767692724,9.82613351137638,2.24824169564194));
#37531=CARTESIAN_POINT('Ctrl Pts',(4.34950254584683,10.0805769763631,2.68067956629756));
#37532=CARTESIAN_POINT('Ctrl Pts',(2.69013112778482,10.3369366903571,3.15747035215418));
#37533=CARTESIAN_POINT('Ctrl Pts',(0.899042785899667,10.4658275761937,3.41382980296367));
#37534=CARTESIAN_POINT('Ctrl Pts',(-0.895960490475546,10.4659356306253,
3.41405001720562));
#37535=CARTESIAN_POINT('Ctrl Pts',(-2.68707068653567,10.3372753366022,3.15812834094409));
#37536=CARTESIAN_POINT('Ctrl Pts',(-4.3476022823214,10.0809961755248,2.68141832841113));
#37537=CARTESIAN_POINT('Ctrl Pts',(-5.37472436608816,9.82639210091812,2.24865847853217));
#37538=CARTESIAN_POINT('Ctrl Pts',(-5.83034025009099,9.6903571840313,2.02842520243865));
#37539=CARTESIAN_POINT('',(-5.72001816061901,9.72697624291305,2.05943242314956));
#37540=CARTESIAN_POINT('Origin',(-5.89877612790054,10.1838113533859,2.15616400895824));
#37541=CARTESIAN_POINT('Ctrl Pts',(5.72001490840061,9.72697523518687,2.05943402421887));
#37542=CARTESIAN_POINT('Ctrl Pts',(5.51235198943714,9.78739731182845,2.15782078059172));
#37543=CARTESIAN_POINT('Ctrl Pts',(5.29964847952653,9.84440335009143,2.25259520759938));
#37544=CARTESIAN_POINT('Ctrl Pts',(5.08198158984127,9.8979028691542,2.34311806232899));
#37545=CARTESIAN_POINT('Ctrl Pts',(4.87630120287531,9.94845627118625,2.42865599516285));
#37546=CARTESIAN_POINT('Ctrl Pts',(4.66618904522251,9.99587865664118,2.51039747519363));
#37547=CARTESIAN_POINT('Ctrl Pts',(4.45173460952731,10.0400902988936,2.58775796338993));
#37548=CARTESIAN_POINT('Ctrl Pts',(4.43923677872028,10.0426668351297,2.5922663256884));
#37549=CARTESIAN_POINT('Ctrl Pts',(4.42672420769387,10.0452324660357,2.59675979619238));
#37550=CARTESIAN_POINT('Ctrl Pts',(4.41419691688718,10.0477871755214,2.60123825439549));
#37551=CARTESIAN_POINT('Ctrl Pts',(4.40407569623453,10.0498512114576,2.6048565517877));
#37552=CARTESIAN_POINT('Ctrl Pts',(4.39394486714726,10.0519081183605,2.60846504978682));
#37553=CARTESIAN_POINT('Ctrl Pts',(4.38380444711611,10.0539578885756,2.61206368468342));
#37554=CARTESIAN_POINT('Ctrl Pts',(4.17192365805595,10.0967871726915,2.68725599418255));
#37555=CARTESIAN_POINT('Ctrl Pts',(3.95585617378088,10.1364960011834,2.75816495889607));
#37556=CARTESIAN_POINT('Ctrl Pts',(3.73575047118406,10.1729824351331,2.82430882007291));
#37557=CARTESIAN_POINT('Ctrl Pts',(3.71382288922425,10.1766173217417,2.83089826741563));
#37558=CARTESIAN_POINT('Ctrl Pts',(3.69185523817543,10.1802202209102,2.8374403809089));
#37559=CARTESIAN_POINT('Ctrl Pts',(3.66984767104303,10.1837910278748,2.84393465629152));
#37560=CARTESIAN_POINT('Ctrl Pts',(3.54838959673465,10.2034980375156,2.87977606380628));
#37561=CARTESIAN_POINT('Ctrl Pts',(3.42571635010909,10.2222269093428,2.91416268775258));
#37562=CARTESIAN_POINT('Ctrl Pts',(3.30185884873608,10.2399551345675,2.94701908582717));
#37563=CARTESIAN_POINT('Ctrl Pts',(3.23993009804958,10.2488192471798,2.96344728486447));
#37564=CARTESIAN_POINT('Ctrl Pts',(3.17770527845606,10.2574331732445,2.97949292001389));
#37565=CARTESIAN_POINT('Ctrl Pts',(3.11518875344279,10.2657937072243,2.99514699337891));
#37566=CARTESIAN_POINT('Ctrl Pts',(3.08393049093615,10.2699739742143,3.00297403006142));
#37567=CARTESIAN_POINT('Ctrl Pts',(3.05259930187275,10.2740908918314,3.01070317587191));
#37568=CARTESIAN_POINT('Ctrl Pts',(3.02119574738027,10.2781440430835,3.01833332061816));
#37569=CARTESIAN_POINT('Ctrl Pts',(2.99854982368428,10.2810668763571,3.02383561736467));
#37570=CARTESIAN_POINT('Ctrl Pts',(2.9748857110574,10.2840806737505,3.02952098717871));
#37571=CARTESIAN_POINT('Ctrl Pts',(2.9523245541333,10.2869160467782,3.0348804082814));
#37572=CARTESIAN_POINT('Ctrl Pts',(2.94359970433979,10.2880125421334,3.0369530034173));
#37573=CARTESIAN_POINT('Ctrl Pts',(2.93503996082666,10.2890826369461,3.03897732516861));
#37574=CARTESIAN_POINT('Ctrl Pts',(2.92676855739885,10.2901117713241,3.04092564871964));
#37575=CARTESIAN_POINT('Ctrl Pts',(2.83652357254174,10.3013401217689,3.06218279460714));
#37576=CARTESIAN_POINT('Ctrl Pts',(2.74597262321716,10.3120229794392,3.08250464961453));
#37577=CARTESIAN_POINT('Ctrl Pts',(2.65513062758051,10.3221651214447,3.10187144875567));
#37578=CARTESIAN_POINT('Ctrl Pts',(2.39635416121228,10.3510564690113,3.15704055651781));
#37579=CARTESIAN_POINT('Ctrl Pts',(2.13521677961336,10.3755617409481,3.20446287311253));
#37580=CARTESIAN_POINT('Ctrl Pts',(1.87219104066715,10.3957416660273,3.24382759350234));
#37581=CARTESIAN_POINT('Ctrl Pts',(1.61422025029409,10.4155337641057,3.28243578474802));
#37582=CARTESIAN_POINT('Ctrl Pts',(1.35443247684423,10.4311650650209,3.31329332864275));
#37583=CARTESIAN_POINT('Ctrl Pts',(1.09326623534793,10.4426713053128,3.33606238398908));
#37584=CARTESIAN_POINT('Ctrl Pts',(1.02414978900039,10.445716378961,3.3420881099145));
#37585=CARTESIAN_POINT('Ctrl Pts',(0.954936781483695,10.4484724306796,3.34754708449844));
#37586=CARTESIAN_POINT('Ctrl Pts',(0.885635322910046,10.4509398774855,3.35243247792281));
#37587=CARTESIAN_POINT('Ctrl Pts',(0.622150988790217,10.4603211169571,3.37100675701921));
#37588=CARTESIAN_POINT('Ctrl Pts',(0.357387451141609,10.4655323006477,3.38129329316036));
#37589=CARTESIAN_POINT('Ctrl Pts',(0.0918656894087061,10.4665095187268,
3.3832237866013));
#37590=CARTESIAN_POINT('Ctrl Pts',(0.0612581983271671,10.4666221655903,
3.38344632037929));
#37591=CARTESIAN_POINT('Ctrl Pts',(0.0306406423813369,10.4666785268953,
3.38355777001305));
#37592=CARTESIAN_POINT('Ctrl Pts',(1.38288139147356E-5,10.4666784850131,
3.38355799146479));
#37593=CARTESIAN_POINT('Ctrl Pts',(-0.260471068774009,10.4666781287992,
3.38355987493963));
#37594=CARTESIAN_POINT('Ctrl Pts',(-0.520268343612212,10.4625922845768,
3.37554239434947));
#37595=CARTESIAN_POINT('Ctrl Pts',(-0.778903582148321,10.4544897161825,
3.35956035939152));
#37596=CARTESIAN_POINT('Ctrl Pts',(-0.813491042715138,10.4534061543816,
3.35742307134441));
#37597=CARTESIAN_POINT('Ctrl Pts',(-0.848057728692277,10.4522507238744,
3.35514327831035));
#37598=CARTESIAN_POINT('Ctrl Pts',(-0.882602510186255,10.4510235576393,
3.35272104898075));
#37599=CARTESIAN_POINT('Ctrl Pts',(-1.08260237594735,10.4439187773607,3.33869735220771));
#37600=CARTESIAN_POINT('Ctrl Pts',(-1.28186813818427,10.4344100971061,3.31990076044197));
#37601=CARTESIAN_POINT('Ctrl Pts',(-1.48021120198736,10.4224869677621,3.29648136837608));
#37602=CARTESIAN_POINT('Ctrl Pts',(-1.72460014088733,10.4077958519104,3.2676251015275));
#37603=CARTESIAN_POINT('Ctrl Pts',(-1.96757580743929,10.3894539541556,3.2317098037961));
#37604=CARTESIAN_POINT('Ctrl Pts',(-2.20877711737513,10.3674169612257,3.18901198452615));
#37605=CARTESIAN_POINT('Ctrl Pts',(-2.32937777234304,10.3563984647607,3.16766307489118));
#37606=CARTESIAN_POINT('Ctrl Pts',(-2.44953515283027,10.3444552399712,3.14461997457069));
#37607=CARTESIAN_POINT('Ctrl Pts',(-2.56920598353283,10.331576080652,3.11992579982614));
#37608=CARTESIAN_POINT('Ctrl Pts',(-2.59686203949018,10.3285996932673,3.11421894983984));
#37609=CARTESIAN_POINT('Ctrl Pts',(-2.62449215450421,10.3255732879286,3.10842397436765));
#37610=CARTESIAN_POINT('Ctrl Pts',(-2.65209572000823,10.322496739247,3.10254136005408));
#37611=CARTESIAN_POINT('Ctrl Pts',(-2.68421400384005,10.318917003732,3.09569661109696));
#37612=CARTESIAN_POINT('Ctrl Pts',(-2.7162963432974,10.3152693811637,3.08873321145855));
#37613=CARTESIAN_POINT('Ctrl Pts',(-2.74834204355002,10.3115536050379,3.08165225587728));
#37614=CARTESIAN_POINT('Ctrl Pts',(-2.77813548600742,10.308098983628,3.07506896885309));
#37615=CARTESIAN_POINT('Ctrl Pts',(-2.80789721199739,10.3045854773189,3.06838401271604));
#37616=CARTESIAN_POINT('Ctrl Pts',(-2.83762657928914,10.3010129105985,3.06159817626225));
#37617=CARTESIAN_POINT('Ctrl Pts',(-2.85923495052844,10.2984162408741,3.05666598676008));
#37618=CARTESIAN_POINT('Ctrl Pts',(-2.87983096400873,10.2959101762994,3.05191147348056));
#37619=CARTESIAN_POINT('Ctrl Pts',(-2.90158490594942,10.2932296975479,3.0468324070001));
#37620=CARTESIAN_POINT('Ctrl Pts',(-2.90976061131236,10.2922223029081,3.04492355980467));
#37621=CARTESIAN_POINT('Ctrl Pts',(-2.91809973466331,10.2911900242974,3.04296845002873));
#37622=CARTESIAN_POINT('Ctrl Pts',(-2.92671696595623,10.2901178465306,3.04093882497416));
#37623=CARTESIAN_POINT('Ctrl Pts',(-3.15178238735407,10.2621146361379,2.98792894248901));
#37624=CARTESIAN_POINT('Ctrl Pts',(-3.37318101670882,10.2308852311845,2.92969863789928));
#37625=CARTESIAN_POINT('Ctrl Pts',(-3.59074180566845,10.1965240090342,2.86679780973399));
#37626=CARTESIAN_POINT('Ctrl Pts',(-3.81369841711418,10.1613105788366,2.80233694998106));
#37627=CARTESIAN_POINT('Ctrl Pts',(-4.03262451490004,10.1228081162286,2.73297091727145));
#37628=CARTESIAN_POINT('Ctrl Pts',(-4.24735524579871,10.0811143954969,2.65924060733081));
#37629=CARTESIAN_POINT('Ctrl Pts',(-4.30221094336249,10.0704632040015,2.64040526147015));
#37630=CARTESIAN_POINT('Ctrl Pts',(-4.35679293942059,10.0596037257926,2.62128484889262));
#37631=CARTESIAN_POINT('Ctrl Pts',(-4.41109867300135,10.0485375457635,2.60188788503165));
#37632=CARTESIAN_POINT('Ctrl Pts',(-4.63913382081059,10.0020695610366,2.52043811482444));
#37633=CARTESIAN_POINT('Ctrl Pts',(-4.86229671262369,9.95195749262712,2.434116675331));
#37634=CARTESIAN_POINT('Ctrl Pts',(-5.0804825496319,9.89832400754834,2.34351848583091));
#37635=CARTESIAN_POINT('Ctrl Pts',(-5.2986683866401,9.84469052246957,2.25292029633083));
#37636=CARTESIAN_POINT('Ctrl Pts',(-5.51187730087082,9.78753563449656,2.15804500081236));
#37637=CARTESIAN_POINT('Ctrl Pts',(-5.72001753333531,9.72697463976802,2.05943208370059));
#37638=CARTESIAN_POINT('Ctrl Pts',(-5.71201821360281,10.3745893795876,1.73089321988294));
#37639=CARTESIAN_POINT('Ctrl Pts',(-5.71753470941925,10.3728819373349,1.7286358487777));
#37640=CARTESIAN_POINT('Ctrl Pts',(-5.76529494709306,10.3582189611947,1.70809774779482));
#37641=CARTESIAN_POINT('Ctrl Pts',(-5.85055921091664,10.3340058651975,1.65506459479143));
#37642=CARTESIAN_POINT('Ctrl Pts',(-5.94855788476008,10.3111442455001,1.55167544971277));
#37643=CARTESIAN_POINT('Ctrl Pts',(-6.01625188434961,10.3010076858463,1.43149053235932));
#37644=CARTESIAN_POINT('Ctrl Pts',(-6.04732974734974,10.3030375271302,1.31928535914519));
#37645=CARTESIAN_POINT('Ctrl Pts',(-6.05141080953246,10.3096109683119,1.25173107752086));
#37646=CARTESIAN_POINT('Ctrl Pts',(-6.05071568539176,10.3130319392939,1.22538737377867));
#37647=CARTESIAN_POINT('Ctrl Pts',(-5.59596286913054,10.091024988519,1.65481426090108));
#37648=CARTESIAN_POINT('Ctrl Pts',(-5.60111045497149,10.0894199224357,1.65273810722318));
#37649=CARTESIAN_POINT('Ctrl Pts',(-5.64568435427929,10.0756272036296,1.63384806964916));
#37650=CARTESIAN_POINT('Ctrl Pts',(-5.72536755241762,10.0527126854641,1.5850500029164));
#37651=CARTESIAN_POINT('Ctrl Pts',(-5.81695324569551,10.0308278463846,1.48997227540393));
#37652=CARTESIAN_POINT('Ctrl Pts',(-5.88006365701701,10.020853739627,1.37978256343051));
#37653=CARTESIAN_POINT('Ctrl Pts',(-5.90886973469154,10.0223543906179,1.27753231866074));
#37654=CARTESIAN_POINT('Ctrl Pts',(-5.91261218350735,10.0282473351447,1.21648882520907));
#37655=CARTESIAN_POINT('Ctrl Pts',(-5.9119739864041,10.0313348077132,1.19278337685752));
#37656=CARTESIAN_POINT('Ctrl Pts',(-5.5788598499786,9.8189785998903,1.81407643830995));
#37657=CARTESIAN_POINT('Ctrl Pts',(-5.58617900390802,9.81673898600098,1.8111487551284));
#37658=CARTESIAN_POINT('Ctrl Pts',(-5.64948915158139,9.79753620524486,1.78454467298062));
#37659=CARTESIAN_POINT('Ctrl Pts',(-5.76170664028583,9.76626533716724,1.71642469728939));
#37660=CARTESIAN_POINT('Ctrl Pts',(-5.89067180786221,9.73709385598877,1.58418520698851));
#37661=CARTESIAN_POINT('Ctrl Pts',(-5.98091235554539,9.72423239118939,1.42907135224037));
#37662=CARTESIAN_POINT('Ctrl Pts',(-6.02360066369486,9.72705369891453,1.28087941931778));
#37663=CARTESIAN_POINT('Ctrl Pts',(-6.02950933576142,9.73602295206567,1.18866363771198));
#37664=CARTESIAN_POINT('Ctrl Pts',(-6.02850854633718,9.74076242253544,1.15211679278597));
#37665=CARTESIAN_POINT('Ctrl Pts',(-5.67191631397939,9.7367167713257,2.104318164895));
#37666=CARTESIAN_POINT('Ctrl Pts',(-5.68252452601478,9.73352149298544,2.100064196715));
#37667=CARTESIAN_POINT('Ctrl Pts',(-5.77421599484514,9.70617344358581,2.06143883184841));
#37668=CARTESIAN_POINT('Ctrl Pts',(-5.93576401678745,9.66236705788763,1.96310123941882));
#37669=CARTESIAN_POINT('Ctrl Pts',(-6.12140704144701,9.62242031220293,1.77257821790161));
#37670=CARTESIAN_POINT('Ctrl Pts',(-6.25271357804119,9.60551370991075,1.54705882731488));
#37671=CARTESIAN_POINT('Ctrl Pts',(-6.31634136597211,9.61064011934564,1.32713332299514));
#37672=CARTESIAN_POINT('Ctrl Pts',(-6.32550161226352,9.62442663858794,1.18648879700547));
#37673=CARTESIAN_POINT('Ctrl Pts',(-6.32395631113669,9.63172107981537,1.13003563160022));
#37674=CARTESIAN_POINT('',(-5.99998809173028,10.0933467245957,1.21103470346248));
#37675=CARTESIAN_POINT('',(-5.99999999616419,9.65438802498414,1.8624761678277));
#37676=CARTESIAN_POINT('Ctrl Pts',(-5.99998809173028,10.0933467245957,1.21103470346248));
#37677=CARTESIAN_POINT('Ctrl Pts',(-5.99998614033857,10.0742249652676,1.22561744409544));
#37678=CARTESIAN_POINT('Ctrl Pts',(-5.99998781129217,10.0554651409929,1.24052926194382));
#37679=CARTESIAN_POINT('Ctrl Pts',(-6.00000062824795,10.037183037652,1.25577699121628));
#37680=CARTESIAN_POINT('Ctrl Pts',(-6.00000707142198,10.0279924954203,1.26344213221258));
#37681=CARTESIAN_POINT('Ctrl Pts',(-6.0000156689702,10.0189226652474,1.27119157323869));
#37682=CARTESIAN_POINT('Ctrl Pts',(-6.00002447527685,10.0099875859112,1.27902227748033));
#37683=CARTESIAN_POINT('Ctrl Pts',(-6.0000429277041,9.99126533290177,1.29543046150826));
#37684=CARTESIAN_POINT('Ctrl Pts',(-6.0000639885918,9.97313591895691,1.31219831393756));
#37685=CARTESIAN_POINT('Ctrl Pts',(-6.0000852622,9.95570443374821,1.3292681789178));
#37686=CARTESIAN_POINT('Ctrl Pts',(-6.0000991408704,9.94433232255919,1.34040437300642));
#37687=CARTESIAN_POINT('Ctrl Pts',(-6.00011245325909,9.93325694654117,1.35166810031643));
#37688=CARTESIAN_POINT('Ctrl Pts',(-6.00012171175544,9.92250192113295,1.3630332377823));
#37689=CARTESIAN_POINT('Ctrl Pts',(-6.0001362455576,9.90561889763326,1.38087400297164));
#37690=CARTESIAN_POINT('Ctrl Pts',(-6.00013967180241,9.8895273924494,1.39896623194891));
#37691=CARTESIAN_POINT('Ctrl Pts',(-6.0001239623281,9.8742900370339,1.41717677920137));
#37692=CARTESIAN_POINT('Ctrl Pts',(-6.00011958298751,9.87004230934187,1.42225334555701));
#37693=CARTESIAN_POINT('Ctrl Pts',(-6.00011380591212,9.86586073279952,1.42733890963523));
#37694=CARTESIAN_POINT('Ctrl Pts',(-6.0001067056879,9.86174612648125,1.43243017907439));
#37695=CARTESIAN_POINT('Ctrl Pts',(-6.00010098822784,9.85843283713094,1.4365299270229));
#37696=CARTESIAN_POINT('Ctrl Pts',(-6.00009441688859,9.85516296794322,1.44063337206656));
#37697=CARTESIAN_POINT('Ctrl Pts',(-6.00008719772681,9.85193679562792,1.44473884265702));
#37698=CARTESIAN_POINT('Ctrl Pts',(-6.00006865390159,9.84364974272975,1.45528454469337));
#37699=CARTESIAN_POINT('Ctrl Pts',(-6.00005102576008,9.83553345028822,1.46598520939338));
#37700=CARTESIAN_POINT('Ctrl Pts',(-6.00003057015005,9.82773268116427,1.47665723439913));
#37701=CARTESIAN_POINT('Ctrl Pts',(-6.00000992968066,9.81986141572172,1.48742570354556));
#37702=CARTESIAN_POINT('Ctrl Pts',(-5.99998595813747,9.81231176741329,1.49816463309059));
#37703=CARTESIAN_POINT('Ctrl Pts',(-5.99996791547376,9.80519759071623,1.50864643475104));
#37704=CARTESIAN_POINT('Ctrl Pts',(-5.99995722328368,9.80098168719531,1.51485801290091));
#37705=CARTESIAN_POINT('Ctrl Pts',(-5.99994890968004,9.79691800437195,1.52097856799308));
#37706=CARTESIAN_POINT('Ctrl Pts',(-5.99994782973511,9.7930240862629,1.5269554953353));
#37707=CARTESIAN_POINT('Ctrl Pts',(-5.99994380484361,9.77851168159836,1.54923115337734));
#37708=CARTESIAN_POINT('Ctrl Pts',(-5.99996594985734,9.76478866904984,1.57206820321156));
#37709=CARTESIAN_POINT('Ctrl Pts',(-5.9999936985603,9.75201300643072,1.59536297341009));
#37710=CARTESIAN_POINT('Ctrl Pts',(-6.00002003739057,9.73988645731992,1.61747416899025));
#37711=CARTESIAN_POINT('Ctrl Pts',(-6.00005067895151,9.72861404445652,1.63999684562807));
#37712=CARTESIAN_POINT('Ctrl Pts',(-6.00007008721526,9.71830125813383,1.66279885804127));
#37713=CARTESIAN_POINT('Ctrl Pts',(-6.00007112610654,9.71774923225662,1.66401941090746));
#37714=CARTESIAN_POINT('Ctrl Pts',(-6.00007213476147,9.7171999474611,1.66524075529511));
#37715=CARTESIAN_POINT('Ctrl Pts',(-6.00007311154295,9.7166534169473,1.66646286803396));
#37716=CARTESIAN_POINT('Ctrl Pts',(-6.00009137615566,9.70643396830422,1.68931487364968));
#37717=CARTESIAN_POINT('Ctrl Pts',(-6.0000974466336,9.6971810033845,1.71243799002433));
#37718=CARTESIAN_POINT('Ctrl Pts',(-6.0000894323575,9.68895805489599,1.73566955548174));
#37719=CARTESIAN_POINT('Ctrl Pts',(-6.00008131870306,9.68063314048201,1.75918919620504));
#37720=CARTESIAN_POINT('Ctrl Pts',(-6.00005836465151,9.67336426344868,1.78281898369511));
#37721=CARTESIAN_POINT('Ctrl Pts',(-6.00003565609075,9.66717105559036,1.80636853253183));
#37722=CARTESIAN_POINT('Ctrl Pts',(-6.00001753957099,9.66223021527243,1.82515597888002));
#37723=CARTESIAN_POINT('Ctrl Pts',(-5.99999991840194,9.65797302840061,1.84389173683365));
#37724=CARTESIAN_POINT('Ctrl Pts',(-5.99999992132011,9.65438781893335,1.86247612807742));
#37725=CARTESIAN_POINT('Ctrl Pts',(-5.72001867922509,9.72697756830105,2.05943270378453));
#37726=CARTESIAN_POINT('Ctrl Pts',(-5.77263456937867,9.71166938421254,2.03449628829274));
#37727=CARTESIAN_POINT('Ctrl Pts',(-5.82217073193389,9.69806595346106,2.00534896070888));
#37728=CARTESIAN_POINT('Ctrl Pts',(-5.86880003058777,9.68600232454907,1.97245371766885));
#37729=CARTESIAN_POINT('Ctrl Pts',(-5.91542932735784,9.67393869612445,1.93955847595777));
#37730=CARTESIAN_POINT('Ctrl Pts',(-5.95915199503842,9.66341542696136,1.90291542432145));
#37731=CARTESIAN_POINT('Ctrl Pts',(-6.00000008250642,9.65438822329311,1.86247621077463));
#37732=CARTESIAN_POINT('Ctrl Pts',(-5.73278520175299,10.3449555119164,1.71288400365943));
#37733=CARTESIAN_POINT('Ctrl Pts',(-5.74762625823566,10.3336655306276,1.70321684759683));
#37734=CARTESIAN_POINT('Ctrl Pts',(-5.76162670497642,10.3229263377101,1.69298708845874));
#37735=CARTESIAN_POINT('Ctrl Pts',(-5.77478485377481,10.3127313231399,1.68242386558445));
#37736=CARTESIAN_POINT('Ctrl Pts',(-5.78881554118989,10.3018602602861,1.67116017792474));
#37737=CARTESIAN_POINT('Ctrl Pts',(-5.80188866776032,10.2916079863685,1.65951704513893));
#37738=CARTESIAN_POINT('Ctrl Pts',(-5.81403019712682,10.2819593872248,1.64772073960543));
#37739=CARTESIAN_POINT('Ctrl Pts',(-5.81727069665296,10.2793842354454,1.64457237819743));
#37740=CARTESIAN_POINT('Ctrl Pts',(-5.82044497488178,10.2768520458908,1.64141285163079));
#37741=CARTESIAN_POINT('Ctrl Pts',(-5.8235538117211,10.2743624479256,1.63824593592917));
#37742=CARTESIAN_POINT('Ctrl Pts',(-5.83603217451932,10.2643696087266,1.62553445407319));
#37743=CARTESIAN_POINT('Ctrl Pts',(-5.84745523384838,10.2550631298136,1.61270887825643));
#37744=CARTESIAN_POINT('Ctrl Pts',(-5.85790547528079,10.2464057644275,1.60000846413517));
#37745=CARTESIAN_POINT('Ctrl Pts',(-5.8687730380341,10.2374026746692,1.5868008699998));
#37746=CARTESIAN_POINT('Ctrl Pts',(-5.8785888944447,10.2291015910019,1.57372786952288));
#37747=CARTESIAN_POINT('Ctrl Pts',(-5.88745826772452,10.2214578451449,1.56099705001076));
#37748=CARTESIAN_POINT('Ctrl Pts',(-5.89162954745436,10.2178629798543,1.55500972625071));
#37749=CARTESIAN_POINT('Ctrl Pts',(-5.89559162955099,10.2144134683544,1.54909729291484));
#37750=CARTESIAN_POINT('Ctrl Pts',(-5.89935609598258,10.2111044910471,1.54327753594125));
#37751=CARTESIAN_POINT('Ctrl Pts',(-5.90168366366344,10.2090585520603,1.53967918316314));
#37752=CARTESIAN_POINT('Ctrl Pts',(-5.90393569087849,10.207066336566,1.53611621550207));
#37753=CARTESIAN_POINT('Ctrl Pts',(-5.90611496859368,10.2051266893969,1.53259243533064));
#37754=CARTESIAN_POINT('Ctrl Pts',(-5.90944521028314,10.2021626367566,1.52720760550852));
#37755=CARTESIAN_POINT('Ctrl Pts',(-5.91260559262295,10.1993213304078,1.52191438606531));
#37756=CARTESIAN_POINT('Ctrl Pts',(-5.91560707709282,10.1965982311228,1.5167261658696));
#37757=CARTESIAN_POINT('Ctrl Pts',(-5.91808989042462,10.1943456966597,1.51243449539801));
#37758=CARTESIAN_POINT('Ctrl Pts',(-5.92046390928247,10.1921740784455,1.50821473564372));
#37759=CARTESIAN_POINT('Ctrl Pts',(-5.92273528386489,10.1900808352025,1.50407344253474));
#37760=CARTESIAN_POINT('Ctrl Pts',(-5.9238709711561,10.189034213581,1.50200279598024));
#37761=CARTESIAN_POINT('Ctrl Pts',(-5.92498099014943,10.1880071875312,1.4999517613849));
#37762=CARTESIAN_POINT('Ctrl Pts',(-5.9260660878658,10.1869994516525,1.49792110336238));
#37763=CARTESIAN_POINT('Ctrl Pts',(-5.92682745232362,10.1862923685305,1.49649628159654));
#37764=CARTESIAN_POINT('Ctrl Pts',(-5.92726381086926,10.1858856593911,1.4956732784651));
#37765=CARTESIAN_POINT('Ctrl Pts',(-5.92803487321876,10.1851664614614,1.49420743045771));
#37766=CARTESIAN_POINT('Ctrl Pts',(-5.92836273003475,10.1848606574711,1.49358414978433));
#37767=CARTESIAN_POINT('Ctrl Pts',(-5.92875078441314,10.1844984854958,1.49284443006148));
#37768=CARTESIAN_POINT('Ctrl Pts',(-5.92924734435405,10.184033813251,1.49189099663322));
#37769=CARTESIAN_POINT('Ctrl Pts',(-5.93919300113636,10.1747268388407,1.47279456766051));
#37770=CARTESIAN_POINT('Ctrl Pts',(-5.94793107627244,10.1661803928757,1.45367212129977));
#37771=CARTESIAN_POINT('Ctrl Pts',(-5.95553872313124,10.1583598358875,1.4347373834926));
#37772=CARTESIAN_POINT('Ctrl Pts',(-5.9586318177942,10.1551801768509,1.42703895353879));
#37773=CARTESIAN_POINT('Ctrl Pts',(-5.96153809959893,10.1521204767886,1.41937092680088));
#37774=CARTESIAN_POINT('Ctrl Pts',(-5.9642630307132,10.1491782414327,1.4117452974802));
#37775=CARTESIAN_POINT('Ctrl Pts',(-5.9710901981722,10.1418066299549,1.39263969584501));
#37776=CARTESIAN_POINT('Ctrl Pts',(-5.97677989684862,10.135172123484,1.37380405250111));
#37777=CARTESIAN_POINT('Ctrl Pts',(-5.98146315896994,10.1292176627262,1.35542195960802));
#37778=CARTESIAN_POINT('Ctrl Pts',(-5.98644690166057,10.1228811606237,1.33586046193365));
#37779=CARTESIAN_POINT('Ctrl Pts',(-5.99029046394656,10.1173148938422,1.31681231134461));
#37780=CARTESIAN_POINT('Ctrl Pts',(-5.99314482070217,10.1124514917611,1.29844067055225));
#37781=CARTESIAN_POINT('Ctrl Pts',(-5.99383961718569,10.1112676612335,1.29396871679453));
#37782=CARTESIAN_POINT('Ctrl Pts',(-5.99447578939983,10.1101254778785,1.28953660287938));
#37783=CARTESIAN_POINT('Ctrl Pts',(-5.99505550273689,10.1090239704676,1.28514623077354));
#37784=CARTESIAN_POINT('Ctrl Pts',(-5.99754124290847,10.10430084087,1.2663208499966));
#37785=CARTESIAN_POINT('Ctrl Pts',(-5.99899094609771,10.1003248617228,1.24826680445821));
#37786=CARTESIAN_POINT('Ctrl Pts',(-5.99961818135814,10.0970053748056,1.23110680412698));
#37787=CARTESIAN_POINT('Ctrl Pts',(-5.99986797371164,10.0956834107806,1.22427294586166));
#37788=CARTESIAN_POINT('Ctrl Pts',(-5.99998707059434,10.0944656568097,1.21758034077405));
#37789=CARTESIAN_POINT('Ctrl Pts',(-5.99998809173028,10.0933467245957,1.21103470346248));
#37790=CARTESIAN_POINT('Ctrl Pts',(-5.72202398775916,19.8960805169565,0.386352176427263));
#37791=CARTESIAN_POINT('Ctrl Pts',(-5.722744923188,19.5069870025453,0.666957542712061));
#37792=CARTESIAN_POINT('Ctrl Pts',(-5.72404047055462,18.65358895384,1.1961917425212));
#37793=CARTESIAN_POINT('Ctrl Pts',(-5.72530463330588,17.252880723512,1.80439897490435));
#37794=CARTESIAN_POINT('Ctrl Pts',(-5.72546454574842,15.7365645039447,2.20426079914038));
#37795=CARTESIAN_POINT('Ctrl Pts',(-5.72471278438522,14.1774183292184,2.3706007618924));
#37796=CARTESIAN_POINT('Ctrl Pts',(-5.72306497930087,12.6107761111604,2.29992939792902));
#37797=CARTESIAN_POINT('Ctrl Pts',(-5.72038826693908,11.1578231494624,2.009761590955));
#37798=CARTESIAN_POINT('Ctrl Pts',(-5.71829665675548,10.2528020998913,1.69379809858199));
#37799=CARTESIAN_POINT('Ctrl Pts',(-5.71724106961605,9.85241023628882,1.52490686972533));
#37800=CARTESIAN_POINT('Ctrl Pts',(-5.90002815788726,19.8627034270208,0.340121769673507));
#37801=CARTESIAN_POINT('Ctrl Pts',(-5.90064112502721,19.4755717271918,0.618895098936227));
#37802=CARTESIAN_POINT('Ctrl Pts',(-5.90174136243637,18.6265869130023,1.14467025662982));
#37803=CARTESIAN_POINT('Ctrl Pts',(-5.90281091502772,17.233624563546,1.74886350102612));
#37804=CARTESIAN_POINT('Ctrl Pts',(-5.90294617326952,15.7258951691654,2.14638243188552));
#37805=CARTESIAN_POINT('Ctrl Pts',(-5.90231020081427,14.1756917163178,2.31212465550085));
#37806=CARTESIAN_POINT('Ctrl Pts',(-5.90091450222212,12.6178122340193,2.24263139230537));
#37807=CARTESIAN_POINT('Ctrl Pts',(-5.89863680636618,11.1726809459824,1.9553149115722));
#37808=CARTESIAN_POINT('Ctrl Pts',(-5.89685246807884,10.2721886785122,1.64197819775049));
#37809=CARTESIAN_POINT('Ctrl Pts',(-5.89594599918652,9.87374136647885,1.47444506422475));
#37810=CARTESIAN_POINT('Ctrl Pts',(-6.00728101833992,19.7730197694138,0.215901419477209));
#37811=CARTESIAN_POINT('Ctrl Pts',(-6.00760398018924,19.3915708450173,0.490321734932853));
#37812=CARTESIAN_POINT('Ctrl Pts',(-6.00818204236773,18.5550176863609,1.00794402616504));
#37813=CARTESIAN_POINT('Ctrl Pts',(-6.00873885820584,17.1829706228646,1.6026646162929));
#37814=CARTESIAN_POINT('Ctrl Pts',(-6.00880922773446,15.6978212924223,1.99418148817968));
#37815=CARTESIAN_POINT('Ctrl Pts',(-6.00847821278282,14.1710746182912,2.15763405987662));
#37816=CARTESIAN_POINT('Ctrl Pts',(-6.00774960894449,12.6364830352444,2.0896700063425));
#37817=CARTESIAN_POINT('Ctrl Pts',(-6.00654717924463,11.2128937590667,1.80743882631002));
#37818=CARTESIAN_POINT('Ctrl Pts',(-6.00559946168958,10.3255097743763,1.49932376623001));
#37819=CARTESIAN_POINT('Ctrl Pts',(-6.00511047283608,9.93286787454664,1.33457276173998));
#37820=CARTESIAN_POINT('Ctrl Pts',(-5.99966790103542,19.6635731258448,0.0643074436082086));
#37821=CARTESIAN_POINT('Ctrl Pts',(-5.99963698975156,19.2892128226794,0.333628132544527));
#37822=CARTESIAN_POINT('Ctrl Pts',(-5.99957878613466,18.4680448255696,0.841727065914757));
#37823=CARTESIAN_POINT('Ctrl Pts',(-5.99951367581519,17.1215601727196,1.42537763535855));
#37824=CARTESIAN_POINT('Ctrl Pts',(-5.99950536396078,15.66378285343,1.80967927954129));
#37825=CARTESIAN_POINT('Ctrl Pts',(-5.99954420660795,14.1654483981742,1.97008249641598));
#37826=CARTESIAN_POINT('Ctrl Pts',(-5.99962585188073,12.6591804244486,1.90337383375695));
#37827=CARTESIAN_POINT('Ctrl Pts',(-5.99973680056724,11.2620763145782,1.62638694967239));
#37828=CARTESIAN_POINT('Ctrl Pts',(-5.99981416523958,10.3910398983604,1.32395870088371));
#37829=CARTESIAN_POINT('Ctrl Pts',(-5.99984092544071,10.0056993730018,1.16227925631749));
#37830=CARTESIAN_POINT('',(-5.99999988467789,19.5919337295688,0.13548398932811));
#37831=CARTESIAN_POINT('Origin',(-5.59998164335335,19.5919273324291,0.135474139597038));
#37832=CARTESIAN_POINT('Ctrl Pts',(-6.,19.5919320859607,0.135483413470245));
#37833=CARTESIAN_POINT('Ctrl Pts',(-6.,19.2032417293653,0.410171473275152));
#37834=CARTESIAN_POINT('Ctrl Pts',(-6.,18.7991432375947,0.654503356286178));
#37835=CARTESIAN_POINT('Ctrl Pts',(-6.,18.3770565530435,0.869913230869506));
#37836=CARTESIAN_POINT('Ctrl Pts',(-6.,17.9549695699687,1.08532325780287));
#37837=CARTESIAN_POINT('Ctrl Pts',(-6.,17.5148943686686,1.27181123539797));
#37838=CARTESIAN_POINT('Ctrl Pts',(-6.,17.0647735964723,1.42538956888279));
#37839=CARTESIAN_POINT('Ctrl Pts',(-6.,16.6146528242763,1.5789679023675));
#37840=CARTESIAN_POINT('Ctrl Pts',(-6.,16.1544864811841,1.69963659174199));
#37841=CARTESIAN_POINT('Ctrl Pts',(-6.,15.6870767766761,1.78685625005223));
#37842=CARTESIAN_POINT('Ctrl Pts',(-6.,15.2196670721679,1.87407590836254));
#37843=CARTESIAN_POINT('Ctrl Pts',(-6.,14.7450140062439,1.92784653560856));
#37844=CARTESIAN_POINT('Ctrl Pts',(-6.,14.2698875448941,1.94742220490056));
#37845=CARTESIAN_POINT('Ctrl Pts',(-6.,13.7947610835446,1.96699787419255));
#37846=CARTESIAN_POINT('Ctrl Pts',(-6.,13.3191612267692,1.95237858553056));
#37847=CARTESIAN_POINT('Ctrl Pts',(-6.,12.8461741667461,1.90343073178653));
#37848=CARTESIAN_POINT('Ctrl Pts',(-6.,12.3731871067227,1.85448287804245));
#37849=CARTESIAN_POINT('Ctrl Pts',(-6.,11.9028128434515,1.77120645921628));
#37850=CARTESIAN_POINT('Ctrl Pts',(-6.,11.4430952551193,1.65563717376403));
#37851=CARTESIAN_POINT('Ctrl Pts',(-6.,10.9833776667874,1.54006788831187));
#37852=CARTESIAN_POINT('Ctrl Pts',(-6.,10.5343167533944,1.39220573623369));
#37853=CARTESIAN_POINT('Ctrl Pts',(-6.,10.0933467247176,1.21103470471191));
#37854=CARTESIAN_POINT('Origin',(-5.599999999997,19.5919343769627,0.135488060674723));
#37855=CARTESIAN_POINT('Origin',(-5.6,19.5919343770088,0.135488060674804));
#37856=CARTESIAN_POINT('Ctrl Pts',(-6.05070961963225,10.3130249361011,-1.22535725240516));
#37857=CARTESIAN_POINT('Ctrl Pts',(-6.05140667375169,10.3096023136128,-1.25170873298356));
#37858=CARTESIAN_POINT('Ctrl Pts',(-6.04732759893246,10.3030271880175,-1.31927088995749));
#37859=CARTESIAN_POINT('Ctrl Pts',(-6.01624876430349,10.3009968959657,-1.43148297695375));
#37860=CARTESIAN_POINT('Ctrl Pts',(-5.94855854570417,10.3111324909314,-1.55166467988863));
#37861=CARTESIAN_POINT('Ctrl Pts',(-5.85056713415748,10.3339919100581,-1.65505066142282));
#37862=CARTESIAN_POINT('Ctrl Pts',(-5.76530747145516,10.3582031816919,-1.70808535345447));
#37863=CARTESIAN_POINT('Ctrl Pts',(-5.71754885550636,10.3728653836147,-1.72862512790978));
#37864=CARTESIAN_POINT('Ctrl Pts',(-5.7120304436856,10.3745733921892,-1.73088351326345));
#37865=CARTESIAN_POINT('Ctrl Pts',(-5.9119799714366,10.0313345995451,-1.19275674695457));
#37866=CARTESIAN_POINT('Ctrl Pts',(-5.91261995497024,10.0282455529599,-1.21646968247228));
#37867=CARTESIAN_POINT('Ctrl Pts',(-5.90887926223061,10.0223509287081,-1.27752158060179));
#37868=CARTESIAN_POINT('Ctrl Pts',(-5.8800717142639,10.0208498082042,-1.37978014786759));
#37869=CARTESIAN_POINT('Ctrl Pts',(-5.81696369720526,10.0308230995347,-1.48996890572508));
#37870=CARTESIAN_POINT('Ctrl Pts',(-5.72538322198305,10.0527061528258,-1.58504538083284));
#37871=CARTESIAN_POINT('Ctrl Pts',(-5.64570293957858,10.0756193202956,-1.63384573406177));
#37872=CARTESIAN_POINT('Ctrl Pts',(-5.60112974557925,10.0894115585813,-1.65273765411278));
#37873=CARTESIAN_POINT('Ctrl Pts',(-5.59598027839829,10.0910171857285,-1.65481477844338));
#37874=CARTESIAN_POINT('Ctrl Pts',(-6.0285097850003,9.74077481927242,-1.1520775934791));
#37875=CARTESIAN_POINT('Ctrl Pts',(-6.02951335972276,9.73603300079858,-1.18863580640333));
#37876=CARTESIAN_POINT('Ctrl Pts',(-6.0236073757172,9.72706141057504,-1.28086318017417));
#37877=CARTESIAN_POINT('Ctrl Pts',(-5.98091755192499,9.72423946816267,-1.42906490732787));
#37878=CARTESIAN_POINT('Ctrl Pts',(-5.89068175080473,9.73709969987668,-1.58417525760424));
#37879=CARTESIAN_POINT('Ctrl Pts',(-5.76172577093106,9.766268391079,-1.71641116692069));
#37880=CARTESIAN_POINT('Ctrl Pts',(-5.64951415628754,9.79753689869301,-1.78453321317423));
#37881=CARTESIAN_POINT('Ctrl Pts',(-5.586206150674,9.81673862473118,-1.81113948056136));
#37882=CARTESIAN_POINT('Ctrl Pts',(-5.57888445210631,9.81897897780365,-1.81406848190426));
#37883=CARTESIAN_POINT('Ctrl Pts',(-6.32394327601718,9.63173326085878,-1.12997458657446));
#37884=CARTESIAN_POINT('Ctrl Pts',(-6.32549286216374,9.62443529434766,-1.18644508677191));
#37885=CARTESIAN_POINT('Ctrl Pts',(-6.31633671118906,9.61064543956799,-1.32710607464008));
#37886=CARTESIAN_POINT('Ctrl Pts',(-6.25270734978457,9.6055181449323,-1.54704358343089));
#37887=CARTESIAN_POINT('Ctrl Pts',(-6.12140914137511,9.62242290629162,-1.77255538315458));
#37888=CARTESIAN_POINT('Ctrl Pts',(-5.93578135264523,9.66236535691839,-1.96307110762315));
#37889=CARTESIAN_POINT('Ctrl Pts',(-5.7742437071044,9.70616784886645,-2.0614104224421));
#37890=CARTESIAN_POINT('Ctrl Pts',(-5.68255656006243,9.73351397080183,-2.10003844602719));
#37891=CARTESIAN_POINT('Ctrl Pts',(-5.67194479924022,9.73671025575887,-2.10429427367507));
#37892=CARTESIAN_POINT('',(-5.7327877343283,10.3449530459579,-1.71289077335416));
#37893=CARTESIAN_POINT('',(-5.72001814737754,9.72697621226736,-2.05943242421435));
#37894=CARTESIAN_POINT('Origin',(-5.8987601709971,10.1837992950051,-2.15614229677139));
#37895=CARTESIAN_POINT('',(-5.9999999968135,9.65438801435697,-1.86247622312975));
#37896=CARTESIAN_POINT('Ctrl Pts',(-6.00000008328868,9.65438821225989,-1.86247626630162));
#37897=CARTESIAN_POINT('Ctrl Pts',(-5.95915137667818,9.66341555272123,-1.90291609182812));
#37898=CARTESIAN_POINT('Ctrl Pts',(-5.91542827656402,9.67393895342414,-1.9395593190579));
#37899=CARTESIAN_POINT('Ctrl Pts',(-5.86879893709647,9.6860026085962,-1.97245448346289));
#37900=CARTESIAN_POINT('Ctrl Pts',(-5.82216959562333,9.69806626428713,-2.00534964928275));
#37901=CARTESIAN_POINT('Ctrl Pts',(-5.77263377986791,9.71166961723077,-2.03449664691797));
#37902=CARTESIAN_POINT('Ctrl Pts',(-5.72001867761226,9.72697756737453,-2.0594327111465));
#37903=CARTESIAN_POINT('',(-5.99998808311063,10.09334672158,-1.2110347210661));
#37904=CARTESIAN_POINT('Ctrl Pts',(-5.99998808311063,10.09334672158,-1.2110347210661));
#37905=CARTESIAN_POINT('Ctrl Pts',(-5.99998579341327,10.0709268555555,-1.2281327269299));
#37906=CARTESIAN_POINT('Ctrl Pts',(-5.99998684305411,10.0492796321252,-1.24555661530825));
#37907=CARTESIAN_POINT('Ctrl Pts',(-5.99998299250915,10.0284346981922,-1.26332163857805));
#37908=CARTESIAN_POINT('Ctrl Pts',(-5.9999818636268,10.0223234910084,-1.26852989388725));
#37909=CARTESIAN_POINT('Ctrl Pts',(-5.99998012528455,10.0162810465041,-1.27376722624289));
#37910=CARTESIAN_POINT('Ctrl Pts',(-5.99997728635832,10.0103076348659,-1.27903349119982));
#37911=CARTESIAN_POINT('Ctrl Pts',(-5.99996366417836,9.98164507665961,-1.3043029075739));
#37912=CARTESIAN_POINT('Ctrl Pts',(-5.99992845500907,9.9545755699725,-1.33023848659307));
#37913=CARTESIAN_POINT('Ctrl Pts',(-5.99991579265607,9.92904827997819,-1.3568311348157));
#37914=CARTESIAN_POINT('Ctrl Pts',(-5.99991509569424,9.92764320568267,-1.35829484860889));
#37915=CARTESIAN_POINT('Ctrl Pts',(-5.99991446145114,9.92624279434832,-1.35976055702209));
#37916=CARTESIAN_POINT('Ctrl Pts',(-5.99991389619172,9.92484703487078,-1.36122826085182));
#37917=CARTESIAN_POINT('Ctrl Pts',(-5.99990496302787,9.90278893600095,-1.38442334332033));
#37918=CARTESIAN_POINT('Ctrl Pts',(-5.99990285601733,9.88191510379151,-1.40812762073311));
#37919=CARTESIAN_POINT('Ctrl Pts',(-5.9999038676287,9.86223177764951,-1.43232863089542));
#37920=CARTESIAN_POINT('Ctrl Pts',(-5.99990457803031,9.84840921017725,-1.44932373088269));
#37921=CARTESIAN_POINT('Ctrl Pts',(-5.99990726918065,9.83517314684603,-1.46656412244876));
#37922=CARTESIAN_POINT('Ctrl Pts',(-5.99991518239819,9.82252477117456,-1.48405885957351));
#37923=CARTESIAN_POINT('Ctrl Pts',(-5.99991811455196,9.81783805781404,-1.49054133766801));
#37924=CARTESIAN_POINT('Ctrl Pts',(-5.99992620313177,9.81307118484453,-1.49727692070492));
#37925=CARTESIAN_POINT('Ctrl Pts',(-5.99993158586974,9.80845147725634,-1.50397097353427));
#37926=CARTESIAN_POINT('Ctrl Pts',(-5.9999370371547,9.80377293957075,-1.51075027240407));
#37927=CARTESIAN_POINT('Ctrl Pts',(-5.9999394402226,9.79924553862276,-1.5174867094576));
#37928=CARTESIAN_POINT('Ctrl Pts',(-5.99994448128701,9.79506976773256,-1.52383523346148));
#37929=CARTESIAN_POINT('Ctrl Pts',(-5.99994531690624,9.79437758167727,-1.52488758041793));
#37930=CARTESIAN_POINT('Ctrl Pts',(-5.99994625961908,9.79369497785949,-1.52592919076002));
#37931=CARTESIAN_POINT('Ctrl Pts',(-5.99994737646189,9.79302277710163,-1.526958405299));
#37932=CARTESIAN_POINT('Ctrl Pts',(-5.99997425283644,9.77684653535922,-1.55172604055182));
#37933=CARTESIAN_POINT('Ctrl Pts',(-5.99996042293814,9.76199838214035,-1.57679063138343));
#37934=CARTESIAN_POINT('Ctrl Pts',(-5.99993587672946,9.74841240942493,-1.60210525746293));
#37935=CARTESIAN_POINT('Ctrl Pts',(-5.99991530960845,9.73702880437642,-1.62331623081582));
#37936=CARTESIAN_POINT('Ctrl Pts',(-5.99988812722501,9.72653125073023,-1.6447038648777));
#37937=CARTESIAN_POINT('Ctrl Pts',(-5.9998711787835,9.71689962998366,-1.66626214470264));
#37938=CARTESIAN_POINT('Ctrl Pts',(-5.99985203331414,9.70601946145499,-1.69061502609774));
#37939=CARTESIAN_POINT('Ctrl Pts',(-5.99984751258481,9.69624316928748,-1.71518651254818));
#37940=CARTESIAN_POINT('Ctrl Pts',(-5.99986529071402,9.68757637932992,-1.73999079081509));
#37941=CARTESIAN_POINT('Ctrl Pts',(-5.99988251401862,9.67918006487467,-1.76402097052225));
#37942=CARTESIAN_POINT('Ctrl Pts',(-5.99992124830363,9.67182546041951,-1.78827070432582));
#37943=CARTESIAN_POINT('Ctrl Pts',(-5.99995587878963,9.66555347191789,-1.81275252917949));
#37944=CARTESIAN_POINT('Ctrl Pts',(-5.99997917551999,9.66133415992386,-1.82922202002983));
#37945=CARTESIAN_POINT('Ctrl Pts',(-5.99999991524883,9.65760556987688,-1.84579651491695));
#37946=CARTESIAN_POINT('Ctrl Pts',(-5.99999992273905,9.65438780859768,-1.86247618343571));
#37947=CARTESIAN_POINT('Ctrl Pts',(-5.99998808311063,10.09334672158,-1.2110347210661));
#37948=CARTESIAN_POINT('Ctrl Pts',(-5.99998551891589,10.0961555650809,-1.22746603445882));
#37949=CARTESIAN_POINT('Ctrl Pts',(-5.99924019502052,10.0995867364503,-1.24482748142736));
#37950=CARTESIAN_POINT('Ctrl Pts',(-5.99754681056573,10.1037278134695,-1.26301505141432));
#37951=CARTESIAN_POINT('Ctrl Pts',(-5.99687196657425,10.105378106725,-1.2702631233394));
#37952=CARTESIAN_POINT('Ctrl Pts',(-5.99604634751327,10.1071412272894,-1.27764189205116));
#37953=CARTESIAN_POINT('Ctrl Pts',(-5.99505598209408,10.1090230777761,-1.28514264891433));
#37954=CARTESIAN_POINT('Ctrl Pts',(-5.99264929788291,10.113596157335,-1.30337021700654));
#37955=CARTESIAN_POINT('Ctrl Pts',(-5.98926946606121,10.1188704998751,-1.32232184177371));
#37956=CARTESIAN_POINT('Ctrl Pts',(-5.98476114210219,10.1249156580807,-1.34184178461827));
#37957=CARTESIAN_POINT('Ctrl Pts',(-5.98055933808551,10.1305498073257,-1.36003457089437));
#37958=CARTESIAN_POINT('Ctrl Pts',(-5.97537764155951,10.1368533912459,-1.37872127166542));
#37959=CARTESIAN_POINT('Ctrl Pts',(-5.96908599007236,10.1438834564595,-1.39772962282572));
#37960=CARTESIAN_POINT('Ctrl Pts',(-5.96754611917192,10.1456040528518,-1.40238188414008));
#37961=CARTESIAN_POINT('Ctrl Pts',(-5.96593972334642,10.1473681747883,-1.40705317486269));
#37962=CARTESIAN_POINT('Ctrl Pts',(-5.96426481079894,10.1491766784785,-1.41174048388465));
#37963=CARTESIAN_POINT('Ctrl Pts',(-5.96381007634479,10.1496676825847,-1.41301307624343));
#37964=CARTESIAN_POINT('Ctrl Pts',(-5.96335029118388,10.1501619581831,-1.41428684812407));
#37965=CARTESIAN_POINT('Ctrl Pts',(-5.96288542949712,10.1506595170982,-1.41556174614242));
#37966=CARTESIAN_POINT('Ctrl Pts',(-5.95829898371322,10.1555685622044,-1.42814022014359));
#37967=CARTESIAN_POINT('Ctrl Pts',(-5.95321825935307,10.1607972808259,-1.44082909355127));
#37968=CARTESIAN_POINT('Ctrl Pts',(-5.94761928777537,10.1663565694259,-1.45357194238132));
#37969=CARTESIAN_POINT('Ctrl Pts',(-5.94481980198652,10.1691362137259,-1.45994336679635));
#37970=CARTESIAN_POINT('Ctrl Pts',(-5.94189071237444,10.1719985095046,-1.46632826213982));
#37971=CARTESIAN_POINT('Ctrl Pts',(-5.93882920319315,10.1749447294529,-1.47271846796723));
#37972=CARTESIAN_POINT('Ctrl Pts',(-5.93729844860251,10.1764178394271,-1.47591357088094));
#37973=CARTESIAN_POINT('Ctrl Pts',(-5.93573458582514,10.1779119311141,-1.47910999970802));
#37974=CARTESIAN_POINT('Ctrl Pts',(-5.93413725899299,10.1794271634867,-1.48230668713107));
#37975=CARTESIAN_POINT('Ctrl Pts',(-5.93307814973919,10.1804318399219,-1.48442625412459));
#37976=CARTESIAN_POINT('Ctrl Pts',(-5.93173234065811,10.181702758603,-1.48708001239351));
#37977=CARTESIAN_POINT('Ctrl Pts',(-5.9306387932707,10.1827296550799,-1.48920401045017));
#37978=CARTESIAN_POINT('Ctrl Pts',(-5.93008307493992,10.1832515027864,-1.49028338265501));
#37979=CARTESIAN_POINT('Ctrl Pts',(-5.92959342275462,10.1837099577805,-1.49122653267897));
#37980=CARTESIAN_POINT('Ctrl Pts',(-5.92924452264283,10.1840364429654,-1.49189642960275));
#37981=CARTESIAN_POINT('Ctrl Pts',(-5.92334534744649,10.1895566283702,-1.50322299323332));
#37982=CARTESIAN_POINT('Ctrl Pts',(-5.9166616455774,10.1956931332343,-1.51523970801863));
#37983=CARTESIAN_POINT('Ctrl Pts',(-5.90905335711028,10.2025037329907,-1.52779298919207));
#37984=CARTESIAN_POINT('Ctrl Pts',(-5.90809035048613,10.2033657734757,-1.52938190015112));
#37985=CARTESIAN_POINT('Ctrl Pts',(-5.90711252019561,10.2042386187167,-1.53097933947511));
#37986=CARTESIAN_POINT('Ctrl Pts',(-5.90611957305421,10.2051223903042,-1.53258493413081));
#37987=CARTESIAN_POINT('Ctrl Pts',(-5.8985559999358,10.211854340821,-1.54481522522138));
#37988=CARTESIAN_POINT('Ctrl Pts',(-5.8901147942091,10.2192204202246,-1.55752239042882));
#37989=CARTESIAN_POINT('Ctrl Pts',(-5.88068120099843,10.2272683777287,-1.57053114009695));
#37990=CARTESIAN_POINT('Ctrl Pts',(-5.87365871205742,10.2332593815072,-1.58021502179936));
#37991=CARTESIAN_POINT('Ctrl Pts',(-5.86608634065068,10.2396282268125,-1.59006530425002));
#37992=CARTESIAN_POINT('Ctrl Pts',(-5.85791987654171,10.2463937661191,-1.5999909644792));
#37993=CARTESIAN_POINT('Ctrl Pts',(-5.8474691036833,10.2550517499925,-1.61269301265337));
#37994=CARTESIAN_POINT('Ctrl Pts',(-5.83604472953277,10.2643594640929,-1.62552103427835));
#37995=CARTESIAN_POINT('Ctrl Pts',(-5.82356408577863,10.2743542334951,-1.63823549129981));
#37996=CARTESIAN_POINT('Ctrl Pts',(-5.81185649569968,10.2837299247976,-1.65016241220356));
#37997=CARTESIAN_POINT('Ctrl Pts',(-5.79921845229279,10.2937105873015,-1.66198843389947));
#37998=CARTESIAN_POINT('Ctrl Pts',(-5.78561687265328,10.3043134922338,-1.67349578870636));
#37999=CARTESIAN_POINT('Ctrl Pts',(-5.77289224946348,10.3142327790781,-1.68426121137857));
#38000=CARTESIAN_POINT('Ctrl Pts',(-5.75932421188658,10.3246966185417,-1.69474796424745));
#38001=CARTESIAN_POINT('Ctrl Pts',(-5.74490757706917,10.3357133209617,-1.70473747444832));
#38002=CARTESIAN_POINT('Ctrl Pts',(-5.74093112655276,10.3387519893183,-1.70749281877799));
#38003=CARTESIAN_POINT('Ctrl Pts',(-5.73689025758254,10.341832684617,-1.71021007228805));
#38004=CARTESIAN_POINT('Ctrl Pts',(-5.73278520328664,10.3449555024461,-1.7128840178198));
#38005=CARTESIAN_POINT('Ctrl Pts',(-5.71725900098506,9.85240186273889,-1.52489737983018));
#38006=CARTESIAN_POINT('Ctrl Pts',(-5.71831458271734,10.2527966794643,-1.6937903386106));
#38007=CARTESIAN_POINT('Ctrl Pts',(-5.72040617580086,11.1578210792105,-2.00975541592047));
#38008=CARTESIAN_POINT('Ctrl Pts',(-5.72308285296501,12.6107767816378,-2.2999236291718));
#38009=CARTESIAN_POINT('Ctrl Pts',(-5.72473063324945,14.1774181660355,-2.37059488757382));
#38010=CARTESIAN_POINT('Ctrl Pts',(-5.72548238281593,15.7365634246302,-2.20425498075435));
#38011=CARTESIAN_POINT('Ctrl Pts',(-5.72532247293938,17.2528787711321,-1.80439340096888));
#38012=CARTESIAN_POINT('Ctrl Pts',(-5.72405833313342,18.6535823415443,-1.19618825603203));
#38013=CARTESIAN_POINT('Ctrl Pts',(-5.72276281321446,19.5069765306111,-0.666957242692712));
#38014=CARTESIAN_POINT('Ctrl Pts',(-5.72204189664406,19.8960667901931,-0.386355007630499));
#38015=CARTESIAN_POINT('Ctrl Pts',(-5.89595608811401,9.87373568239816,-1.47442937000013));
#38016=CARTESIAN_POINT('Ctrl Pts',(-5.89686253255657,10.2721856611528,-1.64196412804974));
#38017=CARTESIAN_POINT('Ctrl Pts',(-5.89864681126967,11.1726806565925,-1.95530224537703));
#38018=CARTESIAN_POINT('Ctrl Pts',(-5.90092442591395,12.6178137104256,-2.24261899237967));
#38019=CARTESIAN_POINT('Ctrl Pts',(-5.90232007042876,14.1756913526124,-2.3121121385942));
#38020=CARTESIAN_POINT('Ctrl Pts',(-5.90295601817132,15.7258928867575,-2.14637009402302));
#38021=CARTESIAN_POINT('Ctrl Pts',(-5.90282076518485,17.2336204409562,-1.74885165906947));
#38022=CARTESIAN_POINT('Ctrl Pts',(-5.9017512571849,18.6265772369609,-1.14466085934096));
#38023=CARTESIAN_POINT('Ctrl Pts',(-5.90065106834299,19.47555764694,-0.618889185779098));
#38024=CARTESIAN_POINT('Ctrl Pts',(-5.90003813161803,19.8626858446245,-0.340119139048481));
#38025=CARTESIAN_POINT('Ctrl Pts',(-6.00511196337079,9.93286177430145,-1.33455848991861));
#38026=CARTESIAN_POINT('Ctrl Pts',(-6.00560092878501,10.3255063448102,-1.49931113500935));
#38027=CARTESIAN_POINT('Ctrl Pts',(-6.00654858673405,11.2128931137538,-1.80742765761119));
#38028=CARTESIAN_POINT('Ctrl Pts',(-6.00775094556156,12.6364843163732,-2.08965919677582));
#38029=CARTESIAN_POINT('Ctrl Pts',(-6.00847950177932,14.1710743021289,-2.1576231816053));
#38030=CARTESIAN_POINT('Ctrl Pts',(-6.00881049544709,15.697819310256,-1.99417077940699));
#38031=CARTESIAN_POINT('Ctrl Pts',(-6.00874013038259,17.1829670424457,-1.60265433566748));
#38032=CARTESIAN_POINT('Ctrl Pts',(-6.00818335243022,18.5550088225529,-1.00793604053573));
#38033=CARTESIAN_POINT('Ctrl Pts',(-6.00760532996379,19.3915577425242,-0.490317082630804));
#38034=CARTESIAN_POINT('Ctrl Pts',(-6.00728239242838,19.7730032591172,-0.215899947647808));
#38035=CARTESIAN_POINT('Ctrl Pts',(-5.99984082028272,10.0056907570941,-1.16227147505724));
#38036=CARTESIAN_POINT('Ctrl Pts',(-5.99981405141536,10.3910341666072,-1.32395264497647));
#38037=CARTESIAN_POINT('Ctrl Pts',(-5.99973665762545,11.262073897347,-1.62638254338466));
#38038=CARTESIAN_POINT('Ctrl Pts',(-5.99962568511255,12.6591808586663,-1.90336998277106));
#38039=CARTESIAN_POINT('Ctrl Pts',(-5.99954402211993,14.1654482917451,-1.97007863120369));
#38040=CARTESIAN_POINT('Ctrl Pts',(-5.99950517213815,15.6637821447797,-1.80967547346287));
#38041=CARTESIAN_POINT('Ctrl Pts',(-5.99951348544965,17.1215588901583,-1.42537398644992));
#38042=CARTESIAN_POINT('Ctrl Pts',(-5.99957860877151,18.4680392834296,-0.841725262046986));
#38043=CARTESIAN_POINT('Ctrl Pts',(-5.99963682440262,19.2892036755591,-0.333629249611667));
#38044=CARTESIAN_POINT('Ctrl Pts',(-5.99966774289508,19.6635608898064,-0.0643114939931151));
#38045=CARTESIAN_POINT('',(-5.99999997114735,19.5919329044493,-0.135484571570026));
#38046=CARTESIAN_POINT('Ctrl Pts',(-6.,10.0933467217017,-1.2110347223169));
#38047=CARTESIAN_POINT('Ctrl Pts',(-6.,10.534316803576,-1.39220578035687));
#38048=CARTESIAN_POINT('Ctrl Pts',(-6.,10.9833777640737,-1.54006792738036));
#38049=CARTESIAN_POINT('Ctrl Pts',(-6.,11.4430953897292,-1.65563720843317));
#38050=CARTESIAN_POINT('Ctrl Pts',(-6.,11.9028130153849,-1.77120648948607));
#38051=CARTESIAN_POINT('Ctrl Pts',(-6.,12.3731873061984,-1.85448290456825));
#38052=CARTESIAN_POINT('Ctrl Pts',(-6.,12.8461743612776,-1.90343075106931));
#38053=CARTESIAN_POINT('Ctrl Pts',(-6.,13.3191614163566,-1.95237859757033));
#38054=CARTESIAN_POINT('Ctrl Pts',(-6.,13.7947612357013,-1.96699787549028));
#38055=CARTESIAN_POINT('Ctrl Pts',(-6.,14.2698876719687,-1.94742220019824));
#38056=CARTESIAN_POINT('Ctrl Pts',(-6.,14.7450141082364,-1.92784652490618));
#38057=CARTESIAN_POINT('Ctrl Pts',(-6.,15.2196671614267,-1.87407589640209));
#38058=CARTESIAN_POINT('Ctrl Pts',(-6.,15.6870768618399,-1.78685623436044));
#38059=CARTESIAN_POINT('Ctrl Pts',(-6.,16.1544865622528,-1.69963657231885));
#38060=CARTESIAN_POINT('Ctrl Pts',(-6.,16.6146529098885,-1.57896787673975));
#38061=CARTESIAN_POINT('Ctrl Pts',(-6.,17.0647736754607,-1.4253895422543));
#38062=CARTESIAN_POINT('Ctrl Pts',(-6.,17.5148944410332,-1.27181120776873));
#38063=CARTESIAN_POINT('Ctrl Pts',(-6.,17.954969624542,-1.08532323437677));
#38064=CARTESIAN_POINT('Ctrl Pts',(-6.,18.3770565919024,-0.869913211307542));
#38065=CARTESIAN_POINT('Ctrl Pts',(-6.,18.7991432606589,-0.654503340629331));
#38066=CARTESIAN_POINT('Ctrl Pts',(-6.,19.2032417387183,-0.41017146119544));
#38067=CARTESIAN_POINT('Ctrl Pts',(-6.,19.5919320853478,-0.135483412521195));
#38068=CARTESIAN_POINT('',(-5.736443569433,19.8089505408241,-0.442546871806432));
#38069=CARTESIAN_POINT('Origin',(-5.59998163814211,19.5919264032321,-0.135474791301221));
#38070=CARTESIAN_POINT('Ctrl Pts',(-5.732787989488,10.344952798621,-1.71289145292299));
#38071=CARTESIAN_POINT('Ctrl Pts',(-5.73461480973083,11.1182357741961,-1.99332781082549));
#38072=CARTESIAN_POINT('Ctrl Pts',(-5.73605973941588,11.9265526424831,-2.1816925109264));
#38073=CARTESIAN_POINT('Ctrl Pts',(-5.73818934992294,13.5675395619842,-2.35984303021664));
#38074=CARTESIAN_POINT('Ctrl Pts',(-5.73887403074496,14.4000936737092,-2.35028713240501));
#38075=CARTESIAN_POINT('Ctrl Pts',(-5.73948314352597,16.0408966746419,-2.13191112187471));
#38076=CARTESIAN_POINT('Ctrl Pts',(-5.73940757548497,16.8491806682658,-1.9234336965296));
#38077=CARTESIAN_POINT('Ctrl Pts',(-5.73849619058033,18.3938446694523,-1.31839093065865));
#38078=CARTESIAN_POINT('Ctrl Pts',(-5.73766037378413,19.1301818496608,-0.921733807345979));
#38079=CARTESIAN_POINT('Ctrl Pts',(-5.73644356975675,19.8089503602267,-0.442546999301902));
#38080=CARTESIAN_POINT('Origin',(-5.599999999997,19.5919343769573,-0.135488060979611));
#38081=CARTESIAN_POINT('',(-5.593361696257,19.9918770425242,-0.136828655319171));
#38082=CARTESIAN_POINT('Origin',(-5.599999999997,19.5919343769573,-0.135488060979611));
#38083=CARTESIAN_POINT('Origin',(-5.6,19.5919343770044,-0.135488060981261));
#38084=CARTESIAN_POINT('Ctrl Pts',(-5.59335880963393,19.9918769844261,-0.136831702173518));
#38085=CARTESIAN_POINT('Ctrl Pts',(-5.59335897597995,19.9918902023629,-0.132889263698749));
#38086=CARTESIAN_POINT('Ctrl Pts',(-5.59336249921666,19.9921701764066,-0.0456108094042529));
#38087=CARTESIAN_POINT('Ctrl Pts',(-5.59336249921666,19.9921701764069,0.0456108090956939));
#38088=CARTESIAN_POINT('Ctrl Pts',(-5.59335897597995,19.9918902023646,0.132889263387468));
#38089=CARTESIAN_POINT('Ctrl Pts',(-5.59335880963393,19.9918769844279,0.1368317018641));
#38090=CARTESIAN_POINT('Ctrl Pts',(-5.83074004395878,19.9958187405297,-0.136844915099747));
#38091=CARTESIAN_POINT('Ctrl Pts',(-5.83074021194014,19.9958318610111,-0.13290209557407));
#38092=CARTESIAN_POINT('Ctrl Pts',(-5.8307437698124,19.9961097709333,-0.0456152065241548));
#38093=CARTESIAN_POINT('Ctrl Pts',(-5.83074376981241,19.9961097709314,0.0456152062141224));
#38094=CARTESIAN_POINT('Ctrl Pts',(-5.83074021194014,19.9958318610128,0.132902095265602));
#38095=CARTESIAN_POINT('Ctrl Pts',(-5.83074004395878,19.9958187405316,0.13684491479334));
#38096=CARTESIAN_POINT('Ctrl Pts',(-6.00000347483923,19.8293408303182,-0.136286874323723));
#38097=CARTESIAN_POINT('Ctrl Pts',(-6.00000357357543,19.8293538265013,-0.132360134067916));
#38098=CARTESIAN_POINT('Ctrl Pts',(-6.0000056648227,19.8296291037059,-0.0454292086005723));
#38099=CARTESIAN_POINT('Ctrl Pts',(-6.0000056648227,19.8296291037082,0.0454292082960187));
#38100=CARTESIAN_POINT('Ctrl Pts',(-6.00000357357543,19.8293538265043,0.132360133764452));
#38101=CARTESIAN_POINT('Ctrl Pts',(-6.00000347483923,19.8293408303212,0.136286874022268));
#38102=CARTESIAN_POINT('Ctrl Pts',(-5.9999999999769,19.5919285123983,-0.135491058510798));
#38103=CARTESIAN_POINT('Ctrl Pts',(-5.99999999996753,19.5919414317191,-0.131587249061459));
#38104=CARTESIAN_POINT('Ctrl Pts',(-5.99999999976694,19.5922150808793,-0.0451639658275902));
#38105=CARTESIAN_POINT('Ctrl Pts',(-5.99999999976694,19.5922150808828,0.0451639655258831));
#38106=CARTESIAN_POINT('Ctrl Pts',(-5.99999999996752,19.591941431722,0.131587248762196));
#38107=CARTESIAN_POINT('Ctrl Pts',(-5.9999999999769,19.5919285124013,0.135491058213587));
#38108=CARTESIAN_POINT('Origin',(-5.47627593058377,-17.2218949143738,6.06772203221723E-6));
#38109=CARTESIAN_POINT('Ctrl Pts',(-6.00000000001697,19.5919329102797,-0.135482829540219));
#38110=CARTESIAN_POINT('Ctrl Pts',(-6.00000000001005,19.5919459863958,-0.131581789340447));
#38111=CARTESIAN_POINT('Ctrl Pts',(-6.00000000000347,19.591958508822,-0.127680725304212));
#38112=CARTESIAN_POINT('Ctrl Pts',(-5.9999999999973,19.5919704756381,-0.123779639821517));
#38113=CARTESIAN_POINT('Ctrl Pts',(-5.99999999993208,19.5920970397706,-0.082520754142832));
#38114=CARTESIAN_POINT('Ctrl Pts',(-5.99999999990817,19.5921614523042,-0.0412594672366372));
#38115=CARTESIAN_POINT('Ctrl Pts',(-5.99999999990817,19.5921614509438,1.4231705702387E-6));
#38116=CARTESIAN_POINT('Ctrl Pts',(-5.99999999990817,19.5921614495833,0.0412621564140265));
#38117=CARTESIAN_POINT('Ctrl Pts',(-5.99999999993208,19.5920970348205,0.0825224934060036));
#38118=CARTESIAN_POINT('Ctrl Pts',(-5.9999999999973,19.5919704760335,0.123779639519311));
#38119=CARTESIAN_POINT('Ctrl Pts',(-6.00000000000346,19.5919585091951,0.12768073253251));
#38120=CARTESIAN_POINT('Ctrl Pts',(-6.00000000001005,19.5919459867654,0.131581797037309));
#38121=CARTESIAN_POINT('Ctrl Pts',(-6.00000000001698,19.5919329106708,0.135482830646012));
#38122=CARTESIAN_POINT('Ctrl Pts',(-5.67764080611035,19.9920086654548,-0.35317650519169));
#38123=CARTESIAN_POINT('Ctrl Pts',(-3.78509387074023,19.9513483860085,-1.26988355976882));
#38124=CARTESIAN_POINT('Ctrl Pts',(-2.0656550255016E-10,19.8990602291944,
-2.18625140349313));
#38125=CARTESIAN_POINT('Ctrl Pts',(3.78509387032731,19.9513483860076,-1.26988355987377));
#38126=CARTESIAN_POINT('Ctrl Pts',(5.67764080549097,19.9920086654425,-0.353176505498152));
#38127=CARTESIAN_POINT('Ctrl Pts',(-5.67764080611035,19.9939837518553,-0.127283758352494));
#38128=CARTESIAN_POINT('Ctrl Pts',(-3.78509387074023,19.9624116465656,-0.457857765159308));
#38129=CARTESIAN_POINT('Ctrl Pts',(-2.0656550255016E-10,20.0792796545209,
-0.792979083240276));
#38130=CARTESIAN_POINT('Ctrl Pts',(3.78509387032731,19.9624116465789,-0.457857765200401));
#38131=CARTESIAN_POINT('Ctrl Pts',(5.67764080549097,19.9939837518422,-0.127283758470664));
#38132=CARTESIAN_POINT('Ctrl Pts',(-5.67764080611035,19.9940637065833,0.0986861771942666));
#38133=CARTESIAN_POINT('Ctrl Pts',(-3.78509387074023,19.9628595054405,0.355008386647923));
#38134=CARTESIAN_POINT('Ctrl Pts',(-2.0656550255016E-10,20.0865752314139,
0.615338279627633));
#38135=CARTESIAN_POINT('Ctrl Pts',(3.78509387032731,19.9628595054527,0.355008386675378));
#38136=CARTESIAN_POINT('Ctrl Pts',(5.67764080549097,19.9940637065743,0.0986861772782846));
#38137=CARTESIAN_POINT('Ctrl Pts',(-5.67764080611035,19.9922485296364,0.324585173480459));
#38138=CARTESIAN_POINT('Ctrl Pts',(-3.78509387074023,19.9526919626316,1.16710221932013));
#38139=CARTESIAN_POINT('Ctrl Pts',(-2.0656550255016E-10,19.9209469598825,
2.00982869570971));
#38140=CARTESIAN_POINT('Ctrl Pts',(3.78509387032731,19.9526919626278,1.16710221941215));
#38141=CARTESIAN_POINT('Ctrl Pts',(5.67764080549097,19.9922485296225,0.324585173755783));
#38142=CARTESIAN_POINT('Ctrl Pts',(-5.59336169625714,19.9918770425157,-0.136828655319142));
#38143=CARTESIAN_POINT('Ctrl Pts',(-5.58009644017448,19.9916362290972,-0.142984613489992));
#38144=CARTESIAN_POINT('Ctrl Pts',(-5.56074613957355,19.9912865571345,-0.151958711829183));
#38145=CARTESIAN_POINT('Ctrl Pts',(-5.53527458568659,19.9908348355144,-0.163677026593076));
#38146=CARTESIAN_POINT('Ctrl Pts',(-5.50989210816338,19.9903846936063,-0.175354361333796));
#38147=CARTESIAN_POINT('Ctrl Pts',(-5.47843096000199,19.9898333361175,-0.1897568285786));
#38148=CARTESIAN_POINT('Ctrl Pts',(-5.44083463266139,19.9891901590629,-0.206764048111785));
#38149=CARTESIAN_POINT('Ctrl Pts',(-5.41345000419988,19.9887216780723,-0.219151864183826));
#38150=CARTESIAN_POINT('Ctrl Pts',(-5.38280993341899,19.988204554942,-0.232920656878242));
#38151=CARTESIAN_POINT('Ctrl Pts',(-5.34888648441068,19.9876426410121,-0.248007586354099));
#38152=CARTESIAN_POINT('Ctrl Pts',(-5.30328426181425,19.9868872778383,-0.268288469824585));
#38153=CARTESIAN_POINT('Ctrl Pts',(-5.25174934336198,19.9860509360498,-0.290953240785525));
#38154=CARTESIAN_POINT('Ctrl Pts',(-5.19419938879444,19.9851442256669,-0.315807394008167));
#38155=CARTESIAN_POINT('Ctrl Pts',(-5.15774847931625,19.9845699347168,-0.331549482704565));
#38156=CARTESIAN_POINT('Ctrl Pts',(-5.11888420994136,19.9839674252062,-0.348168925542301));
#38157=CARTESIAN_POINT('Ctrl Pts',(-5.07758279458025,19.9833392305093,-0.365605829096777));
#38158=CARTESIAN_POINT('Ctrl Pts',(-5.01428717619997,19.9823765038944,-0.392328390139004));
#38159=CARTESIAN_POINT('Ctrl Pts',(-4.94526809252529,19.9813534060161,-0.420973376428607));
#38160=CARTESIAN_POINT('Ctrl Pts',(-4.87042927244288,19.9802806512975,-0.451284601016866));
#38161=CARTESIAN_POINT('Ctrl Pts',(-4.84061551917361,19.979853294954,-0.463359769628138));
#38162=CARTESIAN_POINT('Ctrl Pts',(-4.80987804835423,19.9794180560131,-0.475698813708442));
#38163=CARTESIAN_POINT('Ctrl Pts',(-4.77821033097395,19.9789755899773,-0.488283254179042));
#38164=CARTESIAN_POINT('Ctrl Pts',(-4.70107154376649,19.9778977954215,-0.518937452078098));
#38165=CARTESIAN_POINT('Ctrl Pts',(-4.61841362640652,19.9767770765998,-0.55105125131751));
#38166=CARTESIAN_POINT('Ctrl Pts',(-4.53013604499199,19.9756247565424,-0.58432225556632));
#38167=CARTESIAN_POINT('Ctrl Pts',(-4.50293366277614,19.9752696737441,-0.594574581918937));
#38168=CARTESIAN_POINT('Ctrl Pts',(-4.47519762071291,19.9749115925001,-0.60493642323504));
#38169=CARTESIAN_POINT('Ctrl Pts',(-4.44692485275567,19.9745508479666,-0.615397929701921));
#38170=CARTESIAN_POINT('Ctrl Pts',(-4.35781685172489,19.9734138802558,-0.648369725404562));
#38171=CARTESIAN_POINT('Ctrl Pts',(-4.26337760100315,19.9722503887103,-0.682335366219507));
#38172=CARTESIAN_POINT('Ctrl Pts',(-4.16350896254227,19.9710726333925,-0.716953413664895));
#38173=CARTESIAN_POINT('Ctrl Pts',(-4.13544397277845,19.9707416617136,-0.72668174442189));
#38174=CARTESIAN_POINT('Ctrl Pts',(-4.10695019601858,19.9704095684455,-0.736461284000019));
#38175=CARTESIAN_POINT('Ctrl Pts',(-4.07802541747408,19.9700766365274,-0.746283705314207));
#38176=CARTESIAN_POINT('Ctrl Pts',(-3.98974865350231,19.9690605474222,-0.776261171404391));
#38177=CARTESIAN_POINT('Ctrl Pts',(-3.89745734273723,19.9680365943023,-0.806640345102402));
#38178=CARTESIAN_POINT('Ctrl Pts',(-3.80108980409398,19.9670138196758,-0.837164813292626));
#38179=CARTESIAN_POINT('Ctrl Pts',(-3.75649682634983,19.9665405424001,-0.851289662280391));
#38180=CARTESIAN_POINT('Ctrl Pts',(-3.71103102503581,19.9660675268623,-0.865445191326704));
#38181=CARTESIAN_POINT('Ctrl Pts',(-3.66468636938461,19.9655957181186,-0.879603669421038));
#38182=CARTESIAN_POINT('Ctrl Pts',(-3.629247389634,19.965234933897,-0.890430419807553));
#38183=CARTESIAN_POINT('Ctrl Pts',(-3.59329450760697,19.9648748557562,-0.901258864403766));
#38184=CARTESIAN_POINT('Ctrl Pts',(-3.55682518356218,19.9645159343212,-0.912076066338966));
#38185=CARTESIAN_POINT('Ctrl Pts',(-3.51474448708024,19.9641017872438,-0.924557662950405));
#38186=CARTESIAN_POINT('Ctrl Pts',(-3.47197612954805,19.9636891723991,-0.937024514001034));
#38187=CARTESIAN_POINT('Ctrl Pts',(-3.42851638066827,19.9632788118654,-0.949455625228041));
#38188=CARTESIAN_POINT('Ctrl Pts',(-3.40678650622838,19.9630736315986,-0.955671180841545));
#38189=CARTESIAN_POINT('Ctrl Pts',(-3.38488378395104,19.9628690147478,-0.961877801491924));
#38190=CARTESIAN_POINT('Ctrl Pts',(-3.36280774484562,19.9626650525873,-0.968072805286863));
#38191=CARTESIAN_POINT('Ctrl Pts',(-3.35176972529291,19.962563071507,-0.971170307184331));
#38192=CARTESIAN_POINT('Ctrl Pts',(-3.34068837653317,19.9624612540851,-0.974264904867446));
#38193=CARTESIAN_POINT('Ctrl Pts',(-3.32956364118686,19.9623596118574,-0.977356257519711));
#38194=CARTESIAN_POINT('Ctrl Pts',(-3.3240012735137,19.9623087907436,-0.978901933845844));
#38195=CARTESIAN_POINT('Ctrl Pts',(-3.3184280591939,19.9622580134274,-0.980446798914225));
#38196=CARTESIAN_POINT('Ctrl Pts',(-3.3128439911071,19.9622072813604,-0.981990809731292));
#38197=CARTESIAN_POINT('Ctrl Pts',(-3.30725992302029,19.9621565492934,-0.983534820548359));
#38198=CARTESIAN_POINT('Ctrl Pts',(-3.30284643870994,19.9621165350483,-0.984752940852499));
#38199=CARTESIAN_POINT('Ctrl Pts',(-3.29605921844197,19.9620552223591,-0.986620236315678));
#38200=CARTESIAN_POINT('Ctrl Pts',(-3.26420947507747,19.9617675061309,-0.995382716232327));
#38201=CARTESIAN_POINT('Ctrl Pts',(-3.23246236011294,19.961485434778,-1.00399045631962));
#38202=CARTESIAN_POINT('Ctrl Pts',(-3.20081930664225,19.961208906558,-1.01244547959457));
#38203=CARTESIAN_POINT('Ctrl Pts',(-3.02528053482623,19.959674875585,-1.05934943602643));
#38204=CARTESIAN_POINT('Ctrl Pts',(-2.85294730098256,19.9583113839894,-1.10155240253784));
#38205=CARTESIAN_POINT('Ctrl Pts',(-2.68405734163335,19.9571013326502,-1.13942220670422));
#38206=CARTESIAN_POINT('Ctrl Pts',(-2.50183512028643,19.9557957592235,-1.18028147307956));
#38207=CARTESIAN_POINT('Ctrl Pts',(-2.32362196300848,19.9546687611369,-1.21609717693824));
#38208=CARTESIAN_POINT('Ctrl Pts',(-2.14968414857974,19.9536983326622,-1.24736532756201));
#38209=CARTESIAN_POINT('Ctrl Pts',(-2.13682519108344,19.9536265903643,-1.2496769342772));
#38210=CARTESIAN_POINT('Ctrl Pts',(-2.12398957691993,19.9535557043388,-1.25196368987188));
#38211=CARTESIAN_POINT('Ctrl Pts',(-2.11117740271896,19.9534856659585,-1.25422579612376));
#38212=CARTESIAN_POINT('Ctrl Pts',(-1.93621865309989,19.95252924535,-1.28511635967114));
#38213=CARTESIAN_POINT('Ctrl Pts',(-1.7656353215977,19.9517307044816,-1.31141089660614));
#38214=CARTESIAN_POINT('Ctrl Pts',(-1.59966046888125,19.9510660881632,-1.33364632095043));
#38215=CARTESIAN_POINT('Ctrl Pts',(-1.55744726884481,19.9508970530285,-1.33930156570817));
#38216=CARTESIAN_POINT('Ctrl Pts',(-1.51553191190328,19.9507366921506,-1.34469420710316));
#38217=CARTESIAN_POINT('Ctrl Pts',(-1.47391771006237,19.9505846339209,-1.34983299816217));
#38218=CARTESIAN_POINT('Ctrl Pts',(-1.30946665097347,19.9499837300033,-1.37014047961576));
#38219=CARTESIAN_POINT('Ctrl Pts',(-1.14972249295738,19.949512234599,-1.386485381975));
#38220=CARTESIAN_POINT('Ctrl Pts',(-0.994867945863715,19.949145973856,-1.39942373538886));
#38221=CARTESIAN_POINT('Ctrl Pts',(-0.92299758083666,19.9489759866403,-1.40542862320233));
#38222=CARTESIAN_POINT('Ctrl Pts',(-0.852179763116334,19.9488287115822,
-1.41069942676756));
#38223=CARTESIAN_POINT('Ctrl Pts',(-0.782429370782511,19.9487019529345,
-1.41529007975822));
#38224=CARTESIAN_POINT('Ctrl Pts',(-0.633135744668933,19.9484306389314,
-1.42511590594029));
#38225=CARTESIAN_POINT('Ctrl Pts',(-0.488734978173752,19.9482529345977,
-1.43182821637309));
#38226=CARTESIAN_POINT('Ctrl Pts',(-0.349348859034708,19.9481438619172,
-1.43595954720335));
#38227=CARTESIAN_POINT('Ctrl Pts',(-0.262235554798481,19.9480756938553,
-1.43854153945438));
#38228=CARTESIAN_POINT('Ctrl Pts',(-0.177080119018712,19.9480344392527,
-1.44011472297812));
#38229=CARTESIAN_POINT('Ctrl Pts',(-0.0939047509515874,19.9480149632798,
-1.44080217709803));
#38230=CARTESIAN_POINT('Ctrl Pts',(0.0408608604582856,19.9479834071659,
-1.44191603059744));
#38231=CARTESIAN_POINT('Ctrl Pts',(0.170426608443204,19.9480093358015,-1.44070684670635));
#38232=CARTESIAN_POINT('Ctrl Pts',(0.294722178057082,19.9480858363438,-1.43767395803733));
#38233=CARTESIAN_POINT('Ctrl Pts',(0.343048654823458,19.9481155799758,-1.43649476215566));
#38234=CARTESIAN_POINT('Ctrl Pts',(0.390578812885668,19.9481529485472,-1.43503944637556));
#38235=CARTESIAN_POINT('Ctrl Pts',(0.437309817035389,19.9481974668766,-1.43333570032628));
#38236=CARTESIAN_POINT('Ctrl Pts',(0.473889188802879,19.948232314245,-1.43200206837747));
#38237=CARTESIAN_POINT('Ctrl Pts',(0.509978917138882,19.9482715416553,-1.43051619975346));
#38238=CARTESIAN_POINT('Ctrl Pts',(0.545577925881862,19.9483149076229,-1.42889097738007));
#38239=CARTESIAN_POINT('Ctrl Pts',(0.575261242611154,19.9483510672183,-1.42753582755516));
#38240=CARTESIAN_POINT('Ctrl Pts',(0.60460338601008,19.9483901039359,-1.42608378579906));
#38241=CARTESIAN_POINT('Ctrl Pts',(0.633603956839183,19.9484318697382,-1.42454228018567));
#38242=CARTESIAN_POINT('Ctrl Pts',(0.665494340265893,19.9484777973669,-1.42284716854958));
#38243=CARTESIAN_POINT('Ctrl Pts',(0.696971606900236,19.9485270246339,-1.42104388842941));
#38244=CARTESIAN_POINT('Ctrl Pts',(0.728035441233224,19.9485793495753,-1.41914204120244));
#38245=CARTESIAN_POINT('Ctrl Pts',(0.743567358399718,19.948605512046,-1.41819111758896));
#38246=CARTESIAN_POINT('Ctrl Pts',(0.758995917489945,19.948632448546,-1.41721555217114));
#38247=CARTESIAN_POINT('Ctrl Pts',(0.774321073339735,19.9486601335504,-1.4162165167394));
#38248=CARTESIAN_POINT('Ctrl Pts',(0.78198365126463,19.9486739760527,-1.41571699902353));
#38249=CARTESIAN_POINT('Ctrl Pts',(0.789620378379354,19.9486880056576,-1.41521161380253));
#38250=CARTESIAN_POINT('Ctrl Pts',(0.79723125033673,19.9487022191044,-1.4147005065104));
#38251=CARTESIAN_POINT('Ctrl Pts',(0.804842122294106,19.9487164325513,-1.41418939921827));
#38252=CARTESIAN_POINT('Ctrl Pts',(0.8141885175813,19.9487342266443,-1.41355084271498));
#38253=CARTESIAN_POINT('Ctrl Pts',(0.819986296612124,19.9487454076543,-1.41315016332844));
#38254=CARTESIAN_POINT('Ctrl Pts',(0.912968818718277,19.9489247243383,-1.40672422337471));
#38255=CARTESIAN_POINT('Ctrl Pts',(1.01085354077577,19.949146375472,-1.39887348397393));
#38256=CARTESIAN_POINT('Ctrl Pts',(1.11358303380358,19.9494232496908,-1.38924753938107));
#38257=CARTESIAN_POINT('Ctrl Pts',(1.22623353893273,19.9497268627981,-1.37869197749938));
#38258=CARTESIAN_POINT('Ctrl Pts',(1.34471056382887,19.950096901445,-1.36600184523302));
#38259=CARTESIAN_POINT('Ctrl Pts',(1.46890925483827,19.9505514692569,-1.35068217452509));
#38260=CARTESIAN_POINT('Ctrl Pts',(1.5153837961882,19.9507215663037,-1.34494962884368));
#38261=CARTESIAN_POINT('Ctrl Pts',(1.56265915662713,19.9509035257976,-1.33884849850583));
#38262=CARTESIAN_POINT('Ctrl Pts',(1.61072854604317,19.9510983943111,-1.33235148126275));
#38263=CARTESIAN_POINT('Ctrl Pts',(1.74017460898387,19.9516231557482,-1.31485566296359));
#38264=CARTESIAN_POINT('Ctrl Pts',(1.87538176880813,19.9522413543956,-1.29449106412342));
#38265=CARTESIAN_POINT('Ctrl Pts',(2.01619359019374,19.9529742557988,-1.27071133078169));
#38266=CARTESIAN_POINT('Ctrl Pts',(2.02948594399093,19.9530434402227,-1.26846657160117));
#38267=CARTESIAN_POINT('Ctrl Pts',(2.04282820892096,19.9531136486326,-1.26619135877892));
#38268=CARTESIAN_POINT('Ctrl Pts',(2.05622023297625,19.9531849000987,-1.26388521963766));
#38269=CARTESIAN_POINT('Ctrl Pts',(2.18611588762425,19.9538760021906,-1.24151687171451));
#38270=CARTESIAN_POINT('Ctrl Pts',(2.32069562415765,19.954665116498,-1.21624008450209));
#38271=CARTESIAN_POINT('Ctrl Pts',(2.45980641014352,19.9555695145239,-1.1876232037297));
#38272=CARTESIAN_POINT('Ctrl Pts',(2.57751721920422,19.95633478533,-1.16340857389609));
#38273=CARTESIAN_POINT('Ctrl Pts',(2.69847171415293,19.9571826339952,-1.13680195572644));
#38274=CARTESIAN_POINT('Ctrl Pts',(2.82256104373563,19.9581238872826,-1.10754080826207));
#38275=CARTESIAN_POINT('Ctrl Pts',(2.92925609544617,19.9589331999649,-1.0823813553718));
#38276=CARTESIAN_POINT('Ctrl Pts',(3.03826843858179,19.959811580392,-1.05525922949466));
#38277=CARTESIAN_POINT('Ctrl Pts',(3.14952010306516,19.9607660880248,-1.02600930039865));
#38278=CARTESIAN_POINT('Ctrl Pts',(3.24640822738728,19.961597360569,-1.00053578699257));
#38279=CARTESIAN_POINT('Ctrl Pts',(3.34499460831031,19.9624863767901,-0.973448371221141));
#38280=CARTESIAN_POINT('Ctrl Pts',(3.44522290327178,19.9634379571108,-0.944640100632512));
#38281=CARTESIAN_POINT('Ctrl Pts',(3.44872500124271,19.9634712064792,-0.94363350478038));
#38282=CARTESIAN_POINT('Ctrl Pts',(3.4522291031841,19.963504532248,-0.942624808085872));
#38283=CARTESIAN_POINT('Ctrl Pts',(3.45573520662724,19.9635379346302,-0.941614006063889));
#38284=CARTESIAN_POINT('Ctrl Pts',(3.53381527373909,19.964281797521,-0.919103691980711));
#38285=CARTESIAN_POINT('Ctrl Pts',(3.61288815483183,19.9650636505888,-0.895549195410826));
#38286=CARTESIAN_POINT('Ctrl Pts',(3.69292540203938,19.9658858830604,-0.870901362357781));
#38287=CARTESIAN_POINT('Ctrl Pts',(3.6995495805477,19.9659539340598,-0.868861416561504));
#38288=CARTESIAN_POINT('Ctrl Pts',(3.70618036478951,19.966022261695,-0.866813981888607));
#38289=CARTESIAN_POINT('Ctrl Pts',(3.71281773769273,19.9660908673404,-0.864759030751817));
#38290=CARTESIAN_POINT('Ctrl Pts',(3.74627869963934,19.9664367287111,-0.854399413657385));
#38291=CARTESIAN_POINT('Ctrl Pts',(3.77990711552836,19.9667896554082,-0.84384876565254));
#38292=CARTESIAN_POINT('Ctrl Pts',(3.81370081233948,19.9671498333894,-0.833103598408753));
#38293=CARTESIAN_POINT('Ctrl Pts',(3.83394934812138,19.9673656451362,-0.826665300029194));
#38294=CARTESIAN_POINT('Ctrl Pts',(3.85425722301091,19.967584060312,-0.820157165131984));
#38295=CARTESIAN_POINT('Ctrl Pts',(3.87462396755603,19.9678051193895,-0.813578448686667));
#38296=CARTESIAN_POINT('Ctrl Pts',(3.88480733982858,19.9679156489282,-0.81028909046401));
#38297=CARTESIAN_POINT('Ctrl Pts',(3.89500542951504,19.9680268394502,-0.806982086854589));
#38298=CARTESIAN_POINT('Ctrl Pts',(3.90521817679822,19.9681386960524,-0.80365734496727));
#38299=CARTESIAN_POINT('Ctrl Pts',(3.9103245504398,19.9681946243536,-0.80199497402361));
#38300=CARTESIAN_POINT('Ctrl Pts',(3.91543458848057,19.9682507191752,-0.800328168510491));
#38301=CARTESIAN_POINT('Ctrl Pts',(3.92054828339348,19.9683069811566,-0.798656916846781));
#38302=CARTESIAN_POINT('Ctrl Pts',(3.92566197830639,19.9683632431379,-0.796985665183072));
#38303=CARTESIAN_POINT('Ctrl Pts',(3.93254611564147,19.9684391986675,-0.794730300529606));
#38304=CARTESIAN_POINT('Ctrl Pts',(3.93590033120455,19.9684762692202,-0.793629811831234));
#38305=CARTESIAN_POINT('Ctrl Pts',(3.94215184182074,19.9685453604724,-0.791578746045063));
#38306=CARTESIAN_POINT('Ctrl Pts',(3.9483863655703,19.9686144529542,-0.789528428402651));
#38307=CARTESIAN_POINT('Ctrl Pts',(3.95460391946738,19.9686835441334,-0.787478931678669));
#38308=CARTESIAN_POINT('Ctrl Pts',(4.02981766560043,19.9695193400903,-0.7626861709162));
#38309=CARTESIAN_POINT('Ctrl Pts',(4.10254807853478,19.9703549292316,-0.738014505222679));
#38310=CARTESIAN_POINT('Ctrl Pts',(4.17282587992973,19.9711860991373,-0.713586601878876));
#38311=CARTESIAN_POINT('Ctrl Pts',(4.24075388496264,19.9719894781903,-0.689975465668788));
#38312=CARTESIAN_POINT('Ctrl Pts',(4.30639057596857,19.9727887343623,-0.666591965479921));
#38313=CARTESIAN_POINT('Ctrl Pts',(4.36976383144435,19.9735803936586,-0.643536957258541));
#38314=CARTESIAN_POINT('Ctrl Pts',(4.4312145094457,19.9743480360992,-0.621181377197298));
#38315=CARTESIAN_POINT('Ctrl Pts',(4.49053701984079,19.975108541002,-0.599134582787114));
#38316=CARTESIAN_POINT('Ctrl Pts',(4.54775645035834,19.9758590147286,-0.577480233927572));
#38317=CARTESIAN_POINT('Ctrl Pts',(4.60351117578851,19.9765902778012,-0.556380193886757));
#38318=CARTESIAN_POINT('Ctrl Pts',(4.65726912327683,19.9773120217359,-0.535652705120557));
#38319=CARTESIAN_POINT('Ctrl Pts',(4.70905288636104,19.9780217932391,-0.515368113490108));
#38320=CARTESIAN_POINT('Ctrl Pts',(4.75987167760566,19.9787183384052,-0.495461517944441));
#38321=CARTESIAN_POINT('Ctrl Pts',(4.80878918171655,19.979403358028,-0.47598142251901));
#38322=CARTESIAN_POINT('Ctrl Pts',(4.85582595140891,19.9800747136533,-0.456988155099427));
#38323=CARTESIAN_POINT('Ctrl Pts',(4.90207918063831,19.9807348858088,-0.438311278317304));
#38324=CARTESIAN_POINT('Ctrl Pts',(4.94651381542896,19.9813818500243,-0.420105108591858));
#38325=CARTESIAN_POINT('Ctrl Pts',(4.98914848403816,19.9820137117629,-0.402421574654211));
#38326=CARTESIAN_POINT('Ctrl Pts',(4.98949674229069,19.9820188730805,-0.402277127967314));
#38327=CARTESIAN_POINT('Ctrl Pts',(4.9898448804389,19.9820240333899,-0.402132716123775));
#38328=CARTESIAN_POINT('Ctrl Pts',(4.99019289849271,19.98202919269,-0.401988339150492));
#38329=CARTESIAN_POINT('Ctrl Pts',(5.03325928093211,19.9826676434525,-0.384122042046895));
#38330=CARTESIAN_POINT('Ctrl Pts',(5.07448668103045,19.9832906519714,-0.366790155603053));
#38331=CARTESIAN_POINT('Ctrl Pts',(5.11389326225468,19.9838963666681,-0.350040984422825));
#38332=CARTESIAN_POINT('Ctrl Pts',(5.15369851227836,19.9845082092638,-0.33312236510072));
#38333=CARTESIAN_POINT('Ctrl Pts',(5.19164591949423,19.9851024113326,-0.316798299988091));
#38334=CARTESIAN_POINT('Ctrl Pts',(5.22775300183307,19.9856771307056,-0.30111336975242));
#38335=CARTESIAN_POINT('Ctrl Pts',(5.26453925416354,19.9862626604828,-0.285133407815299));
#38336=CARTESIAN_POINT('Ctrl Pts',(5.29941530406552,19.9868279722818,-0.269816847791514));
#38337=CARTESIAN_POINT('Ctrl Pts',(5.3323983228196,19.9873711404656,-0.25520554745017));
#38338=CARTESIAN_POINT('Ctrl Pts',(5.36641335074965,19.9879313038963,-0.240137072581005));
#38339=CARTESIAN_POINT('Ctrl Pts',(5.3984150436722,19.9884679195571,-0.225818690317629));
#38340=CARTESIAN_POINT('Ctrl Pts',(5.42842066614577,19.988978852473,-0.212290672821496));
#38341=CARTESIAN_POINT('Ctrl Pts',(5.45996866123902,19.9895160487648,-0.198067277523987));
#38342=CARTESIAN_POINT('Ctrl Pts',(5.48931013100147,19.9900248540869,-0.184717620138269));
#38343=CARTESIAN_POINT('Ctrl Pts',(5.51646318129326,19.9905027280262,-0.172282013503108));
#38344=CARTESIAN_POINT('Ctrl Pts',(5.54440810117859,19.9909945382946,-0.159483744895691));
#38345=CARTESIAN_POINT('Ctrl Pts',(5.5700351312696,19.9914535784914,-0.147653628555669));
#38346=CARTESIAN_POINT('Ctrl Pts',(5.59336166012999,19.9918770419872,-0.136828574471761));
#38347=CARTESIAN_POINT('Ctrl Pts',(-5.84637330108191,19.8012033146892,-0.398518179817078));
#38348=CARTESIAN_POINT('Ctrl Pts',(-5.81071183853046,19.8004234735737,-0.415207321699024));
#38349=CARTESIAN_POINT('Ctrl Pts',(-5.69191996061893,19.7978801854681,-0.470269915973425));
#38350=CARTESIAN_POINT('Ctrl Pts',(-5.48049741251962,19.7936452864078,-0.565143604366032));
#38351=CARTESIAN_POINT('Ctrl Pts',(-5.20215554401679,19.7885001063612,-0.684048267802473));
#38352=CARTESIAN_POINT('Ctrl Pts',(-4.89414931300705,19.7832362546721,-0.808353235124788));
#38353=CARTESIAN_POINT('Ctrl Pts',(-4.55276913238558,19.7778650102664,-0.937266430508365));
#38354=CARTESIAN_POINT('Ctrl Pts',(-4.1723835688134,19.7724100565091,-1.06997734570926));
#38355=CARTESIAN_POINT('Ctrl Pts',(-3.74657439469389,19.7669368801863,-1.20488365535651));
#38356=CARTESIAN_POINT('Ctrl Pts',(-3.27003381843662,19.761584724194,-1.33873908498052));
#38357=CARTESIAN_POINT('Ctrl Pts',(-2.73868853585576,19.7565628732899,-1.46664667446678));
#38358=CARTESIAN_POINT('Ctrl Pts',(-2.14775624696211,19.7521256584225,-1.58252476859859));
#38359=CARTESIAN_POINT('Ctrl Pts',(-1.49664356855033,19.7486057968215,-1.67793559717415));
#38360=CARTESIAN_POINT('Ctrl Pts',(-0.805427675692797,19.7463898065183,
-1.74162179620427));
#38361=CARTESIAN_POINT('Ctrl Pts',(-0.11332682193267,19.7456265332955,-1.76632927594041));
#38362=CARTESIAN_POINT('Ctrl Pts',(0.536179045116112,19.7459830344993,-1.75438694563656));
#38363=CARTESIAN_POINT('Ctrl Pts',(1.11984701057849,19.7473096705852,-1.71489328080823));
#38364=CARTESIAN_POINT('Ctrl Pts',(1.63691896308617,19.7493622962935,-1.65738847905435));
#38365=CARTESIAN_POINT('Ctrl Pts',(2.09763398182801,19.7519182398037,-1.58838117097954));
#38366=CARTESIAN_POINT('Ctrl Pts',(2.51226399849238,19.7548276213681,-1.51186339189556));
#38367=CARTESIAN_POINT('Ctrl Pts',(2.88624760872843,19.7579578014457,-1.43111102238662));
#38368=CARTESIAN_POINT('Ctrl Pts',(3.2232642926507,19.7611949382187,-1.3488210050365));
#38369=CARTESIAN_POINT('Ctrl Pts',(3.52768199159861,19.7644624365646,-1.26672665052053));
#38370=CARTESIAN_POINT('Ctrl Pts',(3.80292724591826,19.7677009282426,-1.18614757862148));
#38371=CARTESIAN_POINT('Ctrl Pts',(4.05164145124967,19.7708623531949,-1.10814408881512));
#38372=CARTESIAN_POINT('Ctrl Pts',(4.27616841473193,19.7739109745617,-1.03349245184477));
#38373=CARTESIAN_POINT('Ctrl Pts',(4.47886355116955,19.7768248933238,-0.962648114845364));
#38374=CARTESIAN_POINT('Ctrl Pts',(4.66208312282989,19.7795942073923,-0.895791076677767));
#38375=CARTESIAN_POINT('Ctrl Pts',(4.82814550069091,19.7822187964435,-0.832879638048502));
#38376=CARTESIAN_POINT('Ctrl Pts',(4.97929162616721,19.7847061436466,-0.773703187802608));
#38377=CARTESIAN_POINT('Ctrl Pts',(5.11758620004362,19.7870683005815,-0.717955657569331));
#38378=CARTESIAN_POINT('Ctrl Pts',(5.24463111737929,19.7893154169154,-0.665388285718238));
#38379=CARTESIAN_POINT('Ctrl Pts',(5.3615187146248,19.7914528178618,-0.615872998117026));
#38380=CARTESIAN_POINT('Ctrl Pts',(5.46895006327484,19.7934813185126,-0.569387115888077));
#38381=CARTESIAN_POINT('Ctrl Pts',(5.56756311198424,19.7954023289415,-0.525890087244043));
#38382=CARTESIAN_POINT('Ctrl Pts',(5.65800137343926,19.797218820486,-0.485299481939044));
#38383=CARTESIAN_POINT('Ctrl Pts',(5.74091079063728,19.7989350271782,-0.447496453563895));
#38384=CARTESIAN_POINT('Ctrl Pts',(5.80284291081797,19.8002555833714,-0.418850315846327));
#38385=CARTESIAN_POINT('Ctrl Pts',(5.83721317807521,19.8010036894276,-0.402804474198884));
#38386=CARTESIAN_POINT('Ctrl Pts',(5.84634757864291,19.8012036144135,-0.398529569715516));
#38387=CARTESIAN_POINT('Ctrl Pts',(-5.81214048419312,19.9271886646867,-0.330203432875564));
#38388=CARTESIAN_POINT('Ctrl Pts',(-5.77669382802178,19.9264355395185,-0.3468342593928));
#38389=CARTESIAN_POINT('Ctrl Pts',(-5.65860909331072,19.9239803249271,-0.401708617535871));
#38390=CARTESIAN_POINT('Ctrl Pts',(-5.44840462341083,19.9198968585245,-0.496277870204232));
#38391=CARTESIAN_POINT('Ctrl Pts',(-5.17162939492092,19.9149425108579,-0.614820284163497));
#38392=CARTESIAN_POINT('Ctrl Pts',(-4.86534603855596,19.909880421409,-0.7387553338152));
#38393=CARTESIAN_POINT('Ctrl Pts',(-4.52588138424955,19.9047214712814,-0.867287833853044));
#38394=CARTESIAN_POINT('Ctrl Pts',(-4.14764846585593,19.8994886557635,-0.999606191879825));
#38395=CARTESIAN_POINT('Ctrl Pts',(-3.72427691756136,19.8942451763706,-1.13411062738609));
#38396=CARTESIAN_POINT('Ctrl Pts',(-3.25050020752433,19.8891247812009,-1.2675631879692));
#38397=CARTESIAN_POINT('Ctrl Pts',(-2.72227770248346,19.8843277548829,-1.39508118266476));
#38398=CARTESIAN_POINT('Ctrl Pts',(-2.13486068553421,19.8800965858062,-1.51060199964442));
#38399=CARTESIAN_POINT('Ctrl Pts',(-1.48765672123667,19.8767473168803,-1.60571548174355));
#38400=CARTESIAN_POINT('Ctrl Pts',(-0.800609992034415,19.8746447210675,
-1.669201892475));
#38401=CARTESIAN_POINT('Ctrl Pts',(-0.112656412660023,19.8739243721948,
-1.69383231167287));
#38402=CARTESIAN_POINT('Ctrl Pts',(0.532982300318684,19.8742602839387,-1.68192711531958));
#38403=CARTESIAN_POINT('Ctrl Pts',(1.11313112322414,19.8755170697086,-1.64255726795672));
#38404=CARTESIAN_POINT('Ctrl Pts',(1.62709005453795,19.877467053974,-1.58523245452894));
#38405=CARTESIAN_POINT('Ctrl Pts',(2.0850410197713,19.879899708692,-1.51643993262755));
#38406=CARTESIAN_POINT('Ctrl Pts',(2.49719897995038,19.8826728584564,-1.44015860157243));
#38407=CARTESIAN_POINT('Ctrl Pts',(2.86896944957029,19.8856601881407,-1.3596538028365));
#38408=CARTESIAN_POINT('Ctrl Pts',(3.20400785789159,19.8887529453858,-1.27761408943195));
#38409=CARTESIAN_POINT('Ctrl Pts',(3.50665331445631,19.8918777347858,-1.19576758536166));
#38410=CARTESIAN_POINT('Ctrl Pts',(3.78030901488711,19.8949775130325,-1.11543015088615));
#38411=CARTESIAN_POINT('Ctrl Pts',(4.02759771536219,19.8980059766931,-1.03765922725837));
#38412=CARTESIAN_POINT('Ctrl Pts',(4.25084657576043,19.9009285722717,-0.963229152083871));
#38413=CARTESIAN_POINT('Ctrl Pts',(4.45239467788257,19.9037239882921,-0.892594428082047));
#38414=CARTESIAN_POINT('Ctrl Pts',(4.63458237839232,19.906382426305,-0.825934929847175));
#38415=CARTESIAN_POINT('Ctrl Pts',(4.79971278148409,19.9089035013971,-0.763209477131803));
#38416=CARTESIAN_POINT('Ctrl Pts',(4.95001237258897,19.9112941678028,-0.704208461835124));
#38417=CARTESIAN_POINT('Ctrl Pts',(5.08753268224754,19.9135658129625,-0.648627094581878));
#38418=CARTESIAN_POINT('Ctrl Pts',(5.21386523151555,19.91572803623,-0.596217728895906));
#38419=CARTESIAN_POINT('Ctrl Pts',(5.33009497902457,19.9177858223623,-0.546853050922317));
#38420=CARTESIAN_POINT('Ctrl Pts',(5.43691796903193,19.9197398262928,-0.500510803643336));
#38421=CARTESIAN_POINT('Ctrl Pts',(5.53496769045484,19.9215912808168,-0.45715085370538));
#38422=CARTESIAN_POINT('Ctrl Pts',(5.62488345972163,19.9233429282228,-0.416691214874567));
#38423=CARTESIAN_POINT('Ctrl Pts',(5.70730743311051,19.9249987349898,-0.379013427036684));
#38424=CARTESIAN_POINT('Ctrl Pts',(5.76887172110402,19.9262734719378,-0.350464812380915));
#38425=CARTESIAN_POINT('Ctrl Pts',(5.80303600827932,19.9269958842689,-0.334474531192277));
#38426=CARTESIAN_POINT('Ctrl Pts',(5.81211556025371,19.9271889622373,-0.33021448364458));
#38427=CARTESIAN_POINT('Ctrl Pts',(-5.75637626238554,19.9977626186407,-0.213433499454596));
#38428=CARTESIAN_POINT('Ctrl Pts',(-5.7212417718798,19.9970541325727,-0.229942253987645));
#38429=CARTESIAN_POINT('Ctrl Pts',(-5.60419197539908,19.9947462888451,-0.284416335532265));
#38430=CARTESIAN_POINT('Ctrl Pts',(-5.39580847215891,19.9909174917254,-0.378306544937947));
#38431=CARTESIAN_POINT('Ctrl Pts',(-5.12142638369196,19.9862857505659,-0.496002143975811));
#38432=CARTESIAN_POINT('Ctrl Pts',(-4.8178161221067,19.9815661749843,-0.619044934882558));
#38433=CARTESIAN_POINT('Ctrl Pts',(-4.481360887937,19.9767689878634,-0.746638039711335));
#38434=CARTESIAN_POINT('Ctrl Pts',(-4.10654736969162,19.9719161036614,-0.87797019257089));
#38435=CARTESIAN_POINT('Ctrl Pts',(-3.68708854782038,19.9670669413926,-1.01144932738823));
#38436=CARTESIAN_POINT('Ctrl Pts',(-3.21779412718355,19.9623459099046,-1.1438596304457));
#38437=CARTESIAN_POINT('Ctrl Pts',(-2.69468813599392,19.9579377644809,-1.27035675133342));
#38438=CARTESIAN_POINT('Ctrl Pts',(-2.11308889877294,19.9540643078892,-1.38493050567701));
#38439=CARTESIAN_POINT('Ctrl Pts',(-1.47241765951857,19.9510122177396,-1.47924769932181));
#38440=CARTESIAN_POINT('Ctrl Pts',(-0.792400884528206,19.9491077370756,
-1.54219437673271));
#38441=CARTESIAN_POINT('Ctrl Pts',(-0.111506716483079,19.9484625525284,
-1.56661453768189));
#38442=CARTESIAN_POINT('Ctrl Pts',(0.527523869576598,19.948762395745,-1.55481091008629));
#38443=CARTESIAN_POINT('Ctrl Pts',(1.10171891950028,19.9498970382524,-1.51577665579069));
#38444=CARTESIAN_POINT('Ctrl Pts',(1.61044309412579,19.9516678974757,-1.45893642895713));
#38445=CARTESIAN_POINT('Ctrl Pts',(2.06377799643965,19.9538858627256,-1.39071843856522));
#38446=CARTESIAN_POINT('Ctrl Pts',(2.47183506989037,19.9564223371013,-1.3150651958254));
#38447=CARTESIAN_POINT('Ctrl Pts',(2.83995875855444,19.9591620892954,-1.23521318151454));
#38448=CARTESIAN_POINT('Ctrl Pts',(3.17175878038245,19.9620052196594,-1.15382839085906));
#38449=CARTESIAN_POINT('Ctrl Pts',(3.47152170739744,19.9648838525479,-1.07262526292338));
#38450=CARTESIAN_POINT('Ctrl Pts',(3.7426081303752,19.9677449142739,-0.992910001342112));
#38451=CARTESIAN_POINT('Ctrl Pts',(3.98760666100855,19.9705450649456,-0.915732946242152));
#38452=CARTESIAN_POINT('Ctrl Pts',(4.2088142491485,19.9732517129216,-0.841863855998557));
#38453=CARTESIAN_POINT('Ctrl Pts',(4.40854095596942,19.9758444804241,-0.77175523749468));
#38454=CARTESIAN_POINT('Ctrl Pts',(4.58909944991268,19.9783136764285,-0.70558703477212));
#38455=CARTESIAN_POINT('Ctrl Pts',(4.75276676013221,19.9806584016385,-0.643319687295874));
#38456=CARTESIAN_POINT('Ctrl Pts',(4.90174511909547,19.9828846554531,-0.584746306565457));
#38457=CARTESIAN_POINT('Ctrl Pts',(5.03806430897381,19.9850026522142,-0.529565368061844));
#38458=CARTESIAN_POINT('Ctrl Pts',(5.16329886931378,19.9870210227378,-0.477531953599395));
#38459=CARTESIAN_POINT('Ctrl Pts',(5.27852170418822,19.9889441474,-0.428520527235538));
#38460=CARTESIAN_POINT('Ctrl Pts',(5.38442057514526,19.9907723867053,-0.382509782879185));
#38461=CARTESIAN_POINT('Ctrl Pts',(5.48162162183854,19.9925066527352,-0.339460568099564));
#38462=CARTESIAN_POINT('Ctrl Pts',(5.57075720614196,19.9941492809222,-0.299292035622142));
#38463=CARTESIAN_POINT('Ctrl Pts',(5.6524630478063,19.995703765092,-0.261886921501083));
#38464=CARTESIAN_POINT('Ctrl Pts',(5.71348822196319,19.9969018117002,-0.233546326127602));
#38465=CARTESIAN_POINT('Ctrl Pts',(5.74735238456856,19.9975812837714,-0.21767305554885));
#38466=CARTESIAN_POINT('Ctrl Pts',(5.75635212916742,19.9977629229845,-0.213444206476439));
#38467=CARTESIAN_POINT('Ctrl Pts',(-5.6941765526172,19.9936699861522,-0.0798130175051694));
#38468=CARTESIAN_POINT('Ctrl Pts',(-5.65936703869485,19.9930119793506,-0.0961689593110878));
#38469=CARTESIAN_POINT('Ctrl Pts',(-5.54339967720871,19.9908709134695,-0.150138978145752));
#38470=CARTESIAN_POINT('Ctrl Pts',(-5.33694689369395,19.9873310897129,-0.243159156179306));
#38471=CARTESIAN_POINT('Ctrl Pts',(-5.06513642185539,19.9830664095691,-0.359752329638969));
#38472=CARTESIAN_POINT('Ctrl Pts',(-4.76442569368369,19.9787373930848,-0.48162174086261));
#38473=CARTESIAN_POINT('Ctrl Pts',(-4.4312589705187,19.9743535227251,-0.607970698079695));
#38474=CARTESIAN_POINT('Ctrl Pts',(-4.06020584530988,19.9699355319591,-0.737989586497756));
#38475=CARTESIAN_POINT('Ctrl Pts',(-3.64507557260789,19.9655385839926,-0.870097139656122));
#38476=CARTESIAN_POINT('Ctrl Pts',(-3.18076844297609,19.9612764317549,-1.0011075155669));
#38477=CARTESIAN_POINT('Ctrl Pts',(-2.66338764491666,19.957315974944,-1.12622841344135));
#38478=CARTESIAN_POINT('Ctrl Pts',(-2.08833386770721,19.9538550859021,-1.23952129169351));
#38479=CARTESIAN_POINT('Ctrl Pts',(-1.45505107682955,19.9511463329486,-1.33275847014169));
#38480=CARTESIAN_POINT('Ctrl Pts',(-0.783022235597851,19.9494710713447,
-1.39497134133894));
#38481=CARTESIAN_POINT('Ctrl Pts',(-0.110188903088729,19.9489129492212,
-1.41910487080894));
#38482=CARTESIAN_POINT('Ctrl Pts',(0.521281123261986,19.9491710061186,-1.40743979693122));
#38483=CARTESIAN_POINT('Ctrl Pts',(1.08869926737483,19.950164268464,-1.3688622122969));
#38484=CARTESIAN_POINT('Ctrl Pts',(1.59148386677679,19.9517279966345,-1.31268020141381));
#38485=CARTESIAN_POINT('Ctrl Pts',(2.03960018331289,19.9536979748251,-1.24524120709786));
#38486=CARTESIAN_POINT('Ctrl Pts',(2.44303760720881,19.9559613841007,-1.17043793420388));
#38487=CARTESIAN_POINT('Ctrl Pts',(2.80706804720489,19.9584158367489,-1.09146748105984));
#38488=CARTESIAN_POINT('Ctrl Pts',(3.13524621669758,19.9609716532087,-1.01096521360529));
#38489=CARTESIAN_POINT('Ctrl Pts',(3.4317966606742,19.9635673037228,-0.930627086505941));
#38490=CARTESIAN_POINT('Ctrl Pts',(3.70002963338188,19.9661542544967,-0.851746359874953));
#38491=CARTESIAN_POINT('Ctrl Pts',(3.94249333603436,19.9686925339578,-0.775363949415814));
#38492=CARTESIAN_POINT('Ctrl Pts',(4.16144912038774,19.9711517597429,-0.702243626244488));
#38493=CARTESIAN_POINT('Ctrl Pts',(4.35917319283947,19.9735125811614,-0.632835389747046));
#38494=CARTESIAN_POINT('Ctrl Pts',(4.53794624447846,19.975765389239,-0.567319428639144));
#38495=CARTESIAN_POINT('Ctrl Pts',(4.70001547858408,19.977908659644,-0.505658465160906));
#38496=CARTESIAN_POINT('Ctrl Pts',(4.84755564240826,19.9799472694527,-0.447649311946973));
#38497=CARTESIAN_POINT('Ctrl Pts',(4.9825720787926,19.9818900683868,-0.392994812681759));
#38498=CARTESIAN_POINT('Ctrl Pts',(5.10662033523709,19.9837445626203,-0.341453653044119));
#38499=CARTESIAN_POINT('Ctrl Pts',(5.22075984776193,19.985514427777,-0.292902611947154));
#38500=CARTESIAN_POINT('Ctrl Pts',(5.32566908184073,19.9871996753446,-0.247321606171754));
#38501=CARTESIAN_POINT('Ctrl Pts',(5.42196592776049,19.9888008400244,-0.204672761471427));
#38502=CARTESIAN_POINT('Ctrl Pts',(5.51027491707437,19.9903197826892,-0.164876756608036));
#38503=CARTESIAN_POINT('Ctrl Pts',(5.59122442533177,19.9917594473338,-0.127818010509195));
#38504=CARTESIAN_POINT('Ctrl Pts',(5.65168521434086,19.9928706910276,-0.0997396726106242));
#38505=CARTESIAN_POINT('Ctrl Pts',(5.68523639400912,19.9935015994509,-0.0840132164337404));
#38506=CARTESIAN_POINT('Ctrl Pts',(5.69415298771922,19.9936703044405,-0.0798234694406676));
#38507=CARTESIAN_POINT('',(5.73644274981185,19.8089495938061,-0.442545696631703));
#38508=CARTESIAN_POINT('Origin',(5.599999999773,19.5919343767575,-0.135488061233534));
#38509=CARTESIAN_POINT('Ctrl Pts',(-5.73644387793648,19.8089519016389,-0.442549068206594));
#38510=CARTESIAN_POINT('Ctrl Pts',(-5.66411038116652,19.8074370301077,-0.475761118065655));
#38511=CARTESIAN_POINT('Ctrl Pts',(-5.58548128839259,19.8058476858851,-0.511218926975151));
#38512=CARTESIAN_POINT('Ctrl Pts',(-5.50055659799522,19.8041980383931,-0.548567703824968));
#38513=CARTESIAN_POINT('Ctrl Pts',(-5.41741953789741,19.8025831153119,-0.585130304065416));
#38514=CARTESIAN_POINT('Ctrl Pts',(-5.32824913024332,19.8009104082698,-0.623504915458204));
#38515=CARTESIAN_POINT('Ctrl Pts',(-5.23304537351361,19.7991952410186,-0.663306060482758));
#38516=CARTESIAN_POINT('Ctrl Pts',(-5.13477098041616,19.7974247539447,-0.704390924213256));
#38517=CARTESIAN_POINT('Ctrl Pts',(-5.03006777092705,19.7956090117501,-0.746996132649766));
#38518=CARTESIAN_POINT('Ctrl Pts',(-4.91893574337511,19.7937671147615,-0.790639464683737));
#38519=CARTESIAN_POINT('Ctrl Pts',(-4.80780371582317,19.7919252177729,-0.834282796717708));
#38520=CARTESIAN_POINT('Ctrl Pts',(-4.69024287020841,19.7900571657752,-0.878964256165504));
#38521=CARTESIAN_POINT('Ctrl Pts',(-4.56625320485967,19.7881843424896,-0.924142417267869));
#38522=CARTESIAN_POINT('Ctrl Pts',(-4.44622763757178,19.7863713956069,-0.967876178465492));
#38523=CARTESIAN_POINT('Ctrl Pts',(-4.32017775547907,19.7845539889092,-1.01207510056595));
#38524=CARTESIAN_POINT('Ctrl Pts',(-4.18810355858154,19.7827535621543,-1.05619514264032));
#38525=CARTESIAN_POINT('Ctrl Pts',(-4.05161769976433,19.7808929959147,-1.10178892231133));
#38526=CARTESIAN_POINT('Ctrl Pts',(-3.90869834525198,19.7790505502845,-1.14729878417172));
#38527=CARTESIAN_POINT('Ctrl Pts',(-3.75934549504447,19.7772521459655,-1.19206586482418));
#38528=CARTESIAN_POINT('Ctrl Pts',(-3.60999264483696,19.7754537416466,-1.23683294547664));
#38529=CARTESIAN_POINT('Ctrl Pts',(-3.45420629893429,19.7736993780091,-1.28085725073673));
#38530=CARTESIAN_POINT('Ctrl Pts',(-3.29198645733648,19.7720172810933,-1.32342041175998));
#38531=CARTESIAN_POINT('Ctrl Pts',(-3.2117504477056,19.7711852944324,-1.34447269589578));
#38532=CARTESIAN_POINT('Ctrl Pts',(-3.12994053610347,19.7703710227783,-1.36516660608575));
#38533=CARTESIAN_POINT('Ctrl Pts',(-3.04655672721603,19.7695781056132,-1.38540981940204));
#38534=CARTESIAN_POINT('Ctrl Pts',(-3.00486482277231,19.7691816470307,-1.39553142606018));
#38535=CARTESIAN_POINT('Ctrl Pts',(-2.96277943528041,19.7687905034135,-1.40554032113933));
#38536=CARTESIAN_POINT('Ctrl Pts',(-2.92030057599748,19.7684051737507,-1.41542460742403));
#38537=CARTESIAN_POINT('Ctrl Pts',(-2.89906114635602,19.7682125089192,-1.42036675056638));
#38538=CARTESIAN_POINT('Ctrl Pts',(-2.87772334819987,19.7680212960993,-1.42527773918684));
#38539=CARTESIAN_POINT('Ctrl Pts',(-2.85628718138127,19.7678315939691,-1.43015606844165));
#38540=CARTESIAN_POINT('Ctrl Pts',(-2.84556909797198,19.767736742904,-1.43259523306906));
#38541=CARTESIAN_POINT('Ctrl Pts',(-2.83482642236462,19.7676422694187,-1.43502623270797));
#38542=CARTESIAN_POINT('Ctrl Pts',(-2.82405915455031,19.7675481809229,-1.43744887792669));
#38543=CARTESIAN_POINT('Ctrl Pts',(-2.81867552064316,19.767501136675,-1.43866020053605));
#38544=CARTESIAN_POINT('Ctrl Pts',(-2.81328573868226,19.7674541886688,-1.43986943453117));
#38545=CARTESIAN_POINT('Ctrl Pts',(-2.80788980866765,19.767407337837,-1.44107655614885));
#38546=CARTESIAN_POINT('Ctrl Pts',(-2.80249387865305,19.7673604870052,-1.44228367776654));
#38547=CARTESIAN_POINT('Ctrl Pts',(-2.79531884999955,19.7672984384957,-1.44388301861298));
#38548=CARTESIAN_POINT('Ctrl Pts',(-2.79168357445871,19.7672670777872,-1.44469156006093));
#38549=CARTESIAN_POINT('Ctrl Pts',(-2.04577401164782,19.7608322829147,-1.61059337167776));
#38550=CARTESIAN_POINT('Ctrl Pts',(-1.29987675980753,19.7571533928382,-1.7099242373575));
#38551=CARTESIAN_POINT('Ctrl Pts',(-0.553962218243579,19.756216688384,-1.7426513167991));
#38552=CARTESIAN_POINT('Ctrl Pts',(-0.369309354733381,19.755984805038,-1.75075298072503));
#38553=CARTESIAN_POINT('Ctrl Pts',(-0.18465543167186,19.7559210302059,-1.75477277944571));
#38554=CARTESIAN_POINT('Ctrl Pts',(-6.23933593455217E-13,19.7560252781079,
-1.75470973806164));
#38555=CARTESIAN_POINT('Ctrl Pts',(6.9346062000257E-5,19.7560253172575,
-1.75470971438689));
#38556=CARTESIAN_POINT('Ctrl Pts',(0.000138692124836583,19.7560253564308,
-1.75470969013632));
#38557=CARTESIAN_POINT('Ctrl Pts',(0.000208038187885564,19.7560253956277,
-1.75470966530994));
#38558=CARTESIAN_POINT('Ctrl Pts',(0.465532887800232,19.7562884145047,-1.75454307569928));
#38559=CARTESIAN_POINT('Ctrl Pts',(0.93085773639074,19.7573599747505,-1.72860446382034));
#38560=CARTESIAN_POINT('Ctrl Pts',(1.39618258395941,19.7592421679926,-1.67690533849036));
#38561=CARTESIAN_POINT('Ctrl Pts',(1.62884500774375,19.7601832646136,-1.65105577582537));
#38562=CARTESIAN_POINT('Ctrl Pts',(1.86150743137938,19.761326885799,-1.6187664128127));
#38563=CARTESIAN_POINT('Ctrl Pts',(2.09416985350423,19.7626724911624,-1.58004068048147));
#38564=CARTESIAN_POINT('Ctrl Pts',(2.21050106456666,19.7633452938441,-1.56067781431586));
#38565=CARTESIAN_POINT('Ctrl Pts',(2.32683227716806,19.764068599484,-1.53970586697001));
#38566=CARTESIAN_POINT('Ctrl Pts',(2.44316348898894,19.7648422734326,-1.51712540449519));
#38567=CARTESIAN_POINT('Ctrl Pts',(2.50132909489938,19.7652291104069,-1.50583517325778));
#38568=CARTESIAN_POINT('Ctrl Pts',(2.55949470071762,19.7656285398986,-1.49414281395364));
#38569=CARTESIAN_POINT('Ctrl Pts',(2.61766030646164,19.766040544681,-1.48204840355164));
#38570=CARTESIAN_POINT('Ctrl Pts',(2.64674310933365,19.7662465470722,-1.47600119835064));
#38571=CARTESIAN_POINT('Ctrl Pts',(2.67582591219613,19.7664556933134,-1.46985348041873));
#38572=CARTESIAN_POINT('Ctrl Pts',(2.70490871505082,19.7666679810471,-1.46360525988021));
#38573=CARTESIAN_POINT('Ctrl Pts',(2.7321738427271,19.7668670007974,-1.45774755312535));
#38574=CARTESIAN_POINT('Ctrl Pts',(2.75943897039682,19.7670687816261,-1.45180151400297));
#38575=CARTESIAN_POINT('Ctrl Pts',(2.78670409806629,19.7672733215177,-1.4457671511001));
#38576=CARTESIAN_POINT('Ctrl Pts',(2.78852177324425,19.7672869575105,-1.44536486023991));
#38577=CARTESIAN_POINT('Ctrl Pts',(2.79172178017481,19.7673109945109,-1.44465563983108));
#38578=CARTESIAN_POINT('Ctrl Pts',(2.79215712359993,19.7673142662813,-1.44455910087302));
#38579=CARTESIAN_POINT('Ctrl Pts',(2.80635022699111,19.7674209328201,-1.44141172954727));
#38580=CARTESIAN_POINT('Ctrl Pts',(2.82656863123274,19.7675848277377,-1.43690147673273));
#38581=CARTESIAN_POINT('Ctrl Pts',(2.85281233632482,19.7678094196818,-1.43094097946311));
#38582=CARTESIAN_POINT('Ctrl Pts',(2.87905633539835,19.7680340141419,-1.42498041542411));
#38583=CARTESIAN_POINT('Ctrl Pts',(2.91132577031368,19.7683193068042,-1.4175695743538));
#38584=CARTESIAN_POINT('Ctrl Pts',(2.9496206410708,19.7686708437388,-1.4085690016783));
#38585=CARTESIAN_POINT('Ctrl Pts',(2.98791596514066,19.7690223848347,-1.39956832245917));
#38586=CARTESIAN_POINT('Ctrl Pts',(3.03223686770447,19.7694401714784,-1.38897787390266));
#38587=CARTESIAN_POINT('Ctrl Pts',(3.08258334876223,19.7699318308584,-1.37660610821271));
#38588=CARTESIAN_POINT('Ctrl Pts',(3.13293081631026,19.7704234998721,-1.36423410011007));
#38589=CARTESIAN_POINT('Ctrl Pts',(3.18930409848524,19.7709890441134,-1.35008070502378));
#38590=CARTESIAN_POINT('Ctrl Pts',(3.25170319528717,19.771638177437,-1.33390227483369));
#38591=CARTESIAN_POINT('Ctrl Pts',(3.31410299699454,19.7722873180937,-1.31772366188033));
#38592=CARTESIAN_POINT('Ctrl Pts',(3.38252874947358,19.7730200492131,-1.29951996794108));
#38593=CARTESIAN_POINT('Ctrl Pts',(3.45698045272428,19.7738481780564,-1.27899544831037));
#38594=CARTESIAN_POINT('Ctrl Pts',(3.53143357438562,19.7746763226767,-1.25847053765842));
#38595=CARTESIAN_POINT('Ctrl Pts',(3.61191287642663,19.7755998680385,-1.23562471280952));
#38596=CARTESIAN_POINT('Ctrl Pts',(3.69841835884734,19.7766327236699,-1.21011012356596));
#38597=CARTESIAN_POINT('Ctrl Pts',(3.77371782358943,19.7775317820188,-1.18790072296623));
#38598=CARTESIAN_POINT('Ctrl Pts',(3.85358331706806,19.7785136964691,-1.16366840616151));
#38599=CARTESIAN_POINT('Ctrl Pts',(3.93801483928324,19.779588943194,-1.13715162237394));
#38600=CARTESIAN_POINT('Ctrl Pts',(3.98561399760912,19.7801951248399,-1.12220250672752));
#38601=CARTESIAN_POINT('Ctrl Pts',(4.03466435815191,19.7808309918418,-1.10652678805407));
#38602=CARTESIAN_POINT('Ctrl Pts',(4.08516592649798,19.781498604142,-1.09007340331406));
#38603=CARTESIAN_POINT('Ctrl Pts',(4.11041671067101,19.7818324102921,-1.08184671094406));
#38604=CARTESIAN_POINT('Ctrl Pts',(4.13603028724608,19.7821741330792,-1.0734255721268));
#38605=CARTESIAN_POINT('Ctrl Pts',(4.16200666832599,19.7825240675577,-1.06480330014664));
#38606=CARTESIAN_POINT('Ctrl Pts',(4.17499485886595,19.782699034797,-1.06049216415656));
#38607=CARTESIAN_POINT('Ctrl Pts',(4.1880737499445,19.7828760537271,-1.05613074299689));
#38608=CARTESIAN_POINT('Ctrl Pts',(4.20124334141254,19.7830551581622,-1.05171818614679));
#38609=CARTESIAN_POINT('Ctrl Pts',(4.20782813714656,19.7831447103797,-1.04951190772174));
#38610=CARTESIAN_POINT('Ctrl Pts',(4.21443560793993,19.7832347838967,-1.04729284525787));
#38611=CARTESIAN_POINT('Ctrl Pts',(4.22106575379413,19.7833253830315,-1.04506089129743));
#38612=CARTESIAN_POINT('Ctrl Pts',(4.22769589964832,19.7834159821662,-1.04282893733699));
#38613=CARTESIAN_POINT('Ctrl Pts',(4.23593743769457,19.7835289199598,-1.04004674200915));
#38614=CARTESIAN_POINT('Ctrl Pts',(4.24102421646306,19.7835987614664,-1.03832624687006));
#38615=CARTESIAN_POINT('Ctrl Pts',(4.3703949931502,19.7853750230971,-0.994569322780967));
#38616=CARTESIAN_POINT('Ctrl Pts',(4.49373991369497,19.7871644677347,-0.950843620817392));
#38617=CARTESIAN_POINT('Ctrl Pts',(4.61105897939592,19.7889461132073,-0.907681610185909));
#38618=CARTESIAN_POINT('Ctrl Pts',(4.72934236291549,19.7907424031239,-0.864164824346399));
#38619=CARTESIAN_POINT('Ctrl Pts',(4.84150042403069,19.7925307626914,-0.821221103354181));
#38620=CARTESIAN_POINT('Ctrl Pts',(4.94753316407235,19.7942917588281,-0.779342573722851));
#38621=CARTESIAN_POINT('Ctrl Pts',(5.05275827019582,19.7960393417472,-0.737783025954676));
#38622=CARTESIAN_POINT('Ctrl Pts',(5.15195101100168,19.7977599793199,-0.697272434259096));
#38623=CARTESIAN_POINT('Ctrl Pts',(5.24511138779057,19.7994366989643,-0.658239440062828));
#38624=CARTESIAN_POINT('Ctrl Pts',(5.33934431488943,19.80113272259,-0.618757061144568));
#38625=CARTESIAN_POINT('Ctrl Pts',(5.42740517784177,19.8027838073779,-0.580786598554457));
#38626=CARTESIAN_POINT('Ctrl Pts',(5.50929397799366,19.8043744792903,-0.544717460517054));
#38627=CARTESIAN_POINT('Ctrl Pts',(5.59118277814556,19.8059651512028,-0.508648322479651));
#38628=CARTESIAN_POINT('Ctrl Pts',(5.66689951549702,19.8074954102507,-0.474480506728332));
#38629=CARTESIAN_POINT('Ctrl Pts',(5.73644419139414,19.8089518848421,-0.442548940794832));
#38630=CARTESIAN_POINT('Origin',(5.6,19.5919343769583,-0.135488060981343));
#38631=CARTESIAN_POINT('Origin',(5.59997427808526,19.5919309020823,-0.135464036534198));
#38632=CARTESIAN_POINT('Ctrl Pts',(5.71189864452985,10.3747304895651,-1.73098436839218));
#38633=CARTESIAN_POINT('Ctrl Pts',(5.71686764344326,10.3731922894021,-1.72895290465319));
#38634=CARTESIAN_POINT('Ctrl Pts',(5.76414615685762,10.3586634212538,-1.70873769602088));
#38635=CARTESIAN_POINT('Ctrl Pts',(5.84912002164699,10.334482886934,-1.65630729766632));
#38636=CARTESIAN_POINT('Ctrl Pts',(5.94753982152578,10.3114454163772,-1.5531434815364));
#38637=CARTESIAN_POINT('Ctrl Pts',(6.01568051672699,10.3011442171297,-1.43300892716969));
#38638=CARTESIAN_POINT('Ctrl Pts',(6.04717587912082,10.3030528288475,-1.32055362605887));
#38639=CARTESIAN_POINT('Ctrl Pts',(6.05143244177369,10.3095932145156,-1.25273304586632));
#38640=CARTESIAN_POINT('Ctrl Pts',(6.05078104094871,10.3130207230613,-1.22619796391761));
#38641=CARTESIAN_POINT('Ctrl Pts',(5.59579998485702,10.091096172154,-1.65481746119893));
#38642=CARTESIAN_POINT('Ctrl Pts',(5.60043595614829,10.0896504255744,-1.65294937270293));
#38643=CARTESIAN_POINT('Ctrl Pts',(5.64455259774951,10.0759868560455,-1.63435926048869));
#38644=CARTESIAN_POINT('Ctrl Pts',(5.72395137359632,10.0531092099547,-1.58612351386667));
#38645=CARTESIAN_POINT('Ctrl Pts',(5.81591850580226,10.0310626434678,-1.49126508712223));
#38646=CARTESIAN_POINT('Ctrl Pts',(5.87943865664269,10.0209345533178,-1.38113253481707));
#38647=CARTESIAN_POINT('Ctrl Pts',(5.90862955872158,10.022319989054,-1.27866217141058));
#38648=CARTESIAN_POINT('Ctrl Pts',(5.91253312848719,10.0281804213171,-1.2173831667632));
#38649=CARTESIAN_POINT('Ctrl Pts',(5.91193519380811,10.0312728279379,-1.19350825632173));
#38650=CARTESIAN_POINT('Ctrl Pts',(5.57863052428272,9.8189813716046,-1.81415344748554));
#38651=CARTESIAN_POINT('Ctrl Pts',(5.58522332651264,9.8169636961234,-1.81151876117067));
#38652=CARTESIAN_POINT('Ctrl Pts',(5.64790096319949,9.79793300371442,-1.78533019096301));
#38653=CARTESIAN_POINT('Ctrl Pts',(5.7597437862497,9.76669738257529,-1.71797544780278));
#38654=CARTESIAN_POINT('Ctrl Pts',(5.88924968067551,9.73729923170353,-1.58603258316671));
#38655=CARTESIAN_POINT('Ctrl Pts',(5.98006036132214,9.72422746393119,-1.43101993105616));
#38656=CARTESIAN_POINT('Ctrl Pts',(6.02329964904305,9.72688955971414,-1.28255723102518));
#38657=CARTESIAN_POINT('Ctrl Pts',(6.02945491177813,9.73581061263325,-1.19002012260145));
#38658=CARTESIAN_POINT('Ctrl Pts',(6.02851709775331,9.74055796418653,-1.15322141602788));
#38659=CARTESIAN_POINT('Ctrl Pts',(5.6716461590008,9.73678026104202,-2.10453384239488));
#38660=CARTESIAN_POINT('Ctrl Pts',(5.68120278004111,9.73390122266715,-2.10070515593161));
#38661=CARTESIAN_POINT('Ctrl Pts',(5.77199595282922,9.70678959567008,-2.06267601536369));
#38662=CARTESIAN_POINT('Ctrl Pts',(5.93303210065318,9.66301450628333,-1.96542277239424));
#38663=CARTESIAN_POINT('Ctrl Pts',(6.11945830548874,9.62274187697619,-1.775317678271));
#38664=CARTESIAN_POINT('Ctrl Pts',(6.25157930475856,9.60553947784097,-1.54996558636508));
#38665=CARTESIAN_POINT('Ctrl Pts',(6.31600990124635,9.61044110901839,-1.32968520371137));
#38666=CARTESIAN_POINT('Ctrl Pts',(6.32554536478181,9.62415685682377,-1.18858268459059));
#38667=CARTESIAN_POINT('Ctrl Pts',(6.32409714600594,9.63146424160204,-1.13174887283082));
#38668=CARTESIAN_POINT('',(5.99998739574847,10.093342129965,-1.21103206229897));
#38669=CARTESIAN_POINT('',(5.99999998791408,9.6543882121161,-1.86247524004434));
#38670=CARTESIAN_POINT('Ctrl Pts',(5.99998739574847,10.093342129965,-1.21103206229897));
#38671=CARTESIAN_POINT('Ctrl Pts',(5.99998525070341,10.0742059844227,-1.2256251864801));
#38672=CARTESIAN_POINT('Ctrl Pts',(5.99998676083935,10.0554326526012,-1.24054794704701));
#38673=CARTESIAN_POINT('Ctrl Pts',(5.99999979829476,10.03713808821,-1.25580697991203));
#38674=CARTESIAN_POINT('Ctrl Pts',(6.00000674487255,10.02739043343,-1.26393725191334));
#38675=CARTESIAN_POINT('Ctrl Pts',(6.00001622859838,10.0177786906484,-1.27216235989735));
#38676=CARTESIAN_POINT('Ctrl Pts',(6.00002591477378,10.0083195677745,-1.28047856190009));
#38677=CARTESIAN_POINT('Ctrl Pts',(6.00004505453792,9.98962845664022,-1.29691127536836));
#38678=CARTESIAN_POINT('Ctrl Pts',(6.00006657199182,9.97153445157826,-1.31370242007807));
#38679=CARTESIAN_POINT('Ctrl Pts',(6.00008776273575,9.95414192720689,-1.33079292037839));
#38680=CARTESIAN_POINT('Ctrl Pts',(6.00010095957137,9.94331048656118,-1.3414362712604));
#38681=CARTESIAN_POINT('Ctrl Pts',(6.00011344452304,9.93275077675863,-1.35219475564079));
#38682=CARTESIAN_POINT('Ctrl Pts',(6.00012222699497,9.92248320775588,-1.36304548041424));
#38683=CARTESIAN_POINT('Ctrl Pts',(6.00013667465114,9.90559248408776,-1.38089552784979));
#38684=CARTESIAN_POINT('Ctrl Pts',(6.00013999561394,9.88949456201145,-1.39899690728196));
#38685=CARTESIAN_POINT('Ctrl Pts',(6.00012430276381,9.87425199476169,-1.41721620450256));
#38686=CARTESIAN_POINT('Ctrl Pts',(6.00011929886963,9.86939167985008,-1.42302569318705));
#38687=CARTESIAN_POINT('Ctrl Pts',(6.0001124735993,9.86461804279409,-1.42884691741494));
#38688=CARTESIAN_POINT('Ctrl Pts',(6.00010395684403,9.85993227951363,-1.43467492541273));
#38689=CARTESIAN_POINT('Ctrl Pts',(6.00009905090812,9.85723312312927,-1.43803205296138));
#38690=CARTESIAN_POINT('Ctrl Pts',(6.00009358871496,9.85456311662419,-1.44139142719417));
#38691=CARTESIAN_POINT('Ctrl Pts',(6.0000876867648,9.85192240584083,-1.44475212813161));
#38692=CARTESIAN_POINT('Ctrl Pts',(6.00006914832814,9.84362774927567,-1.4553083239369));
#38693=CARTESIAN_POINT('Ctrl Pts',(6.00005144090386,9.83550486511725,-1.46601891242109));
#38694=CARTESIAN_POINT('Ctrl Pts',(6.00003089267563,9.82769828562318,-1.47670035842532));
#38695=CARTESIAN_POINT('Ctrl Pts',(6.0000101584876,9.81982105722095,-1.48747847064532));
#38696=CARTESIAN_POINT('Ctrl Pts',(5.99998607983893,9.81226624915332,-1.49822652985124));
#38697=CARTESIAN_POINT('Ctrl Pts',(5.99996800047488,9.80514747283832,-1.50871702540345));
#38698=CARTESIAN_POINT('Ctrl Pts',(5.99995733483965,9.80094786320285,-1.51490572754164));
#38699=CARTESIAN_POINT('Ctrl Pts',(5.99994905280315,9.79689929622093,-1.52100407183462));
#38700=CARTESIAN_POINT('Ctrl Pts',(5.99994795704476,9.79301903904449,-1.52696018892455));
#38701=CARTESIAN_POINT('Ctrl Pts',(5.99994404418047,9.77916295551462,-1.54822899976853));
#38702=CARTESIAN_POINT('Ctrl Pts',(5.99996395741825,9.76602634289345,-1.57000915494076));
#38703=CARTESIAN_POINT('Ctrl Pts',(5.99998991543438,9.75374722793985,-1.59221159742656));
#38704=CARTESIAN_POINT('Ctrl Pts',(6.00001572479601,9.74153843214226,-1.61428689255501));
#38705=CARTESIAN_POINT('Ctrl Pts',(6.0000467928305,9.73017813382453,-1.6367791365723));
#38706=CARTESIAN_POINT('Ctrl Pts',(6.00006725086747,9.71977349236808,-1.65955800898032));
#38707=CARTESIAN_POINT('Ctrl Pts',(6.00007042537936,9.71815898468138,-1.66309264924169));
#38708=CARTESIAN_POINT('Ctrl Pts',(6.00007335936769,9.71656741865602,-1.66663411695046));
#38709=CARTESIAN_POINT('Ctrl Pts',(6.00007601305726,9.71499911544098,-1.67018184719024));
#38710=CARTESIAN_POINT('Ctrl Pts',(6.00009313187098,9.70488207278654,-1.69306807086057));
#38711=CARTESIAN_POINT('Ctrl Pts',(6.00009752578096,9.69573653071054,-1.71621725348646));
#38712=CARTESIAN_POINT('Ctrl Pts',(6.00008809970652,9.68762372022529,-1.739465193567));
#38713=CARTESIAN_POINT('Ctrl Pts',(6.00007855620972,9.67940984694546,-1.76300273757664));
#38714=CARTESIAN_POINT('Ctrl Pts',(6.00005445424126,9.67225489482556,-1.78664049911191));
#38715=CARTESIAN_POINT('Ctrl Pts',(6.00003199298379,9.66617590604954,-1.81018726837208));
#38716=CARTESIAN_POINT('Ctrl Pts',(6.00001529302277,9.66165617354125,-1.82769430817947));
#38717=CARTESIAN_POINT('Ctrl Pts',(5.99999988409118,9.65773020436411,-1.84515053404935));
#38718=CARTESIAN_POINT('Ctrl Pts',(5.99999988834942,9.65438801533234,-1.86247520208183));
#38719=CARTESIAN_POINT('',(5.72001530599109,9.72697688177551,-2.05943446844682));
#38720=CARTESIAN_POINT('Ctrl Pts',(5.72001583931905,9.72697824478347,-2.05943475704983));
#38721=CARTESIAN_POINT('Ctrl Pts',(5.77262443161298,9.71167221606504,-2.03450172317382));
#38722=CARTESIAN_POINT('Ctrl Pts',(5.82215801015693,9.69806914525657,-2.00535807896891));
#38723=CARTESIAN_POINT('Ctrl Pts',(5.86878812167555,9.68600522339526,-1.97246301336546));
#38724=CARTESIAN_POINT('Ctrl Pts',(5.91541823319418,9.67394130153395,-1.93956794776201));
#38725=CARTESIAN_POINT('Ctrl Pts',(5.95914511084698,9.66341708212426,-1.90292156494207));
#38726=CARTESIAN_POINT('Ctrl Pts',(6.00000005305837,9.65438841513202,-1.86247527920915));
#38727=CARTESIAN_POINT('',(5.732785087834,10.3449543305438,-1.7128937574831));
#38728=CARTESIAN_POINT('Origin',(5.89877349632372,10.183812103656,-2.15616649229544));
#38729=CARTESIAN_POINT('Ctrl Pts',(5.73278241138339,10.3449569278259,-1.71288661549559));
#38730=CARTESIAN_POINT('Ctrl Pts',(5.74767875123649,10.3336216280175,-1.70318199341943));
#38731=CARTESIAN_POINT('Ctrl Pts',(5.76173634509441,10.322835658242,-1.69290604950805));
#38732=CARTESIAN_POINT('Ctrl Pts',(5.77495203195241,10.3125930760254,-1.68228739492388));
#38733=CARTESIAN_POINT('Ctrl Pts',(5.78903167351962,10.301680901132,-1.67097456252422));
#38734=CARTESIAN_POINT('Ctrl Pts',(5.80215588058894,10.291385530781,-1.65927245019434));
#38735=CARTESIAN_POINT('Ctrl Pts',(5.81434894340356,10.2816926135053,-1.64740640683436));
#38736=CARTESIAN_POINT('Ctrl Pts',(5.81704664373936,10.2795480673329,-1.64478105915564));
#38737=CARTESIAN_POINT('Ctrl Pts',(5.81969886131872,10.2774329841764,-1.64214751019764));
#38738=CARTESIAN_POINT('Ctrl Pts',(5.82230601802282,10.2753471622135,-1.63950791362413));
#38739=CARTESIAN_POINT('Ctrl Pts',(5.8343566194193,10.2657062346013,-1.6273073711309));
#38740=CARTESIAN_POINT('Ctrl Pts',(5.84544364851837,10.2566906065921,-1.61498183373302));
#38741=CARTESIAN_POINT('Ctrl Pts',(5.85563660028135,10.24826867085,-1.60274257496124));
#38742=CARTESIAN_POINT('Ctrl Pts',(5.85625540711629,10.2477573811351,-1.60199953828661));
#38743=CARTESIAN_POINT('Ctrl Pts',(5.85687092211076,10.247248278839,-1.60125680431862));
#38744=CARTESIAN_POINT('Ctrl Pts',(5.85748316207662,10.2467413566176,-1.60051441457763));
#38745=CARTESIAN_POINT('Ctrl Pts',(5.86845374327555,10.2376579388377,-1.58721171075426));
#38746=CARTESIAN_POINT('Ctrl Pts',(5.87837194703487,10.2292747699409,-1.57402408876206));
#38747=CARTESIAN_POINT('Ctrl Pts',(5.88734076941703,10.221548069533,-1.56115987641525));
#38748=CARTESIAN_POINT('Ctrl Pts',(5.89145118167163,10.2180069219118,-1.55526420652425));
#38749=CARTESIAN_POINT('Ctrl Pts',(5.8953623376495,10.2146036181259,-1.54943570552396));
#38750=CARTESIAN_POINT('Ctrl Pts',(5.89908478287728,10.2113337664291,-1.5436909432781));
#38751=CARTESIAN_POINT('Ctrl Pts',(5.90118655203684,10.2094875408886,-1.54044733232387));
#38752=CARTESIAN_POINT('Ctrl Pts',(5.9032281669301,10.2076838576228,-1.53723038063642));
#38753=CARTESIAN_POINT('Ctrl Pts',(5.90521156641127,10.2059219134952,-1.5340428035946));
#38754=CARTESIAN_POINT('Ctrl Pts',(5.90881699114517,10.2027190504322,-1.52824842418851));
#38755=CARTESIAN_POINT('Ctrl Pts',(5.91223007754269,10.1996540965837,-1.52255125712056));
#38756=CARTESIAN_POINT('Ctrl Pts',(5.91546374346187,10.1967216968648,-1.51696747377376));
#38757=CARTESIAN_POINT('Ctrl Pts',(5.91797002104723,10.1944489179598,-1.51263971964165));
#38758=CARTESIAN_POINT('Ctrl Pts',(5.92036844691872,10.1922557983517,-1.50838013033203));
#38759=CARTESIAN_POINT('Ctrl Pts',(5.92266499899361,10.1901398681883,-1.50419520066658));
#38760=CARTESIAN_POINT('Ctrl Pts',(5.92381327503106,10.1890819031065,-1.50210273583385));
#38761=CARTESIAN_POINT('Ctrl Pts',(5.9249360757642,10.188043237144,-1.5000289313888));
#38762=CARTESIAN_POINT('Ctrl Pts',(5.92603412788109,10.1870235727388,-1.49797454672763));
#38763=CARTESIAN_POINT('Ctrl Pts',(5.92680721492419,10.1863056748105,-1.49652815075182));
#38764=CARTESIAN_POINT('Ctrl Pts',(5.92725985652953,10.1858838464094,-1.49567455154667));
#38765=CARTESIAN_POINT('Ctrl Pts',(5.92804436251635,10.1851520674593,-1.49418301711905));
#38766=CARTESIAN_POINT('Ctrl Pts',(5.92837412751263,10.1848444661321,-1.49355605460602));
#38767=CARTESIAN_POINT('Ctrl Pts',(5.92876221211849,10.1844822288943,-1.49281615753072));
#38768=CARTESIAN_POINT('Ctrl Pts',(5.92925474683439,10.1840212904741,-1.49187038511312));
#38769=CARTESIAN_POINT('Ctrl Pts',(5.939199111107,10.1747148610788,-1.47277507033431));
#38770=CARTESIAN_POINT('Ctrl Pts',(5.94793617260916,10.1661689170949,-1.4536541603137));
#38771=CARTESIAN_POINT('Ctrl Pts',(5.95554256935783,10.1583490236111,-1.43472083832225));
#38772=CARTESIAN_POINT('Ctrl Pts',(5.95842928679405,10.1553812816414,-1.427535418928));
#38773=CARTESIAN_POINT('Ctrl Pts',(5.96115320544007,10.1525180805119,-1.42037646288496));
#38774=CARTESIAN_POINT('Ctrl Pts',(5.96371874216079,10.1497574026567,-1.413253735847));
#38775=CARTESIAN_POINT('Ctrl Pts',(5.97059811441644,10.1423547681552,-1.39415446107384));
#38776=CARTESIAN_POINT('Ctrl Pts',(5.97633958133714,10.1356890572738,-1.37531958504562));
#38777=CARTESIAN_POINT('Ctrl Pts',(5.98107332754243,10.1297035854556,-1.35693324828585));
#38778=CARTESIAN_POINT('Ctrl Pts',(5.98611100708851,10.1233338124166,-1.33736640447865));
#38779=CARTESIAN_POINT('Ctrl Pts',(5.99000695673524,10.1177345595621,-1.3183072745247));
#38780=CARTESIAN_POINT('Ctrl Pts',(5.99291128797468,10.1128388295157,-1.2999196848561));
#38781=CARTESIAN_POINT('Ctrl Pts',(5.99361898113252,10.1116458958002,-1.29543921402657));
#38782=CARTESIAN_POINT('Ctrl Pts',(5.99426778584006,10.1104947342988,-1.29099837052087));
#38783=CARTESIAN_POINT('Ctrl Pts',(5.99485986277889,10.1093843755169,-1.28659907171658));
#38784=CARTESIAN_POINT('Ctrl Pts',(5.99739682029324,10.1046266609859,-1.26774876117852));
#38785=CARTESIAN_POINT('Ctrl Pts',(5.99889426417414,10.100617369373,-1.24966510146631));
#38786=CARTESIAN_POINT('Ctrl Pts',(5.99956526156832,10.0972659791722,-1.23247198354656));
#38787=CARTESIAN_POINT('Ctrl Pts',(5.99985052298196,10.0958412012004,-1.22516266585727));
#38788=CARTESIAN_POINT('Ctrl Pts',(5.9999861332354,10.0945354314074,-1.21801369646564));
#38789=CARTESIAN_POINT('Ctrl Pts',(5.99998739574847,10.093342129965,-1.21103206229897));
#38790=CARTESIAN_POINT('Ctrl Pts',(5.99970218885082,10.0072537640941,-1.15840945237376));
#38791=CARTESIAN_POINT('Ctrl Pts',(5.99970218885082,10.4047340562143,-1.32642148281801));
#38792=CARTESIAN_POINT('Ctrl Pts',(5.99970218885082,11.3017776556714,-1.63820419624065));
#38793=CARTESIAN_POINT('Ctrl Pts',(5.99970218885082,12.7412413732199,-1.91712741021756));
#38794=CARTESIAN_POINT('Ctrl Pts',(5.99970218885082,14.2901880401604,-1.97136832589254));
#38795=CARTESIAN_POINT('Ctrl Pts',(5.99970218885082,15.8279955162323,-1.78467115077639));
#38796=CARTESIAN_POINT('Ctrl Pts',(5.99970218885082,17.3193006181559,-1.36141279701238));
#38797=CARTESIAN_POINT('Ctrl Pts',(5.99970218885082,18.6019975902749,-0.768446409410351));
#38798=CARTESIAN_POINT('Ctrl Pts',(5.99970218885082,19.3573547509784,-0.286407566908898));
#38799=CARTESIAN_POINT('Ctrl Pts',(5.99970218885082,19.6640972928094,-0.0649546759702413));
#38800=CARTESIAN_POINT('Ctrl Pts',(6.00690077665715,9.93465823492307,-1.33014020345178));
#38801=CARTESIAN_POINT('Ctrl Pts',(6.00690077665715,10.339650355467,-1.50132938399891));
#38802=CARTESIAN_POINT('Ctrl Pts',(6.00690077665715,11.2534797462814,-1.81894736376076));
#38803=CARTESIAN_POINT('Ctrl Pts',(6.00690077665715,12.7201657060177,-2.10314012549508));
#38804=CARTESIAN_POINT('Ctrl Pts',(6.00690077665715,14.2981396447801,-2.15840027503973));
#38805=CARTESIAN_POINT('Ctrl Pts',(6.00690077665715,15.8650159409265,-1.96817595341715));
#38806=CARTESIAN_POINT('Ctrl Pts',(6.00690077665715,17.3842794608967,-1.53697638991161));
#38807=CARTESIAN_POINT('Ctrl Pts',(6.00690077665715,18.6912061461468,-0.932814930207615));
#38808=CARTESIAN_POINT('Ctrl Pts',(6.00690077665715,19.4607068236737,-0.441751837926806));
#38809=CARTESIAN_POINT('Ctrl Pts',(6.00690077665715,19.7732356586246,-0.216119001381029));
#38810=CARTESIAN_POINT('Ctrl Pts',(5.89988022250419,9.87508958651989,-1.47105478659189));
#38811=CARTESIAN_POINT('Ctrl Pts',(5.89988022250419,10.286245577916,-1.64485099459073));
#38812=CARTESIAN_POINT('Ctrl Pts',(5.89988022250419,11.2138486392983,-1.96725713324961));
#38813=CARTESIAN_POINT('Ctrl Pts',(5.89988022250419,12.7028719549598,-2.25577385048283));
#38814=CARTESIAN_POINT('Ctrl Pts',(5.89988022250419,14.3046643763385,-2.31187033780927));
#38815=CARTESIAN_POINT('Ctrl Pts',(5.89988022250419,15.8953932477307,-2.11875179732357));
#38816=CARTESIAN_POINT('Ctrl Pts',(5.89988022250419,17.4375981966469,-1.68103603184313));
#38817=CARTESIAN_POINT('Ctrl Pts',(5.89988022250419,18.7644067021557,-1.06768839604758));
#38818=CARTESIAN_POINT('Ctrl Pts',(5.89988022250419,19.5455129178013,-0.569220407507801));
#38819=CARTESIAN_POINT('Ctrl Pts',(5.89988022250419,19.862789726409,-0.340157694318395));
#38820=CARTESIAN_POINT('Ctrl Pts',(5.72194811176411,9.85291204087539,-1.52351761197645));
#38821=CARTESIAN_POINT('Ctrl Pts',(5.72194811176411,10.2663628556535,-1.6982844223277));
#38822=CARTESIAN_POINT('Ctrl Pts',(5.72194811176411,11.199093886461,-2.02247320362448));
#38823=CARTESIAN_POINT('Ctrl Pts',(5.72194811176411,12.6964334514226,-2.31259973949581));
#38824=CARTESIAN_POINT('Ctrl Pts',(5.72194811176411,14.3070935489958,-2.36900759731379));
#38825=CARTESIAN_POINT('Ctrl Pts',(5.72194811176411,15.9067027893476,-2.17481153244808));
#38826=CARTESIAN_POINT('Ctrl Pts',(5.72194811176411,17.457448885353,-1.73466976989276));
#38827=CARTESIAN_POINT('Ctrl Pts',(5.72194811176411,18.7916594385481,-1.11790209948377));
#38828=CARTESIAN_POINT('Ctrl Pts',(5.72194811176411,19.5770864228865,-0.616677250928825));
#38829=CARTESIAN_POINT('Ctrl Pts',(5.72194811176411,19.8961309130786,-0.386337586725996));
#38830=CARTESIAN_POINT('Ctrl Pts',(5.73278343895284,10.3449559317257,-1.71288935416517));
#38831=CARTESIAN_POINT('Ctrl Pts',(5.73338951138606,10.6015227812206,-1.80593972809553));
#38832=CARTESIAN_POINT('Ctrl Pts',(5.73395354664378,10.8620214983833,-1.8889039136407));
#38833=CARTESIAN_POINT('Ctrl Pts',(5.73447555380531,11.1255734077639,-1.96144088568236));
#38834=CARTESIAN_POINT('Ctrl Pts',(5.73532470571528,11.5542947428651,-2.0794371755631));
#38835=CARTESIAN_POINT('Ctrl Pts',(5.73606264400881,11.9910976959887,-2.16984187011366));
#38836=CARTESIAN_POINT('Ctrl Pts',(5.73668942675903,12.4324355283466,-2.23165186408241));
#38837=CARTESIAN_POINT('Ctrl Pts',(5.73681690515044,12.5221971513587,-2.24422310762926));
#38838=CARTESIAN_POINT('Ctrl Pts',(5.7369397855595,12.612146198574,-2.25561146181761));
#38839=CARTESIAN_POINT('Ctrl Pts',(5.73705806849707,12.7022525780884,-2.26580840528823));
#38840=CARTESIAN_POINT('Ctrl Pts',(5.73707478430295,12.7149864582159,-2.26724944261013));
#38841=CARTESIAN_POINT('Ctrl Pts',(5.73709140829046,12.7277234803624,-2.26866668563992));
#38842=CARTESIAN_POINT('Ctrl Pts',(5.73710794046104,12.7404635562604,-2.27006012790935));
#38843=CARTESIAN_POINT('Ctrl Pts',(5.73767502813854,13.1774745354613,-2.31785808260716));
#38844=CARTESIAN_POINT('Ctrl Pts',(5.73813408874745,13.6180830602428,-2.33765179056008));
#38845=CARTESIAN_POINT('Ctrl Pts',(5.73848518360082,14.0587002405137,-2.32917720787917));
#38846=CARTESIAN_POINT('Ctrl Pts',(5.73855071706245,14.1409434542674,-2.32759538822686));
#38847=CARTESIAN_POINT('Ctrl Pts',(5.73861248895409,14.2231868244508,-2.32502868692948));
#38848=CARTESIAN_POINT('Ctrl Pts',(5.73867049959467,14.3054068119284,-2.32147536423056));
#38849=CARTESIAN_POINT('Ctrl Pts',(5.73897977936498,14.7437570626134,-2.30253106682041));
#38850=CARTESIAN_POINT('Ctrl Pts',(5.73918215114308,15.1814468350129,-2.25554274024818));
#38851=CARTESIAN_POINT('Ctrl Pts',(5.73927764630324,15.6148687029248,-2.18075653749148));
#38852=CARTESIAN_POINT('Ctrl Pts',(5.73929840881837,15.7091030921352,-2.1644965546436));
#38853=CARTESIAN_POINT('Ctrl Pts',(5.73931411902304,15.8031355368143,-2.14692253669996));
#38854=CARTESIAN_POINT('Ctrl Pts',(5.73932477703665,15.8969286328972,-2.1280370230487));
#38855=CARTESIAN_POINT('Ctrl Pts',(5.73937358626944,16.3264616798984,-2.04154929035207));
#38856=CARTESIAN_POINT('Ctrl Pts',(5.73931644080057,16.7509790383427,-1.92755545699466));
#38857=CARTESIAN_POINT('Ctrl Pts',(5.73915333155579,17.1669747746921,-1.78675913166143));
#38858=CARTESIAN_POINT('Ctrl Pts',(5.73911747417873,17.2584258508751,-1.75580695030658));
#38859=CARTESIAN_POINT('Ctrl Pts',(5.73907649564396,17.349464895975,-1.72355948667232));
#38860=CARTESIAN_POINT('Ctrl Pts',(5.73903039564377,17.4400543274668,-1.69002427007247));
#38861=CARTESIAN_POINT('Ctrl Pts',(5.73900084443013,17.4981243411746,-1.66852738621326));
#38862=CARTESIAN_POINT('Ctrl Pts',(5.73896918874359,17.5560096006854,-1.64650134931223));
#38863=CARTESIAN_POINT('Ctrl Pts',(5.73893542848779,17.6137010993935,-1.62395008432201));
#38864=CARTESIAN_POINT('Ctrl Pts',(5.73869640195945,18.0221636043077,-1.46428451152245));
#38865=CARTESIAN_POINT('Ctrl Pts',(5.73835187092069,18.4209173985343,-1.27828864360647));
#38866=CARTESIAN_POINT('Ctrl Pts',(5.73790179987834,18.8067382170266,-1.06736636396035));
#38867=CARTESIAN_POINT('Ctrl Pts',(5.73786596848425,18.8374544740072,-1.05057426090624));
#38868=CARTESIAN_POINT('Ctrl Pts',(5.73782946814598,18.868088733853,-1.03362417965316));
#38869=CARTESIAN_POINT('Ctrl Pts',(5.73779229884009,18.8986393563168,-1.01651683389843));
#38870=CARTESIAN_POINT('Ctrl Pts',(5.73741169569616,19.2114690603014,-0.84134246831089));
#38871=CARTESIAN_POINT('Ctrl Pts',(5.73696095042693,19.5155310886977,-0.649677705755805));
#38872=CARTESIAN_POINT('Ctrl Pts',(5.73644003522154,19.8089444558277,-0.442538425497627));
#38873=CARTESIAN_POINT('Ctrl Pts',(5.99999999930604,10.093342130059,-1.2110320640041));
#38874=CARTESIAN_POINT('Ctrl Pts',(5.99999999931574,10.2345701328353,-1.2690562326139));
#38875=CARTESIAN_POINT('Ctrl Pts',(5.9999999983593,10.3766480618126,-1.32363361111499));
#38876=CARTESIAN_POINT('Ctrl Pts',(5.99999999609549,10.5196451747559,-1.37484620718349));
#38877=CARTESIAN_POINT('Ctrl Pts',(5.99999999382046,10.6633506397232,-1.42631249051412));
#38878=CARTESIAN_POINT('Ctrl Pts',(5.99999999024024,10.8079848606125,-1.47438070543796));
#38879=CARTESIAN_POINT('Ctrl Pts',(5.9999999903917,10.9536373602466,-1.51908518767612));
#38880=CARTESIAN_POINT('Ctrl Pts',(5.99999999048562,11.0439530244963,-1.54680537798127));
#38881=CARTESIAN_POINT('Ctrl Pts',(5.99999999231407,11.1346605645158,-1.57323126119436));
#38882=CARTESIAN_POINT('Ctrl Pts',(5.99999999505303,11.2257838770401,-1.59836128795789));
#38883=CARTESIAN_POINT('Ctrl Pts',(5.99999999721704,11.2977790699919,-1.61821615358561));
#38884=CARTESIAN_POINT('Ctrl Pts',(5.99999999999976,11.3700338430068,-1.63726195422479));
#38885=CARTESIAN_POINT('Ctrl Pts',(5.99999999999976,11.4425636725777,-1.65549750785664));
#38886=CARTESIAN_POINT('Ctrl Pts',(5.99999999999976,11.6207224355689,-1.70029043921647));
#38887=CARTESIAN_POINT('Ctrl Pts',(5.99999998462037,11.8005057414763,-1.7402636201257));
#38888=CARTESIAN_POINT('Ctrl Pts',(5.99999998025208,11.9814335037277,-1.77525495536016));
#38889=CARTESIAN_POINT('Ctrl Pts',(5.99999997588683,12.1622357141048,-1.81022200892735));
#38890=CARTESIAN_POINT('Ctrl Pts',(5.99999998175318,12.3441803503634,-1.84021401163938));
#38891=CARTESIAN_POINT('Ctrl Pts',(5.99999999007209,12.5267747451034,-1.86511936449999));
#38892=CARTESIAN_POINT('Ctrl Pts',(5.99999999337634,12.5993008924312,-1.87501172342695));
#38893=CARTESIAN_POINT('Ctrl Pts',(5.99999999675179,12.6719294358255,-1.88410214542636));
#38894=CARTESIAN_POINT('Ctrl Pts',(5.99999999861021,12.7446291471263,-1.89238589423402));
#38895=CARTESIAN_POINT('Ctrl Pts',(5.99999999947177,12.7783326929135,-1.89622623558109));
#38896=CARTESIAN_POINT('Ctrl Pts',(5.99999999999976,12.8120515323859,-1.89989322143732));
#38897=CARTESIAN_POINT('Ctrl Pts',(5.99999999999976,12.8457823808324,-1.90338681610497));
#38898=CARTESIAN_POINT('Ctrl Pts',(5.99999999999976,13.0574331213622,-1.92530805237903));
#38899=CARTESIAN_POINT('Ctrl Pts',(5.99999998564335,13.2695715411693,-1.94033615669064));
#38900=CARTESIAN_POINT('Ctrl Pts',(5.99999998504722,13.4819409326284,-1.94851509625262));
#38901=CARTESIAN_POINT('Ctrl Pts',(5.99999998445037,13.6945673780514,-1.9567039356821));
#38902=CARTESIAN_POINT('Ctrl Pts',(5.9999999941301,13.9074259309238,-1.9580270706869));
#38903=CARTESIAN_POINT('Ctrl Pts',(5.99999999838063,14.1202649109823,-1.95247694787897));
#38904=CARTESIAN_POINT('Ctrl Pts',(5.99999999937189,14.1699005355257,-1.95118261818528));
#38905=CARTESIAN_POINT('Ctrl Pts',(5.99999999999976,14.2195350999111,-1.94951425840285));
#38906=CARTESIAN_POINT('Ctrl Pts',(5.99999999999976,14.2691654064614,-1.9474713641832));
#38907=CARTESIAN_POINT('Ctrl Pts',(5.99999999999976,14.2759025341524,-1.94719404896648));
#38908=CARTESIAN_POINT('Ctrl Pts',(5.99999999998822,14.2826395839499,-1.94690987504035));
#38909=CARTESIAN_POINT('Ctrl Pts',(5.99999999996617,14.2893765357274,-1.94661884102389));
#38910=CARTESIAN_POINT('Ctrl Pts',(5.99999999925251,14.5074225361486,-1.93719932825757));
#38911=CARTESIAN_POINT('Ctrl Pts',(5.99999999047932,14.7253659037648,-1.92058926833469));
#38912=CARTESIAN_POINT('Ctrl Pts',(5.9999999900727,14.9425466810117,-1.896835398383));
#38913=CARTESIAN_POINT('Ctrl Pts',(5.99999998966584,15.1598616306626,-1.87306685349609));
#38914=CARTESIAN_POINT('Ctrl Pts',(5.9999999969317,15.3764124894709,-1.84214572408041));
#38915=CARTESIAN_POINT('Ctrl Pts',(5.9999999994141,15.5915425240749,-1.80417066887197));
#38916=CARTESIAN_POINT('Ctrl Pts',(5.99999999977852,15.6231239934002,-1.79859586364592));
#38917=CARTESIAN_POINT('Ctrl Pts',(5.99999999999976,15.654674859378,-1.79286913108824));
#38918=CARTESIAN_POINT('Ctrl Pts',(5.99999999999976,15.686193063671,-1.78699087606494));
#38919=CARTESIAN_POINT('Ctrl Pts',(5.99999999999976,15.7318227336747,-1.77848078347155));
#38920=CARTESIAN_POINT('Ctrl Pts',(5.9999999995305,15.7773834590749,-1.76965175942691));
#38921=CARTESIAN_POINT('Ctrl Pts',(5.99999999872742,15.822872815609,-1.76050414225716));
#38922=CARTESIAN_POINT('Ctrl Pts',(5.99999999501575,16.0331161038684,-1.71822556854151));
#38923=CARTESIAN_POINT('Ctrl Pts',(5.99999998445161,16.2418360185537,-1.66914547855914));
#38924=CARTESIAN_POINT('Ctrl Pts',(5.99999998419206,16.4487787393024,-1.61332739853338));
#38925=CARTESIAN_POINT('Ctrl Pts',(5.99999998393252,16.655721460051,-1.55750931850762));
#38926=CARTESIAN_POINT('Ctrl Pts',(5.99999999999976,16.8608875382432,-1.49495305224471));
#38927=CARTESIAN_POINT('Ctrl Pts',(5.99999999999976,17.0640039415638,-1.42567351722652));
#38928=CARTESIAN_POINT('Ctrl Pts',(5.99999999999976,17.1462851294145,-1.39760880978853));
#38929=CARTESIAN_POINT('Ctrl Pts',(5.99999999597141,17.2282363682393,-1.36845265307108));
#38930=CARTESIAN_POINT('Ctrl Pts',(5.99999999157428,17.3098034003992,-1.33821915827955));
#38931=CARTESIAN_POINT('Ctrl Pts',(5.99999998233619,17.481170486579,-1.27470053108098));
#38932=CARTESIAN_POINT('Ctrl Pts',(5.99999997355916,17.6508403557923,-1.20642352175421));
#38933=CARTESIAN_POINT('Ctrl Pts',(5.99999997660579,17.818361722563,-1.13360431169194));
#38934=CARTESIAN_POINT('Ctrl Pts',(5.99999997965623,17.9860922997894,-1.06069416075198));
#38935=CARTESIAN_POINT('Ctrl Pts',(5.99999999487385,18.1516686004727,-0.983230670361461));
#38936=CARTESIAN_POINT('Ctrl Pts',(5.99999999914244,18.3146612115832,-0.901477355893947));
#38937=CARTESIAN_POINT('Ctrl Pts',(5.99999999968372,18.3353297517971,-0.891110495358455));
#38938=CARTESIAN_POINT('Ctrl Pts',(5.99999999999976,18.3559567822399,-0.880674713526301));
#38939=CARTESIAN_POINT('Ctrl Pts',(5.99999999999976,18.3765414594372,-0.870170598285201));
#38940=CARTESIAN_POINT('Ctrl Pts',(5.99999999999976,18.4906904314639,-0.811921739421176));
#38941=CARTESIAN_POINT('Ctrl Pts',(5.99999999306106,18.6035097023901,-0.751541582593229));
#38942=CARTESIAN_POINT('Ctrl Pts',(5.9999999914505,18.7150751423809,-0.689018196545716));
#38943=CARTESIAN_POINT('Ctrl Pts',(5.99999998952822,18.8482343794444,-0.614393237549431));
#38944=CARTESIAN_POINT('Ctrl Pts',(5.99999999274902,18.9796082754029,-0.536716140205771));
#38945=CARTESIAN_POINT('Ctrl Pts',(5.99999999547953,19.1092846788039,-0.45595063844579));
#38946=CARTESIAN_POINT('Ctrl Pts',(5.99999999819778,19.2383791002591,-0.375547608674738));
#38947=CARTESIAN_POINT('Ctrl Pts',(5.99999999961521,19.3657916282087,-0.2920836018942));
#38948=CARTESIAN_POINT('Ctrl Pts',(5.99999999985088,19.4915819744366,-0.205478937436434));
#38949=CARTESIAN_POINT('Ctrl Pts',(5.99999999991376,19.5251468526991,-0.182370049460026));
#38950=CARTESIAN_POINT('Ctrl Pts',(5.99999999993331,19.5585960651627,-0.15903731653548));
#38951=CARTESIAN_POINT('Ctrl Pts',(5.999999999933,19.5919303631537,-0.135478724431627));
#38952=CARTESIAN_POINT('Ctrl Pts',(-5.84353034391,10.0864246237472,-1.57297147931968));
#38953=CARTESIAN_POINT('Ctrl Pts',(-3.89568689594,10.6220908322031,-2.52887944306001));
#38954=CARTESIAN_POINT('Ctrl Pts',(0.0001666015265935,11.1575591931004,
-3.48561750059097));
#38955=CARTESIAN_POINT('Ctrl Pts',(3.896020098993,10.6220450329135,-2.52879761203758));
#38956=CARTESIAN_POINT('Ctrl Pts',(5.84403014849,10.0862871692312,-1.57272618876811));
#38957=CARTESIAN_POINT('Ctrl Pts',(-5.84353034391,10.8186450746373,-1.86224902860984));
#38958=CARTESIAN_POINT('Ctrl Pts',(-3.89568689594,11.3231575651093,-2.74792601689234));
#38959=CARTESIAN_POINT('Ctrl Pts',(0.0001666015265935,11.8270673123619,
-3.63586001146492));
#38960=CARTESIAN_POINT('Ctrl Pts',(3.896020098993,11.3231144650679,-2.74785007076882));
#38961=CARTESIAN_POINT('Ctrl Pts',(5.84403014849,10.8185156143099,-1.86202175967931));
#38962=CARTESIAN_POINT('Ctrl Pts',(-5.84353034391,12.4568729540691,-2.30089098012815));
#38963=CARTESIAN_POINT('Ctrl Pts',(-3.89568689594,12.8710971370357,-3.0672794361297));
#38964=CARTESIAN_POINT('Ctrl Pts',(0.0001666015265935,13.2856323394137,
-3.8324424808477));
#38965=CARTESIAN_POINT('Ctrl Pts',(3.896020098993,12.8710616813125,-3.06721399076156));
#38966=CARTESIAN_POINT('Ctrl Pts',(5.84403014849,12.4567666621639,-2.30069432116796));
#38967=CARTESIAN_POINT('Ctrl Pts',(-5.84353034391,15.0614254536629,-2.34071384846406));
#38968=CARTESIAN_POINT('Ctrl Pts',(-3.89568689594,15.2991206270769,-3.03320173188209));
#38969=CARTESIAN_POINT('Ctrl Pts',(0.0001666015265936,15.5368879417598,
-3.72636712888337));
#38970=CARTESIAN_POINT('Ctrl Pts',(3.896020098993,15.2991002905397,-3.0331424445665));
#38971=CARTESIAN_POINT('Ctrl Pts',(5.84403014849,15.0613644599445,-2.34053615276473));
#38972=CARTESIAN_POINT('Ctrl Pts',(-5.84353034391,17.6858135162578,-1.67939836042705));
#38973=CARTESIAN_POINT('Ctrl Pts',(-3.89568689594,17.7477953412524,-2.42360807923413));
#38974=CARTESIAN_POINT('Ctrl Pts',(0.0001666015265931,17.8092309023956,
-3.16660406681614));
#38975=CARTESIAN_POINT('Ctrl Pts',(3.896020098993,17.7477900865853,-2.42354452984376));
#38976=CARTESIAN_POINT('Ctrl Pts',(5.84403014849,17.6857976114169,-1.6792073926346));
#38977=CARTESIAN_POINT('Ctrl Pts',(-5.84353034391,19.2592933957493,-0.803936074634235));
#38978=CARTESIAN_POINT('Ctrl Pts',(-3.89568689594,19.2409363984223,-1.65690459370082));
#38979=CARTESIAN_POINT('Ctrl Pts',(0.0001666015265944,19.2238042951407,
-2.51236029214794));
#38980=CARTESIAN_POINT('Ctrl Pts',(3.896020098993,19.2409378637509,-1.65683142548429));
#38981=CARTESIAN_POINT('Ctrl Pts',(5.84403014849,19.2592981062585,-0.803717198855546));
#38982=CARTESIAN_POINT('Ctrl Pts',(-5.84353034391,19.9729831098892,-0.275591925382267));
#38983=CARTESIAN_POINT('Ctrl Pts',(-3.89568689594,19.9313477984332,-1.1982202827636));
#38984=CARTESIAN_POINT('Ctrl Pts',(0.0001666015265944,19.8897492520045,
-2.12096519186025));
#38985=CARTESIAN_POINT('Ctrl Pts',(3.896020098993,19.9313513564076,-1.19814135921599));
#38986=CARTESIAN_POINT('Ctrl Pts',(5.84403014849,19.9729937937055,-0.275355174534935));
#38987=CARTESIAN_POINT('Ctrl Pts',(-5.73278975502083,10.3449510841595,-1.7128961697678));
#38988=CARTESIAN_POINT('Ctrl Pts',(-5.37901580620726,10.4448361796299,-1.88167915312222));
#38989=CARTESIAN_POINT('Ctrl Pts',(-5.01621987753293,10.5336323549078,-2.03731789625457));
#38990=CARTESIAN_POINT('Ctrl Pts',(-4.64601513709761,10.6117448313211,-2.17806966584278));
#38991=CARTESIAN_POINT('Ctrl Pts',(-4.37166252199081,10.6696326966986,-2.28237847621087));
#38992=CARTESIAN_POINT('Ctrl Pts',(-4.09324095252986,10.7216528047211,-2.37850735433697));
#38993=CARTESIAN_POINT('Ctrl Pts',(-3.81140699867882,10.7679937575164,-2.46576099137469));
#38994=CARTESIAN_POINT('Ctrl Pts',(-3.57236698582203,10.8072982550783,-2.5397659515092));
#38995=CARTESIAN_POINT('Ctrl Pts',(-3.33087219324492,10.8425171603883,-2.60738551856862));
#38996=CARTESIAN_POINT('Ctrl Pts',(-3.08732322273381,10.8737878367289,-2.66822937065829));
#38997=CARTESIAN_POINT('Ctrl Pts',(-3.04372206931726,10.8793860437495,-2.67912189105715));
#38998=CARTESIAN_POINT('Ctrl Pts',(-3.00005508020644,10.8848577806713,-2.68979736726869));
#38999=CARTESIAN_POINT('Ctrl Pts',(-2.95632455391942,10.8902039324604,-2.70025372277678));
#39000=CARTESIAN_POINT('Ctrl Pts',(-2.75788264616247,10.9144638865531,-2.74770293757909));
#39001=CARTESIAN_POINT('Ctrl Pts',(-2.55812786428845,10.9361985805701,-2.79065506823792));
#39002=CARTESIAN_POINT('Ctrl Pts',(-2.35732700629461,10.9553876930419,-2.82889428277911));
#39003=CARTESIAN_POINT('Ctrl Pts',(-2.16336841517962,10.9739229386428,-2.86583050034239));
#39004=CARTESIAN_POINT('Ctrl Pts',(-1.96843382320251,10.9900831075099,-2.89836945730171));
#39005=CARTESIAN_POINT('Ctrl Pts',(-1.77276367380457,11.0038735436133,-2.92635857466279));
#39006=CARTESIAN_POINT('Ctrl Pts',(-1.58018406103536,11.0174461649503,-2.95390561441175));
#39007=CARTESIAN_POINT('Ctrl Pts',(-1.3868919430529,11.0287232475636,-2.97704526002274));
#39008=CARTESIAN_POINT('Ctrl Pts',(-1.19311654915955,11.0377339936928,-2.99567504720032));
#39009=CARTESIAN_POINT('Ctrl Pts',(-0.994951121524408,11.0469488807025,
-3.01472689722432));
#39010=CARTESIAN_POINT('Ctrl Pts',(-0.796280272439716,11.0537933397654,
-3.0290617895358));
#39011=CARTESIAN_POINT('Ctrl Pts',(-0.597349166591621,11.0583266053215,
-3.03862030630298));
#39012=CARTESIAN_POINT('Ctrl Pts',(-0.408571857533149,11.0626284849561,
-3.04769093940587));
#39013=CARTESIAN_POINT('Ctrl Pts',(-0.219560181608441,11.0648492036146,
-3.05246055293869));
#39014=CARTESIAN_POINT('Ctrl Pts',(-0.0305236461352285,11.0650646066962,
-3.05292367184669));
#39015=CARTESIAN_POINT('Ctrl Pts',(-0.0203559062909503,11.0650761926178,
-3.05294858170108));
#39016=CARTESIAN_POINT('Ctrl Pts',(-0.0101880945265215,11.0650819831622,
-3.05296104360322));
#39017=CARTESIAN_POINT('Ctrl Pts',(-2.02434432647914E-5,11.0650819922319,
-3.05296106047373));
#39018=CARTESIAN_POINT('Ctrl Pts',(-1.34956290334826E-5,11.0650819922379,
-3.05296106048493));
#39019=CARTESIAN_POINT('Ctrl Pts',(-6.74781482048857E-6,11.0650819922414,
-3.05296106049064));
#39020=CARTESIAN_POINT('Ctrl Pts',(-6.24391702939142E-13,11.0650819922423,
-3.05296106049087));
#39021=CARTESIAN_POINT('Ctrl Pts',(0.189391034103492,11.0650820182466,-3.0529610670559));
#39022=CARTESIAN_POINT('Ctrl Pts',(0.378768545059335,11.0630740529817,-3.04863949431656));
#39023=CARTESIAN_POINT('Ctrl Pts',(0.567921848613415,11.0589804704103,-3.03999941059282));
#39024=CARTESIAN_POINT('Ctrl Pts',(0.769326050312761,11.0546217586437,-3.03079973428636));
#39025=CARTESIAN_POINT('Ctrl Pts',(0.970476061616078,11.0478983328162,-3.01670370047049));
#39026=CARTESIAN_POINT('Ctrl Pts',(1.17111755353397,11.038747420467,-2.99777056713526));
#39027=CARTESIAN_POINT('Ctrl Pts',(1.36691637355855,11.0298173740295,-2.97929440285354));
#39028=CARTESIAN_POINT('Ctrl Pts',(1.56223092515411,11.018575855937,-2.95621227598697));
#39029=CARTESIAN_POINT('Ctrl Pts',(1.75682485384488,11.0049919071274,-2.92862831235811));
#39030=CARTESIAN_POINT('Ctrl Pts',(1.95863808969716,10.9909040027237,-2.90002100176509));
#39031=CARTESIAN_POINT('Ctrl Pts',(2.15967624153261,10.9742966294215,-2.86657163013415));
#39032=CARTESIAN_POINT('Ctrl Pts',(2.35967566109098,10.9551636073509,-2.8284469262728));
#39033=CARTESIAN_POINT('Ctrl Pts',(2.55967508064935,10.9360305852803,-2.79032222241145));
#39034=CARTESIAN_POINT('Ctrl Pts',(2.75863576793065,10.9143720907802,-2.74752252151317));
#39035=CARTESIAN_POINT('Ctrl Pts',(2.95629407467463,10.8902082476216,-2.70026117661292));
#39036=CARTESIAN_POINT('Ctrl Pts',(3.19879463434546,10.8605624129168,-2.64227776686961));
#39037=CARTESIAN_POINT('Ctrl Pts',(3.43934160302183,10.8270524690154,-2.5775523679393));
#39038=CARTESIAN_POINT('Ctrl Pts',(3.67754301047263,10.7895391923811,-2.50645885904836));
#39039=CARTESIAN_POINT('Ctrl Pts',(3.96237540988465,10.7446822089236,-2.42144788057962));
#39040=CARTESIAN_POINT('Ctrl Pts',(4.24385401127729,10.694101158698,-2.32733227970892));
#39041=CARTESIAN_POINT('Ctrl Pts',(4.52130863956216,10.6375985200971,-2.22481497999281));
#39042=CARTESIAN_POINT('Ctrl Pts',(4.88831882413484,10.5628582140876,-2.08920760763328));
#39043=CARTESIAN_POINT('Ctrl Pts',(5.24828812203085,10.477757187457,-1.93890576546615));
#39044=CARTESIAN_POINT('Ctrl Pts',(5.5996654085723,10.381900692554,-1.77558867682684));
#39045=CARTESIAN_POINT('Ctrl Pts',(5.64417809415769,10.3697575342386,-1.7548995700013));
#39046=CARTESIAN_POINT('Ctrl Pts',(5.68855289536406,10.3574418257978,-1.73400154805331));
#39047=CARTESIAN_POINT('Ctrl Pts',(5.73278665880606,10.3449528049738,-1.7128979547254));
#39048=CARTESIAN_POINT('Ctrl Pts',(-5.84422935313255,10.3326179436783,-1.66677955401275));
#39049=CARTESIAN_POINT('Ctrl Pts',(-5.39723073539493,10.4682500954886,-1.88672368606665));
#39050=CARTESIAN_POINT('Ctrl Pts',(-4.37278936862451,10.7273674796295,-2.32714772276908));
#39051=CARTESIAN_POINT('Ctrl Pts',(-2.71089230894894,10.9902717063683,-2.8158221119383));
#39052=CARTESIAN_POINT('Ctrl Pts',(-0.904516202368409,11.1231766923864,
-3.08010999588275));
#39053=CARTESIAN_POINT('Ctrl Pts',(0.905422156638638,11.1231437154035,-3.08004278635486));
#39054=CARTESIAN_POINT('Ctrl Pts',(2.71180944555921,10.9901684408322,-2.81562160453371));
#39055=CARTESIAN_POINT('Ctrl Pts',(4.37341442202404,10.7272312569814,-2.32690647824196));
#39056=CARTESIAN_POINT('Ctrl Pts',(5.39759958770343,10.4681419380673,-1.886546911375));
#39057=CARTESIAN_POINT('Ctrl Pts',(5.84433805276918,10.3325849446319,-1.66672608703151));
#39058=CARTESIAN_POINT('Ctrl Pts',(-5.72537553697924,10.0515132270061,-1.59486222014698));
#39059=CARTESIAN_POINT('Ctrl Pts',(-5.28737692922011,10.1848998766557,-1.80870858998522));
#39060=CARTESIAN_POINT('Ctrl Pts',(-4.28358980961365,10.4398181577976,-2.23709191171346));
#39061=CARTESIAN_POINT('Ctrl Pts',(-2.65541314896773,10.6985985951467,-2.71261121371761));
#39062=CARTESIAN_POINT('Ctrl Pts',(-0.88596500427895,10.829464766054,-2.96982219801529));
#39063=CARTESIAN_POINT('Ctrl Pts',(0.886852389154446,10.8294322908905,-2.96975678663163));
#39064=CARTESIAN_POINT('Ctrl Pts',(2.65631159921206,10.6984969260531,-2.71241608186123));
#39065=CARTESIAN_POINT('Ctrl Pts',(4.28420224316951,10.4396841067023,-2.23685720221533));
#39066=CARTESIAN_POINT('Ctrl Pts',(5.28773835329507,10.1847935018816,-1.80853670049365));
#39067=CARTESIAN_POINT('Ctrl Pts',(5.72548204834205,10.0514807738283,-1.59481023378505));
#39068=CARTESIAN_POINT('Ctrl Pts',(-5.71942831533579,9.77836172016708,-1.74871820725318));
#39069=CARTESIAN_POINT('Ctrl Pts',(-5.28270068923074,9.91044415240004,-1.96030029454256));
#39070=CARTESIAN_POINT('Ctrl Pts',(-4.28157574258823,10.1630390832986,-2.38447623743461));
#39071=CARTESIAN_POINT('Ctrl Pts',(-2.6557887324519,10.4198723259329,-2.8562525631157));
#39072=CARTESIAN_POINT('Ctrl Pts',(-0.88645093086578,10.5499497734634,-3.11191327809778));
#39073=CARTESIAN_POINT('Ctrl Pts',(0.887338700652733,10.5499174748729,-3.11184821214888));
#39074=CARTESIAN_POINT('Ctrl Pts',(2.65668656115258,10.4197713255722,-2.85605874443294));
#39075=CARTESIAN_POINT('Ctrl Pts',(4.28218671263831,10.1629061704207,-2.38424365348559));
#39076=CARTESIAN_POINT('Ctrl Pts',(5.28306107935149,9.91033880165622,-1.9601302077373));
#39077=CARTESIAN_POINT('Ctrl Pts',(5.7195345147545,9.77832958295092,-1.74866677484432));
#39078=CARTESIAN_POINT('Ctrl Pts',(-5.83024722549531,9.69037424501856,-2.02853375411005));
#39079=CARTESIAN_POINT('Ctrl Pts',(-5.38623690424319,9.82293988326085,-2.24315406310329));
#39080=CARTESIAN_POINT('Ctrl Pts',(-4.36805474491177,10.0765945414732,-2.67368564029794));
#39081=CARTESIAN_POINT('Ctrl Pts',(-2.71177598656107,10.3349204760671,-3.15355950681661));
#39082=CARTESIAN_POINT('Ctrl Pts',(-0.905658932461119,10.4659710001726,
-3.41420239959998));
#39083=CARTESIAN_POINT('Ctrl Pts',(0.90656579194999,10.4659384383509,-3.41413600225329));
#39084=CARTESIAN_POINT('Ctrl Pts',(2.71269166196735,10.3348187828708,-3.15336208695204));
#39085=CARTESIAN_POINT('Ctrl Pts',(4.36867635738294,10.0764609950322,-2.6734493933936));
#39086=CARTESIAN_POINT('Ctrl Pts',(5.38660332554845,9.82283413356729,-2.24298152691996));
#39087=CARTESIAN_POINT('Ctrl Pts',(5.83035519169749,9.69034198886957,-2.0284815895926));
#39088=CARTESIAN_POINT('Ctrl Pts',(-5.72001750558411,9.72697457205148,-2.05943207691667));
#39089=CARTESIAN_POINT('Ctrl Pts',(-5.49206568348151,9.79330018878959,-2.16743192710529));
#39090=CARTESIAN_POINT('Ctrl Pts',(-5.25921576351921,9.85517369883701,-2.27049947746689));
#39091=CARTESIAN_POINT('Ctrl Pts',(-5.0216601982015,9.91261925507755,-2.36800096228074));
#39092=CARTESIAN_POINT('Ctrl Pts',(-4.83340321471274,9.95814345535555,-2.44526850763242));
#39093=CARTESIAN_POINT('Ctrl Pts',(-4.64219111721331,10.0008865508324,-2.51903966348394));
#39094=CARTESIAN_POINT('Ctrl Pts',(-4.4481258687923,10.0408548470982,-2.58897722641875));
#39095=CARTESIAN_POINT('Ctrl Pts',(-4.42435514837881,10.0457504953591,-2.59754375890435));
#39096=CARTESIAN_POINT('Ctrl Pts',(-4.40054162912284,10.0506045062339,-2.60605274953309));
#39097=CARTESIAN_POINT('Ctrl Pts',(-4.37668559068971,10.0554168977595,-2.61450355613505));
#39098=CARTESIAN_POINT('Ctrl Pts',(-4.14449479000357,10.1022559001649,-2.69675524921698));
#39099=CARTESIAN_POINT('Ctrl Pts',(-3.90827758451816,10.1451475506915,-2.77352066955216));
#39100=CARTESIAN_POINT('Ctrl Pts',(-3.66827959909047,10.1840646157826,-2.84432679982134));
#39101=CARTESIAN_POINT('Ctrl Pts',(-3.54828060637662,10.2035231483282,-2.87972986495593));
#39102=CARTESIAN_POINT('Ctrl Pts',(-3.42733711572398,10.2219871680773,-2.91364387703704));
#39103=CARTESIAN_POINT('Ctrl Pts',(-3.30548427923154,10.2394481351887,-2.94601451933545));
#39104=CARTESIAN_POINT('Ctrl Pts',(-3.24455786098532,10.2481786187444,-2.96219984048465));
#39105=CARTESIAN_POINT('Ctrl Pts',(-3.18340410134152,10.2566583148036,-2.97799931187828));
#39106=CARTESIAN_POINT('Ctrl Pts',(-3.12202776956448,10.264885806214,-2.99340654821786));
#39107=CARTESIAN_POINT('Ctrl Pts',(-3.08480107734262,10.2698760407495,-3.00275152581095));
#39108=CARTESIAN_POINT('Ctrl Pts',(-3.04679094731952,10.2748650953664,-3.01212474426539));
#39109=CARTESIAN_POINT('Ctrl Pts',(-3.00927407317018,10.2796842949948,-3.02120807144621));
#39110=CARTESIAN_POINT('Ctrl Pts',(-2.98493618726443,10.2828105983815,-3.02710059276053));
#39111=CARTESIAN_POINT('Ctrl Pts',(-2.96080619766097,10.2858659691822,-3.03287201197784));
#39112=CARTESIAN_POINT('Ctrl Pts',(-2.93723584159235,10.288810155411,-3.0384451782907));
#39113=CARTESIAN_POINT('Ctrl Pts',(-2.85104375385783,10.2995764568195,-3.05882513514834));
#39114=CARTESIAN_POINT('Ctrl Pts',(-2.76462199302743,10.3098384886512,-3.07833996422562));
#39115=CARTESIAN_POINT('Ctrl Pts',(-2.67798441088526,10.3196021825765,-3.09697541649601));
#39116=CARTESIAN_POINT('Ctrl Pts',(-2.41894336054858,10.3487950278409,-3.15269427441265));
#39117=CARTESIAN_POINT('Ctrl Pts',(-2.15797485850097,10.3735347225913,-3.20055455830548));
#39118=CARTESIAN_POINT('Ctrl Pts',(-1.89556992266632,10.3939293425982,-3.24032729421704));
#39119=CARTESIAN_POINT('Ctrl Pts',(-1.63420115925437,10.4142434292769,-3.27994297739637));
#39120=CARTESIAN_POINT('Ctrl Pts',(-1.37140674786025,10.4302466213787,-3.31153518973123));
#39121=CARTESIAN_POINT('Ctrl Pts',(-1.10765056326125,10.4420212989983,-3.33483767822194));
#39122=CARTESIAN_POINT('Ctrl Pts',(-1.03553024031539,10.4452409146968,-3.34120940746858));
#39123=CARTESIAN_POINT('Ctrl Pts',(-0.963337911030768,10.4481442389793,
-3.34696109130944));
#39124=CARTESIAN_POINT('Ctrl Pts',(-0.891082862512929,10.4507326466169,
-3.35208671100954));
#39125=CARTESIAN_POINT('Ctrl Pts',(-0.627875898516178,10.4601615644549,
-3.37075805408579));
#39126=CARTESIAN_POINT('Ctrl Pts',(-0.363837180964085,10.4654134527972,
-3.3811253229753));
#39127=CARTESIAN_POINT('Ctrl Pts',(-0.0994820302231884,10.4664670531146,
-3.38320655683317));
#39128=CARTESIAN_POINT('Ctrl Pts',(-0.0663911103587122,10.466598938586,
-3.38346707735874));
#39129=CARTESIAN_POINT('Ctrl Pts',(-0.0332952257283999,10.4666650110093,
-3.38359770416469));
#39130=CARTESIAN_POINT('Ctrl Pts',(-0.000195383006570636,10.4666652029542,
-3.38359842127642));
#39131=CARTESIAN_POINT('Ctrl Pts',(0.260328417753622,10.4666667137238,-3.38360406555319));
#39132=CARTESIAN_POINT('Ctrl Pts',(0.520593752654219,10.4625913206532,-3.3755578983993));
#39133=CARTESIAN_POINT('Ctrl Pts',(0.780120363257257,10.4544573923531,-3.35946676550572));
#39134=CARTESIAN_POINT('Ctrl Pts',(0.817425956250517,10.4532881826991,-3.35715374930621));
#39135=CARTESIAN_POINT('Ctrl Pts',(0.854716282561188,10.4520350739337,-3.35467442500711));
#39136=CARTESIAN_POINT('Ctrl Pts',(0.89198991048456,10.4506980809692,-3.35202873401766));
#39137=CARTESIAN_POINT('Ctrl Pts',(1.08871979571785,10.4436414436864,-3.33806479989815));
#39138=CARTESIAN_POINT('Ctrl Pts',(1.28498476952638,10.4342486516205,-3.3194675611386));
#39139=CARTESIAN_POINT('Ctrl Pts',(1.4806027073567,10.4224868529531,-3.29636060766967));
#39140=CARTESIAN_POINT('Ctrl Pts',(1.72586245691025,10.4077402717986,-3.26738982061612));
#39141=CARTESIAN_POINT('Ctrl Pts',(1.97009186766474,10.3892874677145,-3.23128119591996));
#39142=CARTESIAN_POINT('Ctrl Pts',(2.21291486465638,10.3670517966272,-3.18823396193957));
#39143=CARTESIAN_POINT('Ctrl Pts',(2.33432636315221,10.3559339610836,-3.16671034494937));
#39144=CARTESIAN_POINT('Ctrl Pts',(2.455386465299,10.3438695379754,-3.14345318748102));
#39145=CARTESIAN_POINT('Ctrl Pts',(2.57604938841735,10.3308436213554,-3.11849411619528));
#39146=CARTESIAN_POINT('Ctrl Pts',(2.61034999432425,10.3271407702972,-3.11139905131662));
#39147=CARTESIAN_POINT('Ctrl Pts',(2.64461855856262,10.3233601803353,-3.10416652345661));
#39148=CARTESIAN_POINT('Ctrl Pts',(2.67885392870299,10.3195015097565,-3.09679721177542));
#39149=CARTESIAN_POINT('Ctrl Pts',(2.70483527669272,10.316573150499,-3.09120461410673));
#39150=CARTESIAN_POINT('Ctrl Pts',(2.73079750695558,10.3135998217514,-3.08553323762981));
#39151=CARTESIAN_POINT('Ctrl Pts',(2.75674025459381,10.3105813374921,-3.0797835523159));
#39152=CARTESIAN_POINT('Ctrl Pts',(2.79332433319526,10.3063247156824,-3.0716754312182));
#39153=CARTESIAN_POINT('Ctrl Pts',(2.82916047457324,10.3020630585324,-3.0635725282504));
#39154=CARTESIAN_POINT('Ctrl Pts',(2.86554265400224,10.297642918513,-3.05518462723504));
#39155=CARTESIAN_POINT('Ctrl Pts',(2.88895590046142,10.2947983987706,-3.04978670999011));
#39156=CARTESIAN_POINT('Ctrl Pts',(2.91259502854718,10.2918877539081,-3.04426991457996));
#39157=CARTESIAN_POINT('Ctrl Pts',(2.93680184037229,10.2888644771338,-3.0385474416855));
#39158=CARTESIAN_POINT('Ctrl Pts',(3.1828164679285,10.2581388154889,-2.98038976078138));
#39159=CARTESIAN_POINT('Ctrl Pts',(3.4253594210897,10.2234388449908,-2.9157914273284));
#39160=CARTESIAN_POINT('Ctrl Pts',(3.66417651007782,10.1847920895663,-2.84531381876157));
#39161=CARTESIAN_POINT('Ctrl Pts',(3.91060789592046,10.1449131448143,-2.77258914556676));
#39162=CARTESIAN_POINT('Ctrl Pts',(4.1530722143786,10.1008318659714,-2.69360413379684));
#39163=CARTESIAN_POINT('Ctrl Pts',(4.39129440848135,10.0525670600447,-2.60892207677239));
#39164=CARTESIAN_POINT('Ctrl Pts',(4.4105414251735,10.0486675345248,-2.60208024168975));
#39165=CARTESIAN_POINT('Ctrl Pts',(4.42976075177401,10.0447406934149,-2.59520119067901));
#39166=CARTESIAN_POINT('Ctrl Pts',(4.44895224382876,10.0407865430965,-2.58828520675295));
#39167=CARTESIAN_POINT('Ctrl Pts',(4.69665557783849,9.9897505832941,-2.49902105409841));
#39168=CARTESIAN_POINT('Ctrl Pts',(4.93972238691474,9.93416654528795,-2.40360864190788));
#39169=CARTESIAN_POINT('Ctrl Pts',(5.17793597175251,9.87405249029242,-2.30262611824544));
#39170=CARTESIAN_POINT('Ctrl Pts',(5.36154614781137,9.8277178019124,-2.22479084717491));
#39171=CARTESIAN_POINT('Ctrl Pts',(5.54227296781462,9.77869150699081,-2.14364519080835));
#39172=CARTESIAN_POINT('Ctrl Pts',(5.7200146623697,9.72697523687866,-2.05943412015819));
#39173=CARTESIAN_POINT('Ctrl Pts',(6.05077471961553,6.21842583509821,-8.31822495858353));
#39174=CARTESIAN_POINT('Ctrl Pts',(6.05142593340447,6.23969193373903,-8.30198934364668));
#39175=CARTESIAN_POINT('Ctrl Pts',(6.04716899616723,6.29515597960163,-8.26241512108273));
#39176=CARTESIAN_POINT('Ctrl Pts',(6.01567297877913,6.39159059660638,-8.20453501924637));
#39177=CARTESIAN_POINT('Ctrl Pts',(5.94753066244136,6.50078121143289,-8.15338924888124));
#39178=CARTESIAN_POINT('Ctrl Pts',(5.84910732584619,6.60164332898259,-8.12175932743906));
#39179=CARTESIAN_POINT('Ctrl Pts',(5.76414023552456,6.65913247159952,-8.11648748828758));
#39180=CARTESIAN_POINT('Ctrl Pts',(5.71687096680919,6.68389896885781,-8.11896177582376));
#39181=CARTESIAN_POINT('Ctrl Pts',(5.71191285258273,6.6864219935317,-8.11927735102364));
#39182=CARTESIAN_POINT('Ctrl Pts',(5.9119429072752,6.04924592523811,-8.09057562670355));
#39183=CARTESIAN_POINT('Ctrl Pts',(5.91254068779913,6.06837636901304,-8.07595986584746));
#39184=CARTESIAN_POINT('Ctrl Pts',(5.90863665457664,6.11851658263178,-8.04024430370093));
#39185=CARTESIAN_POINT('Ctrl Pts',(5.87944445404612,6.20656764599406,-7.9878084478441));
#39186=CARTESIAN_POINT('Ctrl Pts',(5.81592145568837,6.30701177251466,-7.94151268428573));
#39187=CARTESIAN_POINT('Ctrl Pts',(5.72394918073557,6.40018754436466,-7.91317658918676));
#39188=CARTESIAN_POINT('Ctrl Pts',(5.64455513570018,6.45339418295547,-7.9088733448521));
#39189=CARTESIAN_POINT('Ctrl Pts',(5.60044619117731,6.47632149431093,-7.91141082748276));
#39190=CARTESIAN_POINT('Ctrl Pts',(5.59582027554415,6.47865725297412,-7.91172803484192));
#39191=CARTESIAN_POINT('Ctrl Pts',(6.02852050621993,5.86900777502338,-7.85896159208741));
#39192=CARTESIAN_POINT('Ctrl Pts',(6.02945804993531,5.89850257739766,-7.83645112392778));
#39193=CARTESIAN_POINT('Ctrl Pts',(6.02330228130752,5.97418179417425,-7.78245669334098));
#39194=CARTESIAN_POINT('Ctrl Pts',(5.98006183254276,6.10142380740703,-7.70591992048359));
#39195=CARTESIAN_POINT('Ctrl Pts',(5.88924834938387,6.24220627570421,-7.63973400270886));
#39196=CARTESIAN_POINT('Ctrl Pts',(5.75973686058714,6.37117340314249,-7.59922294714483));
#39197=CARTESIAN_POINT('Ctrl Pts',(5.64790222410802,6.4451134530259,-7.59259942739894));
#39198=CARTESIAN_POINT('Ctrl Pts',(5.58523655084478,6.47730266427808,-7.59598554867957));
#39199=CARTESIAN_POINT('Ctrl Pts',(5.57865817275388,6.48058621946311,-7.59641446277799));
#39200=CARTESIAN_POINT('Ctrl Pts',(6.32408553231757,5.79586551090958,-7.7752161516984));
#39201=CARTESIAN_POINT('Ctrl Pts',(6.32553330551962,5.84143037849579,-7.74047175332521));
#39202=CARTESIAN_POINT('Ctrl Pts',(6.31599727660815,5.95676945960246,-7.6580435523049));
#39203=CARTESIAN_POINT('Ctrl Pts',(6.25156577757377,6.14508548193301,-7.54365994334047));
#39204=CARTESIAN_POINT('Ctrl Pts',(6.11944215589101,6.34884751030328,-7.44588260852661));
#39205=CARTESIAN_POINT('Ctrl Pts',(5.93300983305097,6.53362083847875,-7.38570904471001));
#39206=CARTESIAN_POINT('Ctrl Pts',(5.77198724572357,6.63971852407646,-7.37499742538782));
#39207=CARTESIAN_POINT('Ctrl Pts',(5.68121256712033,6.68619912587697,-7.37946130795072));
#39208=CARTESIAN_POINT('Ctrl Pts',(5.67167699310978,6.69094421653975,-7.38003877455295));
#39209=CARTESIAN_POINT('',(5.732785291682,6.65588487364253,-8.10254503001699));
#39210=CARTESIAN_POINT('',(5.72001552894544,6.64701088376288,-7.3940918491053));
#39211=CARTESIAN_POINT('Origin',(5.898757994352,6.95917605551496,-7.74135737489339));
#39212=CARTESIAN_POINT('',(5.99999998860446,6.44014593005993,-7.42970700294369));
#39213=CARTESIAN_POINT('Ctrl Pts',(6.0000000519944,6.44014606643596,-7.42970716027456));
#39214=CARTESIAN_POINT('Ctrl Pts',(5.95914560525917,6.47968727812811,-7.41730334914713));
#39215=CARTESIAN_POINT('Ctrl Pts',(5.91541907062042,6.51668572949036,-7.40809453517975));
#39216=CARTESIAN_POINT('Ctrl Pts',(5.86878902309971,6.5512055037961,-7.40209476752825));
#39217=CARTESIAN_POINT('Ctrl Pts',(5.82215897558057,6.5857252781007,-7.39609499987695));
#39218=CARTESIAN_POINT('Ctrl Pts',(5.77262518199994,6.61776600827662,-7.39330385120898));
#39219=CARTESIAN_POINT('Ctrl Pts',(5.72001606109489,6.64701181313427,-7.39409288290435));
#39220=CARTESIAN_POINT('',(5.99998738510675,6.09545783229234,-8.13557311354423));
#39221=CARTESIAN_POINT('Ctrl Pts',(5.99998738510675,6.09545783229234,-8.13557311354423));
#39222=CARTESIAN_POINT('Ctrl Pts',(5.99998486187689,6.09906559316439,-8.10752276907166));
#39223=CARTESIAN_POINT('Ctrl Pts',(5.99998575125142,6.10334644784103,-8.07998145178508));
#39224=CARTESIAN_POINT('Ctrl Pts',(5.9999822017205,6.10832836814456,-8.05296723319903));
#39225=CARTESIAN_POINT('Ctrl Pts',(5.99998107889726,6.10990429917679,-8.04442182444348));
#39226=CARTESIAN_POINT('Ctrl Pts',(5.99997928834143,6.11155002495211,-8.03592910458814));
#39227=CARTESIAN_POINT('Ctrl Pts',(5.99997621692443,6.11326554040231,-8.02748944959876));
#39228=CARTESIAN_POINT('Ctrl Pts',(5.99996211490585,6.12114211034623,-7.98873985231655));
#39229=CARTESIAN_POINT('Ctrl Pts',(5.99992503046442,6.13049155468325,-7.95111245217534));
#39230=CARTESIAN_POINT('Ctrl Pts',(5.99991423108089,6.14127675934099,-7.91456073449541));
#39231=CARTESIAN_POINT('Ctrl Pts',(5.99990487784457,6.15061771548782,-7.88290366327844));
#39232=CARTESIAN_POINT('Ctrl Pts',(5.99990278201506,6.16105737414897,-7.85206613788475));
#39233=CARTESIAN_POINT('Ctrl Pts',(5.99990421744016,6.17258775683501,-7.82206010445584));
#39234=CARTESIAN_POINT('Ctrl Pts',(5.99990515161376,6.18009172136025,-7.80253220009007));
#39235=CARTESIAN_POINT('Ctrl Pts',(5.99990793441964,6.18805772979702,-7.78335583843895));
#39236=CARTESIAN_POINT('Ctrl Pts',(5.99991541529791,6.1964933914083,-7.76452783598631));
#39237=CARTESIAN_POINT('Ctrl Pts',(5.99991831505963,6.19976324927403,-7.75722966605576));
#39238=CARTESIAN_POINT('Ctrl Pts',(5.99992637047872,6.20321225211258,-7.74973530638953));
#39239=CARTESIAN_POINT('Ctrl Pts',(5.99993172018384,6.20669887667019,-7.74238903612566));
#39240=CARTESIAN_POINT('Ctrl Pts',(5.99993713803786,6.21022991668828,-7.73494918309393));
#39241=CARTESIAN_POINT('Ctrl Pts',(5.9999395079884,6.21379941178357,-7.72766152244286));
#39242=CARTESIAN_POINT('Ctrl Pts',(5.99994451737609,6.2172087557156,-7.72087231262672));
#39243=CARTESIAN_POINT('Ctrl Pts',(5.99994535116398,6.21777622420938,-7.71974228211494));
#39244=CARTESIAN_POINT('Ctrl Pts',(5.999946292958,6.21833914779861,-7.71862603044698));
#39245=CARTESIAN_POINT('Ctrl Pts',(5.99994741064976,6.21889648704503,-7.71752511762765));
#39246=CARTESIAN_POINT('Ctrl Pts',(5.99997420500938,6.23225754836266,-7.69113299868253));
#39247=CARTESIAN_POINT('Ctrl Pts',(5.99996028565732,6.24653972602933,-7.66574258331808));
#39248=CARTESIAN_POINT('Ctrl Pts',(5.99993572431094,6.26166953382428,-7.64132013235762));
#39249=CARTESIAN_POINT('Ctrl Pts',(5.99991395264974,6.27508089345201,-7.6196715907991));
#39250=CARTESIAN_POINT('Ctrl Pts',(5.99988491856949,6.28915903686546,-7.59878279218735));
#39251=CARTESIAN_POINT('Ctrl Pts',(5.99986830472584,6.30388676844893,-7.57863699716864));
#39252=CARTESIAN_POINT('Ctrl Pts',(5.99985059014737,6.31959027225559,-7.55715646114912));
#39253=CARTESIAN_POINT('Ctrl Pts',(5.9998484739606,6.33603282621633,-7.53651939610242));
#39254=CARTESIAN_POINT('Ctrl Pts',(5.99986814609502,6.3532309144603,-7.51672507359564));
#39255=CARTESIAN_POINT('Ctrl Pts',(5.99988721410734,6.36990085740629,-7.49753862553458));
#39256=CARTESIAN_POINT('Ctrl Pts',(5.99992732030833,6.38728175857388,-7.47914377038259));
#39257=CARTESIAN_POINT('Ctrl Pts',(5.999961045714,6.4054053563925,-7.46157120296813));
#39258=CARTESIAN_POINT('Ctrl Pts',(5.99998205295471,6.41669437648174,-7.4506254145796));
#39259=CARTESIAN_POINT('Ctrl Pts',(5.99999988350857,6.42827183775403,-7.4399993282562));
#39260=CARTESIAN_POINT('Ctrl Pts',(5.99999988745865,6.4401458000223,-7.42970685292513));
#39261=CARTESIAN_POINT('Ctrl Pts',(5.99998738510675,6.09545783229234,-8.13557311354423));
#39262=CARTESIAN_POINT('Ctrl Pts',(5.99998441904533,6.1110792605425,-8.12979435905872));
#39263=CARTESIAN_POINT('Ctrl Pts',(5.9992397470716,6.1278161441473,-8.12408926921516));
#39264=CARTESIAN_POINT('Ctrl Pts',(5.99754903941737,6.14562213733926,-8.1185853568534));
#39265=CARTESIAN_POINT('Ctrl Pts',(5.99682966821598,6.15319832514584,-8.11624352322053));
#39266=CARTESIAN_POINT('Ctrl Pts',(5.995938805942,6.16096762335711,-8.11393846741642));
#39267=CARTESIAN_POINT('Ctrl Pts',(5.99485951760362,6.16892439542041,-8.11168171476116));
#39268=CARTESIAN_POINT('Ctrl Pts',(5.99246751504082,6.18655881107221,-8.10668012441402));
#39269=CARTESIAN_POINT('Ctrl Pts',(5.98914968027009,6.2051168950132,-8.10191432041602));
#39270=CARTESIAN_POINT('Ctrl Pts',(5.98476329171026,6.22450598415262,-8.09751162212164));
#39271=CARTESIAN_POINT('Ctrl Pts',(5.98056287493804,6.2430730249217,-8.09329558710638));
#39272=CARTESIAN_POINT('Ctrl Pts',(5.9753829567149,6.26240242359787,-8.08941218546347));
#39273=CARTESIAN_POINT('Ctrl Pts',(5.9690941845529,6.28237372842147,-8.0859965229583));
#39274=CARTESIAN_POINT('Ctrl Pts',(5.96738487036364,6.28780201137298,-8.08506813181366));
#39275=CARTESIAN_POINT('Ctrl Pts',(5.96559359427533,6.29327747202086,-8.08417444780743));
#39276=CARTESIAN_POINT('Ctrl Pts',(5.96371764308482,6.29879711683061,-8.08331854647735));
#39277=CARTESIAN_POINT('Ctrl Pts',(5.96344414264071,6.29960184208914,-8.08319376210392));
#39278=CARTESIAN_POINT('Ctrl Pts',(5.96316884226125,6.30040750604515,-8.08306978112478));
#39279=CARTESIAN_POINT('Ctrl Pts',(5.96289173650296,6.3012141001333,-8.08294661136472));
#39280=CARTESIAN_POINT('Ctrl Pts',(5.9583064281901,6.31456092699193,-8.08090850386324));
#39281=CARTESIAN_POINT('Ctrl Pts',(5.95322667453022,6.32816314002302,-8.07909218307997));
#39282=CARTESIAN_POINT('Ctrl Pts',(5.94762863024084,6.34197741559306,-8.07753518789005));
#39283=CARTESIAN_POINT('Ctrl Pts',(5.94482960809616,6.34888455337808,-8.07675669029508));
#39284=CARTESIAN_POINT('Ctrl Pts',(5.9419009720458,6.35584469171829,-8.0760430429858));
#39285=CARTESIAN_POINT('Ctrl Pts',(5.93883992577041,6.36285141390253,-8.07539941117091));
#39286=CARTESIAN_POINT('Ctrl Pts',(5.93730940263271,6.36635477499465,-8.07507759526346));
#39287=CARTESIAN_POINT('Ctrl Pts',(5.93574577369783,6.36986978092234,-8.07477328464124));
#39288=CARTESIAN_POINT('Ctrl Pts',(5.93414868582103,6.37339558875165,-8.07448714829654));
#39289=CARTESIAN_POINT('Ctrl Pts',(5.93308462461123,6.37574466133484,-8.07429650970393));
#39290=CARTESIAN_POINT('Ctrl Pts',(5.93173682852077,6.37868274802833,-8.07406994874411));
#39291=CARTESIAN_POINT('Ctrl Pts',(5.93064071574464,6.38104120075807,-8.07389688260559));
#39292=CARTESIAN_POINT('Ctrl Pts',(5.93009163329116,6.38222263485816,-8.07381018753003));
#39293=CARTESIAN_POINT('Ctrl Pts',(5.92960659975964,6.38325892810984,-8.07373631728435));
#39294=CARTESIAN_POINT('Ctrl Pts',(5.9292566846022,6.38400455129654,-8.0736839462418));
#39295=CARTESIAN_POINT('Ctrl Pts',(5.92324504417235,6.39681456652238,-8.07278419705961));
#39296=CARTESIAN_POINT('Ctrl Pts',(5.91644349452928,6.41051100296279,-8.07208320363119));
#39297=CARTESIAN_POINT('Ctrl Pts',(5.90871320068971,6.42498790319228,-8.07170835271769));
#39298=CARTESIAN_POINT('Ctrl Pts',(5.90756565183023,6.42713697419681,-8.07165270674262));
#39299=CARTESIAN_POINT('Ctrl Pts',(5.90639762303351,6.42930316709509,-8.07160429984891));
#39300=CARTESIAN_POINT('Ctrl Pts',(5.90520864691648,6.43148605064041,-8.07156360519117));
#39301=CARTESIAN_POINT('Ctrl Pts',(5.89737763223853,6.44586328903806,-8.07129557586956));
#39302=CARTESIAN_POINT('Ctrl Pts',(5.8886373033292,6.46096801579065,-8.0713603304539));
#39303=CARTESIAN_POINT('Ctrl Pts',(5.8788707448158,6.476664087043,-8.07189275843248));
#39304=CARTESIAN_POINT('Ctrl Pts',(5.86988435735373,6.49110632662129,-8.07238265506339));
#39305=CARTESIAN_POINT('Ctrl Pts',(5.86002898431128,6.50604936554337,-8.07326842358738));
#39306=CARTESIAN_POINT('Ctrl Pts',(5.84922135971914,6.5213497229377,-8.07467428281701));
#39307=CARTESIAN_POINT('Ctrl Pts',(5.84083256968025,6.53322573552555,-8.07576549928192));
#39308=CARTESIAN_POINT('Ctrl Pts',(5.83187018337614,6.54531643423985,-8.07717034591712));
#39309=CARTESIAN_POINT('Ctrl Pts',(5.82229986758076,6.55753571914848,-8.07895670244825));
#39310=CARTESIAN_POINT('Ctrl Pts',(5.81046703764842,6.57264375981402,-8.08116537073919));
#39311=CARTESIAN_POINT('Ctrl Pts',(5.79770346605293,6.58794939970163,-8.08395721212972));
#39312=CARTESIAN_POINT('Ctrl Pts',(5.7839788211146,6.60327161378152,-8.08745539557388));
#39313=CARTESIAN_POINT('Ctrl Pts',(5.77112680734696,6.61761962112088,-8.09073115986419));
#39314=CARTESIAN_POINT('Ctrl Pts',(5.75743192856449,6.63198234755227,-8.09462614689545));
#39315=CARTESIAN_POINT('Ctrl Pts',(5.74289151150233,6.64617322509536,-8.09925657783635));
#39316=CARTESIAN_POINT('Ctrl Pts',(5.73956595888168,6.64941883420004,-8.10031560810243));
#39317=CARTESIAN_POINT('Ctrl Pts',(5.7361962789524,6.65265528125112,-8.10141318019669));
#39318=CARTESIAN_POINT('Ctrl Pts',(5.73278262922815,6.65588001261884,-8.10255081990868));
#39319=CARTESIAN_POINT('Ctrl Pts',(5.99928507670221,9.87990142103655,-16.9962137655509));
#39320=CARTESIAN_POINT('Ctrl Pts',(5.99928507670221,9.88326637139441,-16.9632224657788));
#39321=CARTESIAN_POINT('Ctrl Pts',(5.99928507670221,9.93380713709435,-16.4417148893617));
#39322=CARTESIAN_POINT('Ctrl Pts',(5.99928507670221,9.95153405412758,-15.4241459871747));
#39323=CARTESIAN_POINT('Ctrl Pts',(5.99928507670221,9.75855490567037,-13.9623406694731));
#39324=CARTESIAN_POINT('Ctrl Pts',(5.99928507670221,9.35132588134331,-12.5448516866735));
#39325=CARTESIAN_POINT('Ctrl Pts',(5.99928507670221,8.73824250065081,-11.2027103817564));
#39326=CARTESIAN_POINT('Ctrl Pts',(5.99928507670221,7.93284474685238,-9.96535729518426));
#39327=CARTESIAN_POINT('Ctrl Pts',(5.99928507670221,7.00873360046685,-8.92486257056714));
#39328=CARTESIAN_POINT('Ctrl Pts',(5.99928507670221,6.32620211116035,-8.33936238043742));
#39329=CARTESIAN_POINT('Ctrl Pts',(5.99928507670221,6.00174809856699,-8.09410015407363));
#39330=CARTESIAN_POINT('Ctrl Pts',(6.01063087509513,10.0684345307133,-17.01545949762));
#39331=CARTESIAN_POINT('Ctrl Pts',(6.01063087509513,10.0718639576454,-16.9818342056501));
#39332=CARTESIAN_POINT('Ctrl Pts',(6.01063087509513,10.1233733290156,-16.4503125276442));
#39333=CARTESIAN_POINT('Ctrl Pts',(6.01063087509513,10.1414447974272,-15.4134144215648));
#39334=CARTESIAN_POINT('Ctrl Pts',(6.01063087509513,9.94474509956266,-13.9234401354667));
#39335=CARTESIAN_POINT('Ctrl Pts',(6.01063087509513,9.52975918464545,-12.4789637137856));
#39336=CARTESIAN_POINT('Ctrl Pts',(6.01063087509513,8.90489167184337,-11.1110056648205));
#39337=CARTESIAN_POINT('Ctrl Pts',(6.01063087509513,8.08411518316363,-9.85004045908981));
#39338=CARTESIAN_POINT('Ctrl Pts',(6.01063087509513,7.14224990779624,-8.78954725626183));
#39339=CARTESIAN_POINT('Ctrl Pts',(6.01063087509513,6.44671813919453,-8.19289533345759));
#39340=CARTESIAN_POINT('Ctrl Pts',(6.01063087509513,6.11602421034097,-7.94291818409647));
#39341=CARTESIAN_POINT('Ctrl Pts',(5.90351530093621,10.2248493207515,-17.0314265452415));
#39342=CARTESIAN_POINT('Ctrl Pts',(5.90351530093621,10.2283322400939,-16.9972752673821));
#39343=CARTESIAN_POINT('Ctrl Pts',(5.90351530093621,10.280645206398,-16.4574454805172));
#39344=CARTESIAN_POINT('Ctrl Pts',(5.90351530093621,10.2990025287459,-15.4045110751714));
#39345=CARTESIAN_POINT('Ctrl Pts',(5.90351530093621,10.0992161106988,-13.8911666590971));
#39346=CARTESIAN_POINT('Ctrl Pts',(5.90351530093621,9.6777947616339,-12.4243003527319));
#39347=CARTESIAN_POINT('Ctrl Pts',(5.90351530093621,9.04315065015506,-11.0349236754524));
#39348=CARTESIAN_POINT('Ctrl Pts',(5.90351530093621,8.20961533311243,-9.75436888852781));
#39349=CARTESIAN_POINT('Ctrl Pts',(5.90351530093621,7.25302050514079,-8.67728412904822));
#39350=CARTESIAN_POINT('Ctrl Pts',(5.90351530093621,6.54670317234504,-8.07138027204041));
#39351=CARTESIAN_POINT('Ctrl Pts',(5.90351530093621,6.21083235337873,-7.81749142944129));
#39352=CARTESIAN_POINT('Ctrl Pts',(5.72195027506538,10.2826708065042,-17.0373290459966));
#39353=CARTESIAN_POINT('Ctrl Pts',(5.72195027506538,10.2861735002605,-17.0029833281784));
#39354=CARTESIAN_POINT('Ctrl Pts',(5.72195027506538,10.3387835296056,-16.4600823023492));
#39355=CARTESIAN_POINT('Ctrl Pts',(5.72195027506538,10.3572465229012,-15.4012197961528));
#39356=CARTESIAN_POINT('Ctrl Pts',(5.72195027506538,10.1563190443011,-13.8792361993662));
#39357=CARTESIAN_POINT('Ctrl Pts',(5.72195027506538,9.73251872350333,-12.4040930772462));
#39358=CARTESIAN_POINT('Ctrl Pts',(5.72195027506538,9.0942605199016,-11.0067986262652));
#39359=CARTESIAN_POINT('Ctrl Pts',(5.72195027506538,8.25600867693205,-9.71900220515771));
#39360=CARTESIAN_POINT('Ctrl Pts',(5.72195027506538,7.29396881005966,-8.63578408414143));
#39361=CARTESIAN_POINT('Ctrl Pts',(5.72195027506538,6.58366440323806,-8.02646008648023));
#39362=CARTESIAN_POINT('Ctrl Pts',(5.72195027506538,6.24587985554049,-7.77112521748877));
#39363=CARTESIAN_POINT('',(6.,9.9133032909571,-16.8993688494793));
#39364=CARTESIAN_POINT('Ctrl Pts',(5.99999999999975,9.9133032909571,-16.8993688494793));
#39365=CARTESIAN_POINT('Ctrl Pts',(5.99999999999975,9.92726798889229,-16.7473133675693));
#39366=CARTESIAN_POINT('Ctrl Pts',(6.00000000003748,9.93769911293785,-16.5954478952856));
#39367=CARTESIAN_POINT('Ctrl Pts',(5.99999999795225,9.94464893033857,-16.4436798521367));
#39368=CARTESIAN_POINT('Ctrl Pts',(5.9999999958601,9.95162180848309,-16.2914082153307));
#39369=CARTESIAN_POINT('Ctrl Pts',(5.99999999148619,9.95509022596526,-16.139234192407));
#39370=CARTESIAN_POINT('Ctrl Pts',(5.9999999908736,9.95505464932154,-15.9870605228147));
#39371=CARTESIAN_POINT('Ctrl Pts',(5.999999990262,9.95501913067149,-15.8351349123105));
#39372=CARTESIAN_POINT('Ctrl Pts',(5.99999999695627,9.9514910077271,-15.6832091914971));
#39373=CARTESIAN_POINT('Ctrl Pts',(5.99999999953315,9.94441902101537,-15.5311897728051));
#39374=CARTESIAN_POINT('Ctrl Pts',(5.99999999982105,9.94362890698645,-15.5142054824956));
#39375=CARTESIAN_POINT('Ctrl Pts',(5.99999999999975,9.94279450412573,-15.497220030147));
#39376=CARTESIAN_POINT('Ctrl Pts',(5.99999999999975,9.9419157008945,-15.4802332916842));
#39377=CARTESIAN_POINT('Ctrl Pts',(5.99999999999975,9.94094263422146,-15.4614244975257));
#39378=CARTESIAN_POINT('Ctrl Pts',(5.99999999977976,9.93991612339977,-15.4426140377054));
#39379=CARTESIAN_POINT('Ctrl Pts',(5.99999999940214,9.93883607995432,-15.4238025173435));
#39380=CARTESIAN_POINT('Ctrl Pts',(5.99999999572736,9.92832587000923,-15.2407422624791));
#39381=CARTESIAN_POINT('Ctrl Pts',(5.99999998184258,9.91274193221338,-15.057581311491));
#39382=CARTESIAN_POINT('Ctrl Pts',(5.99999998033336,9.89208012672901,-14.8748206135648));
#39383=CARTESIAN_POINT('Ctrl Pts',(5.99999997882273,9.8713991178155,-14.6918900547755));
#39384=CARTESIAN_POINT('Ctrl Pts',(5.99999998731005,9.84563081442832,-14.5093609439596));
#39385=CARTESIAN_POINT('Ctrl Pts',(5.99999999411988,9.8148232071059,-14.3277348674503));
#39386=CARTESIAN_POINT('Ctrl Pts',(5.99999999739303,9.80001548195328,-14.2404360067062));
#39387=CARTESIAN_POINT('Ctrl Pts',(5.99999999999975,9.78404431694916,-14.153345716758));
#39388=CARTESIAN_POINT('Ctrl Pts',(5.99999999999975,9.76691929497133,-14.0665191605846));
#39389=CARTESIAN_POINT('Ctrl Pts',(5.99999999999975,9.76020616508213,-14.0324825356869));
#39390=CARTESIAN_POINT('Ctrl Pts',(5.99999999960415,9.75331447298792,-13.9984866912186));
#39391=CARTESIAN_POINT('Ctrl Pts',(5.99999999898866,9.74624448648212,-13.9645326289129));
#39392=CARTESIAN_POINT('Ctrl Pts',(5.99999999507861,9.70133035239358,-13.7488296277829));
#39393=CARTESIAN_POINT('Ctrl Pts',(5.99999998615656,9.64922498996124,-13.5348122190641));
#39394=CARTESIAN_POINT('Ctrl Pts',(5.99999998771986,9.59004136500335,-13.3227629515009));
#39395=CARTESIAN_POINT('Ctrl Pts',(5.99999998928315,9.53085774004545,-13.1107136839378));
#39396=CARTESIAN_POINT('Ctrl Pts',(5.99999999999975,9.46459569652831,-12.900631951729));
#39397=CARTESIAN_POINT('Ctrl Pts',(5.99999999999975,9.39131591670037,-12.6928136411459));
#39398=CARTESIAN_POINT('Ctrl Pts',(5.99999999999975,9.3745538773706,-12.645277216997));
#39399=CARTESIAN_POINT('Ctrl Pts',(5.9999999993467,9.35742705664761,-12.5978581952024));
#39400=CARTESIAN_POINT('Ctrl Pts',(5.99999999845574,9.3399373333427,-12.5505645602474));
#39401=CARTESIAN_POINT('Ctrl Pts',(5.99999999449763,9.26223848888796,-12.3404605624882));
#39402=CARTESIAN_POINT('Ctrl Pts',(5.99999998895133,9.17737337514935,-12.1328324811753));
#39403=CARTESIAN_POINT('Ctrl Pts',(5.99999999115154,9.08561278925283,-11.9283201471139));
#39404=CARTESIAN_POINT('Ctrl Pts',(5.99999999312721,9.00321675921052,-11.7446791616438));
#39405=CARTESIAN_POINT('Ctrl Pts',(5.99999999999975,8.91526165194371,-11.5635505237571));
#39406=CARTESIAN_POINT('Ctrl Pts',(5.99999999999975,8.82197656077892,-11.3853836320773));
#39407=CARTESIAN_POINT('Ctrl Pts',(5.99999999999975,8.79096317958254,-11.3261506114601));
#39408=CARTESIAN_POINT('Ctrl Pts',(5.99999999913628,8.7593588482401,-11.2672464903642));
#39409=CARTESIAN_POINT('Ctrl Pts',(5.99999999780776,8.72716730813645,-11.2086786366005));
#39410=CARTESIAN_POINT('Ctrl Pts',(5.99999999336884,8.6196079425489,-11.0129899191807));
#39411=CARTESIAN_POINT('Ctrl Pts',(5.99999998477715,8.50549634900011,-10.8210529986896));
#39412=CARTESIAN_POINT('Ctrl Pts',(5.99999998688354,8.38499562042057,-10.6331552723254));
#39413=CARTESIAN_POINT('Ctrl Pts',(5.99999998863009,8.28508034958788,-10.477356610858));
#39414=CARTESIAN_POINT('Ctrl Pts',(5.99999999999975,8.18077151927019,-10.3243353045956));
#39415=CARTESIAN_POINT('Ctrl Pts',(5.99999999999975,8.07214108602125,-10.1742724294256));
#39416=CARTESIAN_POINT('Ctrl Pts',(5.99999999999975,8.02304710815971,-10.1064536492633));
#39417=CARTESIAN_POINT('Ctrl Pts',(5.99999999683356,7.97307828550649,-10.0392309360628));
#39418=CARTESIAN_POINT('Ctrl Pts',(5.99999999319076,7.92225874095039,-9.9726436577022));
#39419=CARTESIAN_POINT('Ctrl Pts',(5.99999998466668,7.8033417060917,-9.81683034274397));
#39420=CARTESIAN_POINT('Ctrl Pts',(5.9999999759598,7.67976357121808,-9.66449894127245));
#39421=CARTESIAN_POINT('Ctrl Pts',(5.99999997954455,7.55191355600678,-9.51606320039813));
#39422=CARTESIAN_POINT('Ctrl Pts',(5.9999999831293,7.42406354079548,-9.36762745952381));
#39423=CARTESIAN_POINT('Ctrl Pts',(5.99999999999975,7.29194203564635,-9.22308774629525));
#39424=CARTESIAN_POINT('Ctrl Pts',(5.99999999999975,7.15597859955101,-9.08281763782801));
#39425=CARTESIAN_POINT('Ctrl Pts',(5.99999999999975,7.08650989506377,-9.01114849652541));
#39426=CARTESIAN_POINT('Ctrl Pts',(5.99999999545169,7.0160267676778,-8.94061363520937));
#39427=CARTESIAN_POINT('Ctrl Pts',(5.99999999307294,6.94451383265442,-8.87118228508652));
#39428=CARTESIAN_POINT('Ctrl Pts',(5.9999999894094,6.83437642276922,-8.76425073396415));
#39429=CARTESIAN_POINT('Ctrl Pts',(5.99999999031164,6.72179810473437,-8.65993478356875));
#39430=CARTESIAN_POINT('Ctrl Pts',(5.99999999276244,6.60672174345137,-8.55816514811733));
#39431=CARTESIAN_POINT('Ctrl Pts',(5.99999999520029,6.4922534941214,-8.45693330627604));
#39432=CARTESIAN_POINT('Ctrl Pts',(5.99999999786784,6.37531319152282,-8.35822062896864));
#39433=CARTESIAN_POINT('Ctrl Pts',(5.99999999875695,6.25581047945977,-8.26199732529102));
#39434=CARTESIAN_POINT('Ctrl Pts',(5.99999999915085,6.20286622544753,-8.21936673604451));
#39435=CARTESIAN_POINT('Ctrl Pts',(5.99999999931877,6.14941859523291,-8.17722530242187));
#39436=CARTESIAN_POINT('Ctrl Pts',(5.99999999931449,6.09545783381438,-8.1355731127727));
#39437=CARTESIAN_POINT('',(5.73644276520417,10.287735094912,-16.9337809954845));
#39438=CARTESIAN_POINT('Origin',(5.6,9.91330329093393,-16.8993688493888));
#39439=CARTESIAN_POINT('Ctrl Pts',(5.73644276397747,10.2877350956482,-16.9337809951853));
#39440=CARTESIAN_POINT('Ctrl Pts',(5.73708792252488,10.3280497910532,-16.4922345426347));
#39441=CARTESIAN_POINT('Ctrl Pts',(5.7376256311147,10.3398885430833,-16.0482066703703));
#39442=CARTESIAN_POINT('Ctrl Pts',(5.73805595543757,10.3232537068247,-15.6057356194698));
#39443=CARTESIAN_POINT('Ctrl Pts',(5.73812189675439,10.3207046456871,-15.5379329827125));
#39444=CARTESIAN_POINT('Ctrl Pts',(5.73818531651987,10.3174869811684,-15.4701668027555));
#39445=CARTESIAN_POINT('Ctrl Pts',(5.73824621494101,10.3136007167544,-15.4024515020653));
#39446=CARTESIAN_POINT('Ctrl Pts',(5.73865147313059,10.2877389546408,-14.9518293077615));
#39447=CARTESIAN_POINT('Ctrl Pts',(5.7389450772283,10.2322696006654,-14.503464432552));
#39448=CARTESIAN_POINT('Ctrl Pts',(5.73912707304533,10.1478940723348,-14.0611488527984));
#39449=CARTESIAN_POINT('Ctrl Pts',(5.73915087280122,10.1368602089777,-14.0033068485553));
#39450=CARTESIAN_POINT('Ctrl Pts',(5.73917276389785,10.1253320034285,-13.9455682225513));
#39451=CARTESIAN_POINT('Ctrl Pts',(5.73919274639698,10.1133110090545,-13.8879413913271));
#39452=CARTESIAN_POINT('Ctrl Pts',(5.73934700322873,10.0205137821125,-13.4430855026459));
#39453=CARTESIAN_POINT('Ctrl Pts',(5.73938752575328,9.8983518130802,-13.0048956732406));
#39454=CARTESIAN_POINT('Ctrl Pts',(5.73931432088869,9.74808603084931,-12.5770820026694));
#39455=CARTESIAN_POINT('Ctrl Pts',(5.73930537010441,9.72971298134816,-12.524773076246));
#39456=CARTESIAN_POINT('Ctrl Pts',(5.73929471904359,9.71091975480985,-12.4726192145084));
#39457=CARTESIAN_POINT('Ctrl Pts',(5.73928236767902,9.6917086361614,-12.4206271498742));
#39458=CARTESIAN_POINT('Ctrl Pts',(5.73918135761153,9.53459916217931,-11.9954334859653));
#39459=CARTESIAN_POINT('Ctrl Pts',(5.73896663330746,9.34954312181862,-11.5810645646298));
#39460=CARTESIAN_POINT('Ctrl Pts',(5.73863815941398,9.13842847138387,-11.181029202796));
#39461=CARTESIAN_POINT('Ctrl Pts',(5.73859603622718,9.11135532483154,-11.1297290398053));
#39462=CARTESIAN_POINT('Ctrl Pts',(5.73855204235336,9.08385360099182,-11.0786645361034));
#39463=CARTESIAN_POINT('Ctrl Pts',(5.73850617767971,9.05592724924063,-11.0278430391023));
#39464=CARTESIAN_POINT('Ctrl Pts',(5.73815298354927,8.84087233358326,-10.636477462656));
#39465=CARTESIAN_POINT('Ctrl Pts',(5.73768884857257,8.60063848073488,-10.2595258684371));
#39466=CARTESIAN_POINT('Ctrl Pts',(5.73711370894741,8.33732017512975,-9.90009892045526));
#39467=CARTESIAN_POINT('Ctrl Pts',(5.73703020601639,8.29908971882023,-9.8479147162477));
#39468=CARTESIAN_POINT('Ctrl Pts',(5.73694436301577,8.26037260623242,-9.79609985173272));
#39469=CARTESIAN_POINT('Ctrl Pts',(5.73685617976038,8.22117519680522,-9.74466378006768));
#39470=CARTESIAN_POINT('Ctrl Pts',(5.73622837043537,7.94211429067454,-9.37847129499271));
#39471=CARTESIAN_POINT('Ctrl Pts',(5.73548194360524,7.6387126294289,-9.03148082705006));
#39472=CARTESIAN_POINT('Ctrl Pts',(5.73461683428776,7.31393910142934,-8.70646898025495));
#39473=CARTESIAN_POINT('Ctrl Pts',(5.73452245153485,7.27850656241392,-8.6710104408445));
#39474=CARTESIAN_POINT('Ctrl Pts',(5.73442665616088,7.2428196026404,-8.63581347234199));
#39475=CARTESIAN_POINT('Ctrl Pts',(5.73432944809515,7.20688204886513,-8.60088165646185));
#39476=CARTESIAN_POINT('Ctrl Pts',(5.73384873467085,7.02916362182739,-8.42813680547361));
#39477=CARTESIAN_POINT('Ctrl Pts',(5.73333347356617,6.84531724366401,-8.26187651448214));
#39478=CARTESIAN_POINT('Ctrl Pts',(5.73278365817643,6.65588188893571,-8.10254858487398));
#39479=CARTESIAN_POINT('Ctrl Pts',(5.99999999997502,9.67862872910777,-17.034853315691));
#39480=CARTESIAN_POINT('Ctrl Pts',(5.99999999997502,9.75700380810234,-16.9899528681557));
#39481=CARTESIAN_POINT('Ctrl Pts',(5.99999999997502,9.83522889702098,-16.9447896029538));
#39482=CARTESIAN_POINT('Ctrl Pts',(5.99999999997502,9.91330177297949,-16.8993645966845));
#39483=CARTESIAN_POINT('Ctrl Pts',(6.00000263486395,9.79664482225177,-17.2408547729095));
#39484=CARTESIAN_POINT('Ctrl Pts',(6.00000263486394,9.87548026830594,-17.1956905812719));
#39485=CARTESIAN_POINT('Ctrl Pts',(6.00000263486394,9.95416475310123,-17.1502620839831));
#39486=CARTESIAN_POINT('Ctrl Pts',(6.00000263486394,10.0326962223333,-17.1045702551542));
#39487=CARTESIAN_POINT('Ctrl Pts',(5.83074066841807,9.87940002138452,-17.3853070349662));
#39488=CARTESIAN_POINT('Ctrl Pts',(5.83074066841807,9.95855828584937,-17.3399579007904));
#39489=CARTESIAN_POINT('Ctrl Pts',(5.83074066841807,10.0375649080452,-17.2943434175634));
#39490=CARTESIAN_POINT('Ctrl Pts',(5.83074066841807,10.1164179518752,-17.2484644875228));
#39491=CARTESIAN_POINT('Ctrl Pts',(5.59336110044111,9.87744127562583,-17.3818879717702));
#39492=CARTESIAN_POINT('Ctrl Pts',(5.5933611004411,9.95659189925281,-17.336543215031));
#39493=CARTESIAN_POINT('Ctrl Pts',(5.5933611004411,10.0355908967276,-17.2909331339334));
#39494=CARTESIAN_POINT('Ctrl Pts',(5.59336110044111,10.1144363291584,-17.2450586324212));
#39495=CARTESIAN_POINT('',(5.99999999995607,9.6786359708514,-17.0348513552255));
#39496=CARTESIAN_POINT('',(5.59336167792738,9.87744147097414,-17.3818877029268));
#39497=CARTESIAN_POINT('Origin',(5.6,9.67863108576213,-17.0348569102136));
#39498=CARTESIAN_POINT('',(5.59336169562615,10.114435612724,-17.2450590602278));
#39499=CARTESIAN_POINT('Origin',(5.59336169593387,7.59771250744744,-13.0386810382369));
#39500=CARTESIAN_POINT('Origin',(5.6,9.9133032910197,-16.8993688495356));
#39501=CARTESIAN_POINT('Ctrl Pts',(5.99999999999158,9.67863900758284,-17.0348496155196));
#39502=CARTESIAN_POINT('Ctrl Pts',(5.99999999999163,9.70480912503784,-17.0198569671163));
#39503=CARTESIAN_POINT('Ctrl Pts',(5.99999999999965,9.73095807855235,-17.0048396407998));
#39504=CARTESIAN_POINT('Ctrl Pts',(5.99999999999965,9.75705557048624,-16.9898117781375));
#39505=CARTESIAN_POINT('Ctrl Pts',(5.99999999999965,9.78315306242015,-16.9747839154753));
#39506=CARTESIAN_POINT('Ctrl Pts',(5.99999999999965,9.80919909277344,-16.9597455164675));
#39507=CARTESIAN_POINT('Ctrl Pts',(5.99999999999965,9.83523570690332,-16.9446741822047));
#39508=CARTESIAN_POINT('Ctrl Pts',(5.99999999999965,9.86127232103318,-16.9296028479419));
#39509=CARTESIAN_POINT('Ctrl Pts',(5.99999999999965,9.88729951893964,-16.9144985784241));
#39510=CARTESIAN_POINT('Ctrl Pts',(5.99999999999965,9.9133032909571,-16.8993688494793));
#39511=CARTESIAN_POINT('Origin',(5.6,9.91330329093393,-16.8993688493888));
#39512=CARTESIAN_POINT('Origin',(5.600000004205,9.91330328921885,-16.89936884964));
#39513=CARTESIAN_POINT('Ctrl Pts',(-5.69266449220542,10.0630786776781,-17.2766466781631));
#39514=CARTESIAN_POINT('Ctrl Pts',(-5.65790043414258,10.0769849565476,-17.2678633469364));
#39515=CARTESIAN_POINT('Ctrl Pts',(-5.5437267087947,10.1222517047768,-17.2393085839034));
#39516=CARTESIAN_POINT('Ctrl Pts',(-5.34117223040521,10.2002049877122,-17.1903129318253));
#39517=CARTESIAN_POINT('Ctrl Pts',(-5.07577265985758,10.297830631585,-17.1291595099684));
#39518=CARTESIAN_POINT('Ctrl Pts',(-4.78281831444695,10.4000147575524,-17.0653012548397));
#39519=CARTESIAN_POINT('Ctrl Pts',(-4.459303684198,10.5059980087032,-16.9991848074578));
#39520=CARTESIAN_POINT('Ctrl Pts',(-4.10061258277721,10.6150315669163,-16.9312623156144));
#39521=CARTESIAN_POINT('Ctrl Pts',(-3.70134336606163,10.7258673035538,-16.8623066013417));
#39522=CARTESIAN_POINT('Ctrl Pts',(-3.25666787469216,10.8361817865208,-16.7937662678905));
#39523=CARTESIAN_POINT('Ctrl Pts',(-2.76258823483561,10.9424713829379,-16.7278268451725));
#39524=CARTESIAN_POINT('Ctrl Pts',(-2.21451513067802,11.0403077748057,-16.6672462944136));
#39525=CARTESIAN_POINT('Ctrl Pts',(-1.60542524853154,11.1242578061128,-16.6153980051002));
#39526=CARTESIAN_POINT('Ctrl Pts',(-0.938874874821314,11.1858352943571,
-16.5775066099776));
#39527=CARTESIAN_POINT('Ctrl Pts',(-0.236583627876225,11.2158495117354,
-16.5591684729001));
#39528=CARTESIAN_POINT('Ctrl Pts',(0.464299974377318,11.2096961977306,-16.5629105136066));
#39529=CARTESIAN_POINT('Ctrl Pts',(1.12891944157671,11.1708591884219,-16.5867080644657));
#39530=CARTESIAN_POINT('Ctrl Pts',(1.7341925532243,11.1079134256571,-16.6254836732421));
#39531=CARTESIAN_POINT('Ctrl Pts',(2.27383258279207,11.0299199389491,-16.6736769266626));
#39532=CARTESIAN_POINT('Ctrl Pts',(2.75210078338438,10.9437404518917,-16.7270452561121));
#39533=CARTESIAN_POINT('Ctrl Pts',(3.17956543253272,10.853147213274,-16.7832390598775));
#39534=CARTESIAN_POINT('Ctrl Pts',(3.5623527668001,10.7611441717712,-16.8403830088143));
#39535=CARTESIAN_POINT('Ctrl Pts',(3.90389408990394,10.6703808055596,-16.8968212209322));
#39536=CARTESIAN_POINT('Ctrl Pts',(4.20698802429124,10.5830107962021,-16.9512062257095));
#39537=CARTESIAN_POINT('Ctrl Pts',(4.47552839545299,10.5002685691408,-17.0027635436686));
#39538=CARTESIAN_POINT('Ctrl Pts',(4.71437785352944,10.4224860455875,-17.0512827690776));
#39539=CARTESIAN_POINT('Ctrl Pts',(4.92834708065183,10.3494750576525,-17.0968803214851));
#39540=CARTESIAN_POINT('Ctrl Pts',(5.12117811678946,10.2809937453109,-17.1397088463255));
#39541=CARTESIAN_POINT('Ctrl Pts',(5.29544566343547,10.2169300062458,-17.1798421134489));
#39542=CARTESIAN_POINT('Ctrl Pts',(5.45302101893722,10.157239981754,-17.2173121704573));
#39543=CARTESIAN_POINT('Ctrl Pts',(5.58355363523492,10.1064790825782,-17.2492564746078));
#39544=CARTESIAN_POINT('Ctrl Pts',(5.66171595239179,10.0754576838054,-17.2688281128496));
#39545=CARTESIAN_POINT('Ctrl Pts',(5.69263813280236,10.0630831778572,-17.2766441366971));
#39546=CARTESIAN_POINT('Ctrl Pts',(-5.75649847130068,10.1846663672687,-17.2128693097372));
#39547=CARTESIAN_POINT('Ctrl Pts',(-5.72140233477174,10.1986663653251,-17.2039323534534));
#39548=CARTESIAN_POINT('Ctrl Pts',(-5.60613809903996,10.2442347264077,-17.1748721512905));
#39549=CARTESIAN_POINT('Ctrl Pts',(-5.40164464106496,10.3226877205043,-17.1249718090535));
#39550=CARTESIAN_POINT('Ctrl Pts',(-5.13367468755091,10.4209044324657,-17.0626072240043));
#39551=CARTESIAN_POINT('Ctrl Pts',(-4.83782850255198,10.5236835645344,-16.9974065461764));
#39552=CARTESIAN_POINT('Ctrl Pts',(-4.51104444500548,10.6302690096379,-16.9298277212577));
#39553=CARTESIAN_POINT('Ctrl Pts',(-4.1486314623029,10.7399132384906,-16.8603335925331));
#39554=CARTESIAN_POINT('Ctrl Pts',(-3.74510048327725,10.8513637000167,-16.7897128297027));
#39555=CARTESIAN_POINT('Ctrl Pts',(-3.29553742458152,10.962283478546,-16.7194451614527));
#39556=CARTESIAN_POINT('Ctrl Pts',(-2.7958661187274,11.0691454406598,-16.6517671786418));
#39557=CARTESIAN_POINT('Ctrl Pts',(-2.24141575844614,11.1674897314513,-16.5895078340631));
#39558=CARTESIAN_POINT('Ctrl Pts',(-1.62506220435505,11.2518450143852,-16.5361367827504));
#39559=CARTESIAN_POINT('Ctrl Pts',(-0.950407621639583,11.3136805721432,
-16.4970514102802));
#39560=CARTESIAN_POINT('Ctrl Pts',(-0.239487242992564,11.3437787953034,
-16.4780680325047));
#39561=CARTESIAN_POINT('Ctrl Pts',(0.470002985040156,11.3376139729618,-16.481950388767));
#39562=CARTESIAN_POINT('Ctrl Pts',(1.14277369818418,11.298645972153,-16.5065505464812));
#39563=CARTESIAN_POINT('Ctrl Pts',(1.75537383649425,11.2354239707746,-16.546524035722));
#39564=CARTESIAN_POINT('Ctrl Pts',(2.30142541400522,11.1570481890557,-16.596117814153));
#39565=CARTESIAN_POINT('Ctrl Pts',(2.78525130109912,11.070420416641,-16.650960905252));
#39566=CARTESIAN_POINT('Ctrl Pts',(3.21756581506068,10.9793406103684,-16.7086420451774));
#39567=CARTESIAN_POINT('Ctrl Pts',(3.60459046008406,10.8868345951884,-16.7672410214692));
#39568=CARTESIAN_POINT('Ctrl Pts',(3.94982144119845,10.7955698330654,-16.825065578703));
#39569=CARTESIAN_POINT('Ctrl Pts',(4.25611430913495,10.7077133982218,-16.8807415416324));
#39570=CARTESIAN_POINT('Ctrl Pts',(4.52742836500013,10.6245066330647,-16.9334823385126));
#39571=CARTESIAN_POINT('Ctrl Pts',(4.76869700926165,10.5462824671219,-16.9830781635062));
#39572=CARTESIAN_POINT('Ctrl Pts',(4.98479617406326,10.4728502980132,-17.0296522864356));
#39573=CARTESIAN_POINT('Ctrl Pts',(5.17951842452041,10.4039652420616,-17.0733639174592));
#39574=CARTESIAN_POINT('Ctrl Pts',(5.35547481853325,10.3395129283266,-17.1142914029171));
#39575=CARTESIAN_POINT('Ctrl Pts',(5.51456432417527,10.2794482765431,-17.1524714666152));
#39576=CARTESIAN_POINT('Ctrl Pts',(5.6463454610272,10.2283569966615,-17.1849961244044));
#39577=CARTESIAN_POINT('Ctrl Pts',(5.725254241073,10.1971289896351,-17.2049142863281));
#39578=CARTESIAN_POINT('Ctrl Pts',(5.75647140922376,10.1846721566233,-17.2128686091087));
#39579=CARTESIAN_POINT('Ctrl Pts',(-5.81361946724638,10.2517345378954,-17.0898695141078));
#39580=CARTESIAN_POINT('Ctrl Pts',(-5.77819683786477,10.2657915777574,-17.0808120712885));
#39581=CARTESIAN_POINT('Ctrl Pts',(-5.66186464174654,10.3115378871638,-17.0513579268557));
#39582=CARTESIAN_POINT('Ctrl Pts',(-5.45549338217626,10.3902536999524,-17.0007658028942));
#39583=CARTESIAN_POINT('Ctrl Pts',(-5.18505974968072,10.4887222308117,-16.9374961909567));
#39584=CARTESIAN_POINT('Ctrl Pts',(-4.88646802673155,10.5917039029127,-16.8713094772743));
#39585=CARTESIAN_POINT('Ctrl Pts',(-4.55661094832552,10.698450768387,-16.8026713211113));
#39586=CARTESIAN_POINT('Ctrl Pts',(-4.19073768336938,10.8082203686742,-16.7320525697056));
#39587=CARTESIAN_POINT('Ctrl Pts',(-3.78329110953657,10.9197603181983,-16.6602542945024));
#39588=CARTESIAN_POINT('Ctrl Pts',(-3.32929383344923,11.0307292683044,-16.588779762711));
#39589=CARTESIAN_POINT('Ctrl Pts',(-2.82461592253986,11.1375921938474,-16.5199028072177));
#39590=CARTESIAN_POINT('Ctrl Pts',(-2.26453145297425,11.235880624647,-16.4565023553868));
#39591=CARTESIAN_POINT('Ctrl Pts',(-1.64184500498462,11.3201177955775,-16.402113388426));
#39592=CARTESIAN_POINT('Ctrl Pts',(-0.960212638605293,11.381790604117,-16.3622452378034));
#39593=CARTESIAN_POINT('Ctrl Pts',(-0.241942357302399,11.4117378642006,
-16.3428500559305));
#39594=CARTESIAN_POINT('Ctrl Pts',(0.474833609088317,11.405613463525,-16.3468207371218));
#39595=CARTESIAN_POINT('Ctrl Pts',(1.15457138884398,11.3668033364056,-16.3719381825921));
#39596=CARTESIAN_POINT('Ctrl Pts',(1.77349849179209,11.3037244443956,-16.4127012242899));
#39597=CARTESIAN_POINT('Ctrl Pts',(2.32515189705749,11.2254457645873,-16.4632340183868));
#39598=CARTESIAN_POINT('Ctrl Pts',(2.81389080815452,11.1388643635119,-16.5190803431333));
#39599=CARTESIAN_POINT('Ctrl Pts',(3.25054254209914,11.0477876676189,-16.5777860337094));
#39600=CARTESIAN_POINT('Ctrl Pts',(3.64139929966152,10.9552493865708,-16.6373985951458));
#39601=CARTESIAN_POINT('Ctrl Pts',(3.99000282473668,10.8639241945068,-16.6961988316824));
#39602=CARTESIAN_POINT('Ctrl Pts',(4.29924871552588,10.7759851546574,-16.7527920773989));
#39603=CARTESIAN_POINT('Ctrl Pts',(4.57314637444018,10.692677781047,-16.8063815627452));
#39604=CARTESIAN_POINT('Ctrl Pts',(4.81668678414937,10.6143370339782,-16.85675657135));
#39605=CARTESIAN_POINT('Ctrl Pts',(5.03480081202369,10.5407725073575,-16.9040443288795));
#39606=CARTESIAN_POINT('Ctrl Pts',(5.23132417481802,10.4717385146491,-16.9484081620974));
#39607=CARTESIAN_POINT('Ctrl Pts',(5.40889929673994,10.4071198003723,-16.9899293333123));
#39608=CARTESIAN_POINT('Ctrl Pts',(5.56944961741275,10.3468714240165,-17.0286475895997));
#39609=CARTESIAN_POINT('Ctrl Pts',(5.70244435423125,10.295598206018,-17.0616190888325));
#39610=CARTESIAN_POINT('Ctrl Pts',(5.78208456369384,10.2642482618129,-17.0818074036475));
#39611=CARTESIAN_POINT('Ctrl Pts',(5.81359195404932,10.2517424965309,-17.0898698238178));
#39612=CARTESIAN_POINT('Ctrl Pts',(-5.84786850162611,10.2455091795785,-16.942757011536));
#39613=CARTESIAN_POINT('Ctrl Pts',(-5.81221746652095,10.2595705751324,-16.9336462242179));
#39614=CARTESIAN_POINT('Ctrl Pts',(-5.69514241486186,10.3053212667506,-16.9040207987418));
#39615=CARTESIAN_POINT('Ctrl Pts',(-5.48748642398773,10.3839895355852,-16.8531449384918));
#39616=CARTESIAN_POINT('Ctrl Pts',(-5.21539354735681,10.4823007198192,-16.7895316072133));
#39617=CARTESIAN_POINT('Ctrl Pts',(-4.91498002652965,10.5850367417634,-16.7229931586931));
#39618=CARTESIAN_POINT('Ctrl Pts',(-4.58311636433276,10.69146038893,-16.653997204036));
#39619=CARTESIAN_POINT('Ctrl Pts',(-4.21502391534534,10.800836602231,-16.5830176461027));
#39620=CARTESIAN_POINT('Ctrl Pts',(-3.80511608444942,10.9119176830569,-16.5108610123053));
#39621=CARTESIAN_POINT('Ctrl Pts',(-3.34839262726853,11.0223681180405,-16.4390398832391));
#39622=CARTESIAN_POINT('Ctrl Pts',(-2.84070950668018,11.128662768988,-16.3698410197423));
#39623=CARTESIAN_POINT('Ctrl Pts',(-2.27732756424709,11.2263498157947,-16.306158234012));
#39624=CARTESIAN_POINT('Ctrl Pts',(-1.65102971936692,11.3099812154025,-16.2515425131447));
#39625=CARTESIAN_POINT('Ctrl Pts',(-0.965518635472634,11.3711183727228,
-16.2115228624109));
#39626=CARTESIAN_POINT('Ctrl Pts',(-0.243255125004045,11.4007234847768,
-16.1920650191604));
#39627=CARTESIAN_POINT('Ctrl Pts',(0.477426609194236,11.394679759103,-16.1960472258656));
#39628=CARTESIAN_POINT('Ctrl Pts',(1.16097791888811,11.356270398663,-16.2212512619957));
#39629=CARTESIAN_POINT('Ctrl Pts',(1.78344318131467,11.2937116193071,-16.2621735172597));
#39630=CARTESIAN_POINT('Ctrl Pts',(2.33830463684603,11.2159798756401,-16.3129196770289));
#39631=CARTESIAN_POINT('Ctrl Pts',(2.82992234932633,11.1299242514357,-16.3690154106596));
#39632=CARTESIAN_POINT('Ctrl Pts',(3.26917171323198,11.0393373738254,-16.4279944912735));
#39633=CARTESIAN_POINT('Ctrl Pts',(3.66237112484065,10.9472446708381,-16.4878938370364));
#39634=CARTESIAN_POINT('Ctrl Pts',(4.01307568172585,10.8563152592409,-16.5469843393736));
#39635=CARTESIAN_POINT('Ctrl Pts',(4.32419287162572,10.7687191219718,-16.603862836127));
#39636=CARTESIAN_POINT('Ctrl Pts',(4.59975269123718,10.6857020288348,-16.6577271362962));
#39637=CARTESIAN_POINT('Ctrl Pts',(4.84477427515613,10.6076014135021,-16.7083643670323));
#39638=CARTESIAN_POINT('Ctrl Pts',(5.06421758701105,10.5342296300905,-16.7559017066983));
#39639=CARTESIAN_POINT('Ctrl Pts',(5.26194192432505,10.4653426280537,-16.8005029943812));
#39640=CARTESIAN_POINT('Ctrl Pts',(5.44060721984951,10.4008258962196,-16.8422499285557));
#39641=CARTESIAN_POINT('Ctrl Pts',(5.60215126518848,10.340635949735,-16.8811827769094));
#39642=CARTESIAN_POINT('Ctrl Pts',(5.73598090626615,10.2893801627774,-16.9143415437475));
#39643=CARTESIAN_POINT('Ctrl Pts',(5.81613029482418,10.2580271472924,-16.9346474073568));
#39644=CARTESIAN_POINT('Ctrl Pts',(5.84784091563367,10.2455195690895,-16.9427572183048));
#39645=CARTESIAN_POINT('',(-5.593361696257,10.114435612469,-17.2450590606623));
#39646=CARTESIAN_POINT('Ctrl Pts',(-5.593361696257,10.114435612469,-17.2450590606623));
#39647=CARTESIAN_POINT('Ctrl Pts',(-5.53988028306012,10.1354439865193,-17.23180878986));
#39648=CARTESIAN_POINT('Ctrl Pts',(-5.47937289761996,10.1588326290219,-17.2170754989487));
#39649=CARTESIAN_POINT('Ctrl Pts',(-5.378072861095,10.1973859622821,-17.1928371623116));
#39650=CARTESIAN_POINT('Ctrl Pts',(-5.34254968919255,10.2108081643024,-17.1844054697643));
#39651=CARTESIAN_POINT('Ctrl Pts',(-5.2866301917477,10.2317219773105,-17.1712769734231));
#39652=CARTESIAN_POINT('Ctrl Pts',(-5.25801175812749,10.2423733662331,-17.1645928615778));
#39653=CARTESIAN_POINT('Ctrl Pts',(-5.22840529716057,10.2532965141372,-17.1577411945075));
#39654=CARTESIAN_POINT('Ctrl Pts',(-5.20844809488337,10.2606364040394,-17.1531377696007));
#39655=CARTESIAN_POINT('Ctrl Pts',(-5.19640811531086,10.2650483759484,-17.1503710837434));
#39656=CARTESIAN_POINT('Ctrl Pts',(-5.12218902892848,10.2921680495835,-17.1333663951139));
#39657=CARTESIAN_POINT('Ctrl Pts',(-5.04952088095849,10.3182376312863,-17.1170332995621));
#39658=CARTESIAN_POINT('Ctrl Pts',(-4.93047521889172,10.3599563102957,-17.090921208127));
#39659=CARTESIAN_POINT('Ctrl Pts',(-4.86844152783038,10.3814640319628,-17.0774650732981));
#39660=CARTESIAN_POINT('Ctrl Pts',(-4.7916748832099,10.4075658113976,-17.0611442365309));
#39661=CARTESIAN_POINT('Ctrl Pts',(-4.75219305963743,10.4208496513771,-17.0528403485297));
#39662=CARTESIAN_POINT('Ctrl Pts',(-4.73503688497876,10.4265904842544,-17.0492521356902));
#39663=CARTESIAN_POINT('Ctrl Pts',(-4.72354712562239,10.4304280694972,-17.0468536144988));
#39664=CARTESIAN_POINT('Ctrl Pts',(-4.71663332011695,10.4327323041815,-17.0454135176634));
#39665=CARTESIAN_POINT('Ctrl Pts',(-4.56303751863232,10.4838416899302,-17.0134723230282));
#39666=CARTESIAN_POINT('Ctrl Pts',(-4.38712946317573,10.5399084731665,-16.9784638974453));
#39667=CARTESIAN_POINT('Ctrl Pts',(-4.08281737169274,10.6299894329539,-16.9222869539802));
#39668=CARTESIAN_POINT('Ctrl Pts',(-3.97463833981539,10.6609811182779,-16.9029696525196));
#39669=CARTESIAN_POINT('Ctrl Pts',(-3.80225728992482,10.7081749541802,-16.8735681800859));
#39670=CARTESIAN_POINT('Ctrl Pts',(-3.71353863946091,10.7319458246321,-16.8587626980378));
#39671=CARTESIAN_POINT('Ctrl Pts',(-3.60560932759541,10.7597947892436,-16.8414239018793));
#39672=CARTESIAN_POINT('Ctrl Pts',(-3.55053861674825,10.7737230309169,-16.8327539264673));
#39673=CARTESIAN_POINT('Ctrl Pts',(-3.52669987176067,10.7796903351693,-16.8290398219781));
#39674=CARTESIAN_POINT('Ctrl Pts',(-3.51075470582064,10.783667796514,-16.8265643021482));
#39675=CARTESIAN_POINT('Ctrl Pts',(-3.5015584239999,10.7859527405556,-16.825142240374));
#39676=CARTESIAN_POINT('Ctrl Pts',(-3.27623811862249,10.8417639726306,-16.7904085637452));
#39677=CARTESIAN_POINT('Ctrl Pts',(-3.02980309372394,10.8978171053894,-16.7555580309812));
#39678=CARTESIAN_POINT('Ctrl Pts',(-2.61823664503177,10.9783706192322,-16.7055410572012));
#39679=CARTESIAN_POINT('Ctrl Pts',(-2.47406217691032,11.0046130418625,-16.68925818084));
#39680=CARTESIAN_POINT('Ctrl Pts',(-2.24732199689207,11.0420890498694,-16.6660245528667));
#39681=CARTESIAN_POINT('Ctrl Pts',(-2.16999552391331,11.054265359023,-16.658479120914));
#39682=CARTESIAN_POINT('Ctrl Pts',(-2.01184975201042,11.0778120156048,-16.6438948098896));
#39683=CARTESIAN_POINT('Ctrl Pts',(-1.93305534133166,11.0889155988717,-16.6370209864462));
#39684=CARTESIAN_POINT('Ctrl Pts',(-1.51010234062083,11.1446314683416,-16.6025490483757));
#39685=CARTESIAN_POINT('Ctrl Pts',(-1.15547545530011,11.1793411116954,-16.5811403702837));
#39686=CARTESIAN_POINT('Ctrl Pts',(-0.599138400190915,11.2105411459179,
-16.5619612691803));
#39687=CARTESIAN_POINT('Ctrl Pts',(-0.409626593966499,11.2174664487711,
-16.5577208744858));
#39688=CARTESIAN_POINT('Ctrl Pts',(-0.119259702847854,11.2219241593423,
-16.5549970017463));
#39689=CARTESIAN_POINT('Ctrl Pts',(0.0274485381569757,11.2226707105659,
-16.5545430063037));
#39690=CARTESIAN_POINT('Ctrl Pts',(0.201276544692242,11.2207992343843,-16.555685031869));
#39691=CARTESIAN_POINT('Ctrl Pts',(0.276346060070852,11.2193954414903,-16.556543017445));
#39692=CARTESIAN_POINT('Ctrl Pts',(0.326519469943717,11.218324255164,-16.5571979302159));
#39693=CARTESIAN_POINT('Ctrl Pts',(0.353423748371615,11.2176742699932,-16.5575954345784));
#39694=CARTESIAN_POINT('Ctrl Pts',(0.752239173257733,11.2070497311517,-16.5640948719712));
#39695=CARTESIAN_POINT('Ctrl Pts',(1.10870726251511,11.1824492230569,-16.5792077214685));
#39696=CARTESIAN_POINT('Ctrl Pts',(1.61507798927156,11.1301017166863,-16.6115346913009));
#39697=CARTESIAN_POINT('Ctrl Pts',(1.86118050086738,11.1000689808603,-16.6301060277878));
#39698=CARTESIAN_POINT('Ctrl Pts',(2.13590510710996,11.0596864044952,-16.6551179812476));
#39699=CARTESIAN_POINT('Ctrl Pts',(2.25098815465266,11.0413827195364,-16.6664621426317));
#39700=CARTESIAN_POINT('Ctrl Pts',(2.32711994869927,11.0289750497037,-16.6741536414256));
#39701=CARTESIAN_POINT('Ctrl Pts',(2.36664743998163,11.0223685668864,-16.6782498198878));
#39702=CARTESIAN_POINT('Ctrl Pts',(2.68811795660455,10.9674606160988,-16.7123001593168));
#39703=CARTESIAN_POINT('Ctrl Pts',(2.94939629479706,10.9141967924827,-16.7453824107961));
#39704=CARTESIAN_POINT('Ctrl Pts',(3.30460395387738,10.8339032238938,-16.7953063331382));
#39705=CARTESIAN_POINT('Ctrl Pts',(3.41688819886941,10.8070585507245,-16.8120063272807));
#39706=CARTESIAN_POINT('Ctrl Pts',(3.57613710430534,10.7673178989158,-16.8367404354672));
#39707=CARTESIAN_POINT('Ctrl Pts',(3.65346719151028,10.7475775933703,-16.8490294893356));
#39708=CARTESIAN_POINT('Ctrl Pts',(3.73967048693491,10.7248990085834,-16.8631524446267));
#39709=CARTESIAN_POINT('Ctrl Pts',(3.77575436933522,10.7152671623837,-16.8691515896455));
#39710=CARTESIAN_POINT('Ctrl Pts',(3.79961909380934,10.7088667058967,-16.8731382911077));
#39711=CARTESIAN_POINT('Ctrl Pts',(3.80971292521982,10.7061487497407,-16.8748313201729));
#39712=CARTESIAN_POINT('Ctrl Pts',(4.03894258058649,10.6440870525456,-16.9134922223104));
#39713=CARTESIAN_POINT('Ctrl Pts',(4.23294189407636,10.5865357761191,-16.9493762692554));
#39714=CARTESIAN_POINT('Ctrl Pts',(4.49132149755771,10.5060702067502,-16.9995962783043));
#39715=CARTESIAN_POINT('Ctrl Pts',(4.57201147092592,10.4802061465832,-17.0157474374254));
#39716=CARTESIAN_POINT('Ctrl Pts',(4.68489158928988,10.4432294217741,-17.0388507172504));
#39717=CARTESIAN_POINT('Ctrl Pts',(4.73929293804978,10.4251937998733,-17.0501227569471));
#39718=CARTESIAN_POINT('Ctrl Pts',(4.79919343503098,10.4050054499792,-17.0627452020711));
#39719=CARTESIAN_POINT('Ctrl Pts',(4.82410056018608,10.3965411605049,-17.0680383274529));
#39720=CARTESIAN_POINT('Ctrl Pts',(4.8405354177543,10.390940564724,-17.0715408484918));
#39721=CARTESIAN_POINT('Ctrl Pts',(4.84701640186461,10.3887273506808,-17.0729250180429));
#39722=CARTESIAN_POINT('Ctrl Pts',(4.93430771376098,10.358813700624,-17.0916346102252));
#39723=CARTESIAN_POINT('Ctrl Pts',(5.00672900437769,10.3333491942336,-17.1075721097258));
#39724=CARTESIAN_POINT('Ctrl Pts',(5.10760446036601,10.297274985841,-17.1301685902159));
#39725=CARTESIAN_POINT('Ctrl Pts',(5.15610306837598,10.2797653186203,-17.1411413232466));
#39726=CARTESIAN_POINT('Ctrl Pts',(5.20929131774862,10.2603202481462,-17.1533350719783));
#39727=CARTESIAN_POINT('Ctrl Pts',(5.23135911177139,10.2522013363372,-17.1584280078407));
#39728=CARTESIAN_POINT('Ctrl Pts',(5.24590938112122,10.2468368234746,-17.1617934884257));
#39729=CARTESIAN_POINT('Ctrl Pts',(5.25204166646472,10.2445718761053,-17.1632145550785));
#39730=CARTESIAN_POINT('Ctrl Pts',(5.39102676460598,10.1931086596194,-17.1955073708392));
#39731=CARTESIAN_POINT('Ctrl Pts',(5.50207490988016,10.1502945569566,-17.2224423306575));
#39732=CARTESIAN_POINT('Ctrl Pts',(5.593361696298,10.1144356125401,-17.2450590604365));
#39733=CARTESIAN_POINT('',(-5.73644346265599,10.2877335026453,-16.9337808606183));
#39734=CARTESIAN_POINT('Origin',(-5.599999999997,9.91330329093349,-16.899368849389));
#39735=CARTESIAN_POINT('Ctrl Pts',(-5.73644387762288,10.2877346861591,-16.9337810352107));
#39736=CARTESIAN_POINT('Ctrl Pts',(-5.73644352459358,10.2877348228399,-16.9337809477608));
#39737=CARTESIAN_POINT('Ctrl Pts',(-5.73644317156403,10.2877349595207,-16.9337808603108));
#39738=CARTESIAN_POINT('Ctrl Pts',(-5.73644281853424,10.2877350962016,-16.9337807728608));
#39739=CARTESIAN_POINT('Ctrl Pts',(-5.67992307657405,10.3096175850451,-16.9197801051606));
#39740=CARTESIAN_POINT('Ctrl Pts',(-5.61717065511268,10.3335904563916,-16.9044747020212));
#39741=CARTESIAN_POINT('Ctrl Pts',(-5.54808297603754,10.3594537576529,-16.8879871425014));
#39742=CARTESIAN_POINT('Ctrl Pts',(-5.52952075197148,10.3664026145189,-16.883557325518));
#39743=CARTESIAN_POINT('Ctrl Pts',(-5.51050111168914,10.3734876798064,-16.8790422721391));
#39744=CARTESIAN_POINT('Ctrl Pts',(-5.49102186563804,10.3807044999465,-16.8744445705152));
#39745=CARTESIAN_POINT('Ctrl Pts',(-5.421960655898,10.4062908254154,-16.8581439993671));
#39746=CARTESIAN_POINT('Ctrl Pts',(-5.34712351064947,10.4335365033827,-16.8408025360917));
#39747=CARTESIAN_POINT('Ctrl Pts',(-5.26640088171051,10.4622164379704,-16.8225623695911));
#39748=CARTESIAN_POINT('Ctrl Pts',(-5.25085290357015,10.4677404775352,-16.8190491327979));
#39749=CARTESIAN_POINT('Ctrl Pts',(-5.2350865382652,10.4733175987422,-16.8155026320632));
#39750=CARTESIAN_POINT('Ctrl Pts',(-5.21910094042576,10.4789460078782,-16.8119239946774));
#39751=CARTESIAN_POINT('Ctrl Pts',(-5.19132695624702,10.4887250194524,-16.8057063343102));
#39752=CARTESIAN_POINT('Ctrl Pts',(-5.16289118481947,10.4986588865672,-16.7993916409934));
#39753=CARTESIAN_POINT('Ctrl Pts',(-5.1337891480606,10.5087377160842,-16.792986244664));
#39754=CARTESIAN_POINT('Ctrl Pts',(-5.06602703525961,10.5322055849584,-16.7780717150657));
#39755=CARTESIAN_POINT('Ctrl Pts',(-4.99465299111353,10.5564606256927,-16.7626646217621));
#39756=CARTESIAN_POINT('Ctrl Pts',(-4.91960734870379,10.5813652266411,-16.7468531387424));
#39757=CARTESIAN_POINT('Ctrl Pts',(-4.82891643643845,10.6114618572661,-16.7277453295043));
#39758=CARTESIAN_POINT('Ctrl Pts',(-4.73286349694366,10.6425084044306,-16.7080460567318));
#39759=CARTESIAN_POINT('Ctrl Pts',(-4.63133837398873,10.6742244178999,-16.6879363746291));
#39760=CARTESIAN_POINT('Ctrl Pts',(-4.61738997120669,10.6785818391729,-16.6851735319195));
#39761=CARTESIAN_POINT('Ctrl Pts',(-4.60333826776916,10.6829518303966,-16.6824029867582));
#39762=CARTESIAN_POINT('Ctrl Pts',(-4.58918296916372,10.6873335996056,-16.6796252516688));
#39763=CARTESIAN_POINT('Ctrl Pts',(-4.55700168044369,10.6972953096304,-16.6733102245267));
#39764=CARTESIAN_POINT('Ctrl Pts',(-4.52428495643809,10.7073179243454,-16.6669580163093));
#39765=CARTESIAN_POINT('Ctrl Pts',(-4.4910294131758,10.7173918284569,-16.6605748444745));
#39766=CARTESIAN_POINT('Ctrl Pts',(-4.45061997010429,10.7296328209282,-16.6528185309829));
#39767=CARTESIAN_POINT('Ctrl Pts',(-4.4094149533028,10.7419495710167,-16.6450164806071));
#39768=CARTESIAN_POINT('Ctrl Pts',(-4.36740824388631,10.7543239371829,-16.6371804442443));
#39769=CARTESIAN_POINT('Ctrl Pts',(-4.34640488917806,10.760511120266,-16.6332624260629));
#39770=CARTESIAN_POINT('Ctrl Pts',(-4.3252011074128,10.7667126935057,-16.6293359105165));
#39771=CARTESIAN_POINT('Ctrl Pts',(-4.30379613383866,10.7729262929956,-16.6254024423939));
#39772=CARTESIAN_POINT('Ctrl Pts',(-4.29309364705158,10.7760330927405,-16.6234357083326));
#39773=CARTESIAN_POINT('Ctrl Pts',(-4.28234086205917,10.7791428981615,-16.6214672360706));
#39774=CARTESIAN_POINT('Ctrl Pts',(-4.27153768256719,10.7822554080201,-16.6194972207862));
#39775=CARTESIAN_POINT('Ctrl Pts',(-4.2634352979482,10.784589790414,-16.6180197093228));
#39776=CARTESIAN_POINT('Ctrl Pts',(-4.25530456640277,10.7869256939804,-16.6165413299049));
#39777=CARTESIAN_POINT('Ctrl Pts',(-4.24714544723451,10.7892629901513,-16.6150621657675));
#39778=CARTESIAN_POINT('Ctrl Pts',(-4.24442574084509,10.790042088875,-16.6145691110551));
#39779=CARTESIAN_POINT('Ctrl Pts',(-4.24040612494836,10.7911921014736,-16.6138413435076));
#39780=CARTESIAN_POINT('Ctrl Pts',(-4.23897686402988,10.791600745692,-16.6135827432249));
#39781=CARTESIAN_POINT('Ctrl Pts',(-4.23363917081557,10.7931268613534,-16.612616979062));
#39782=CARTESIAN_POINT('Ctrl Pts',(-4.22827719948883,10.7946570374923,-16.6116486331607));
#39783=CARTESIAN_POINT('Ctrl Pts',(-4.22289092374133,10.7961912023985,-16.6106777518021));
#39784=CARTESIAN_POINT('Ctrl Pts',(-4.14210875622134,10.8192002669668,-16.5961166887915));
#39785=CARTESIAN_POINT('Ctrl Pts',(-4.05586011230241,10.8431100287053,-16.5809830331791));
#39786=CARTESIAN_POINT('Ctrl Pts',(-3.96405508318161,10.867656673159,-16.5654470829088));
#39787=CARTESIAN_POINT('Ctrl Pts',(-3.91582472241796,10.8805524102322,-16.5572851718075));
#39788=CARTESIAN_POINT('Ctrl Pts',(-3.86606072113723,10.8936232288064,-16.5490126840931));
#39789=CARTESIAN_POINT('Ctrl Pts',(-3.81474963041862,10.9068260275257,-16.5406574901261));
#39790=CARTESIAN_POINT('Ctrl Pts',(-3.71991775466438,10.93122711022,-16.5252156294078));
#39791=CARTESIAN_POINT('Ctrl Pts',(-3.61980126908533,10.9560815366103,-16.5094896077981));
#39792=CARTESIAN_POINT('Ctrl Pts',(-3.51431774214659,10.9810861271972,-16.4936755668265));
#39793=CARTESIAN_POINT('Ctrl Pts',(-3.46379272468944,10.9930629487216,-16.486100879865));
#39794=CARTESIAN_POINT('Ctrl Pts',(-3.412036380583,11.0050735980661,-16.4785064074652));
#39795=CARTESIAN_POINT('Ctrl Pts',(-3.35903983414187,11.0170811856145,-16.4709160458442));
#39796=CARTESIAN_POINT('Ctrl Pts',(-3.24836795982101,11.0421564463494,-16.4550652101997));
#39797=CARTESIAN_POINT('Ctrl Pts',(-3.13228704122553,11.0672213831024,-16.4392303151227));
#39798=CARTESIAN_POINT('Ctrl Pts',(-3.01072545229427,11.0919081379047,-16.4236498311181));
#39799=CARTESIAN_POINT('Ctrl Pts',(-2.96856990008022,11.1004690969233,-16.4182467764793));
#39800=CARTESIAN_POINT('Ctrl Pts',(-2.92501756168561,11.1091302428328,-16.4127824107507));
#39801=CARTESIAN_POINT('Ctrl Pts',(-2.88136956717368,11.1176134042915,-16.4074326091601));
#39802=CARTESIAN_POINT('Ctrl Pts',(-2.87180831191927,11.1194716723054,-16.4062607152589));
#39803=CARTESIAN_POINT('Ctrl Pts',(-2.8622425152675,11.1213215615031,-16.4050942142145));
#39804=CARTESIAN_POINT('Ctrl Pts',(-2.85268593487647,11.1231604237239,-16.4039347765108));
#39805=CARTESIAN_POINT('Ctrl Pts',(-2.83186336209958,11.1271670705424,-16.4014085092711));
#39806=CARTESIAN_POINT('Ctrl Pts',(-2.81108450308508,11.1311212182118,-16.3989158713156));
#39807=CARTESIAN_POINT('Ctrl Pts',(-2.79049215901235,11.134997151391,-16.3964730579524));
#39808=CARTESIAN_POINT('Ctrl Pts',(-2.6196898288082,11.1671459158238,-16.3762112454449));
#39809=CARTESIAN_POINT('Ctrl Pts',(-2.4535496126387,11.1954664439551,-16.3583811544424));
#39810=CARTESIAN_POINT('Ctrl Pts',(-2.29231363557507,11.2203978130869,-16.3427011640703));
#39811=CARTESIAN_POINT('Ctrl Pts',(-2.12996501605265,11.2455012263267,-16.3269129706572));
#39812=CARTESIAN_POINT('Ctrl Pts',(-1.97258856158854,11.2671693869041,-16.3133041243216));
#39813=CARTESIAN_POINT('Ctrl Pts',(-1.82039230653809,11.2858594066231,-16.3015811008586));
#39814=CARTESIAN_POINT('Ctrl Pts',(-1.76982075559219,11.2920696992751,-16.2976857916205));
#39815=CARTESIAN_POINT('Ctrl Pts',(-1.71982072511009,11.297951085905,-16.2939987443829));
#39816=CARTESIAN_POINT('Ctrl Pts',(-1.67039864250388,11.303520032287,-16.2905093604163));
#39817=CARTESIAN_POINT('Ctrl Pts',(-1.52115750354897,11.3203367234704,-16.2799723775543));
#39818=CARTESIAN_POINT('Ctrl Pts',(-1.37719003095167,11.3343061285816,-16.2712367654417));
#39819=CARTESIAN_POINT('Ctrl Pts',(-1.23865184096789,11.3458828933172,-16.2640095546856));
#39820=CARTESIAN_POINT('Ctrl Pts',(-1.14900010082279,11.3533745250753,-16.2593326347637));
#39821=CARTESIAN_POINT('Ctrl Pts',(-1.06162099566594,11.3598637351623,-16.2552876599136));
#39822=CARTESIAN_POINT('Ctrl Pts',(-0.976547038833515,11.3654683087099,
-16.251798534706));
#39823=CARTESIAN_POINT('Ctrl Pts',(-0.844653982939271,11.3741572701701,
-16.2463892249342));
#39824=CARTESIAN_POINT('Ctrl Pts',(-0.718303156836323,11.3807218990101,
-16.2423147910948));
#39825=CARTESIAN_POINT('Ctrl Pts',(-0.597588683233163,11.3855885728515,
-16.2393007710482));
#39826=CARTESIAN_POINT('Ctrl Pts',(-0.480912740331577,11.3902924309913,
-16.2363875857412));
#39827=CARTESIAN_POINT('Ctrl Pts',(-0.369501725349506,11.3934099347066,
-16.234465086433));
#39828=CARTESIAN_POINT('Ctrl Pts',(-0.263411423276765,11.3952953898795,
-16.2333039999994));
#39829=CARTESIAN_POINT('Ctrl Pts',(-0.255777298906237,11.3954310648564,
-16.2332204496837));
#39830=CARTESIAN_POINT('Ctrl Pts',(-0.248170714764654,11.3955603470126,
-16.2331408500901));
#39831=CARTESIAN_POINT('Ctrl Pts',(-0.240591686757623,11.3956833622014,
-16.2330651195921));
#39832=CARTESIAN_POINT('Ctrl Pts',(-0.202104723971215,11.396308044019,-16.2326805535428));
#39833=CARTESIAN_POINT('Ctrl Pts',(-0.164328380149182,11.3967711706233,
-16.2323957255254));
#39834=CARTESIAN_POINT('Ctrl Pts',(-0.127264465149227,11.3970891950709,
-16.2321998280071));
#39835=CARTESIAN_POINT('Ctrl Pts',(-0.105083110171538,11.397279520706,-16.2320825907322));
#39836=CARTESIAN_POINT('Ctrl Pts',(-0.083156921819576,11.3974178649977,
-16.2319972023203));
#39837=CARTESIAN_POINT('Ctrl Pts',(-0.0614862081553471,11.3975076461867,
-16.2319414342152));
#39838=CARTESIAN_POINT('Ctrl Pts',(-0.0416887212949267,11.397589666647,
-16.2318904867317));
#39839=CARTESIAN_POINT('Ctrl Pts',(-0.023099625113114,11.3976306229785,
-16.2318646674111));
#39840=CARTESIAN_POINT('Ctrl Pts',(-0.00299170375185956,11.397634612254,
-16.231861115546));
#39841=CARTESIAN_POINT('Ctrl Pts',(-0.00108910381438552,11.3976349897169,
-16.2318607794706));
#39842=CARTESIAN_POINT('Ctrl Pts',(0.000827093947327497,11.3976350040678,
-16.2318606637935));
#39843=CARTESIAN_POINT('Ctrl Pts',(0.00275919977259721,11.3976346381463,
-16.2318607795923));
#39844=CARTESIAN_POINT('Ctrl Pts',(0.115376740968219,11.3976133095128,-16.2318675292087));
#39845=CARTESIAN_POINT('Ctrl Pts',(0.233548307689586,11.3963110824309,-16.2326602020464));
#39846=CARTESIAN_POINT('Ctrl Pts',(0.357219777273745,11.3933314488223,-16.2344971561809));
#39847=CARTESIAN_POINT('Ctrl Pts',(0.400696756010732,11.3922839520352,-16.2351429414709));
#39848=CARTESIAN_POINT('Ctrl Pts',(0.444853207289354,11.3910288181089,-16.2359179991661));
#39849=CARTESIAN_POINT('Ctrl Pts',(0.489685896103932,11.3895477543126,-16.2368342378403));
#39850=CARTESIAN_POINT('Ctrl Pts',(0.61695135346722,11.3853434947332,-16.2394351421582));
#39851=CARTESIAN_POINT('Ctrl Pts',(0.749668736397475,11.3793207257544,-16.2431724844734));
#39852=CARTESIAN_POINT('Ctrl Pts',(0.887739088610556,11.3710519035528,-16.2483218252168));
#39853=CARTESIAN_POINT('Ctrl Pts',(0.982252494670568,11.3653916402317,-16.2518467074586));
#39854=CARTESIAN_POINT('Ctrl Pts',(1.07927350380205,11.3586782993934,-16.256033599861));
#39855=CARTESIAN_POINT('Ctrl Pts',(1.17875932780541,11.3507671091198,-16.260975385379));
#39856=CARTESIAN_POINT('Ctrl Pts',(1.32354861553918,11.3392533520966,-16.2681675417737));
#39857=CARTESIAN_POINT('Ctrl Pts',(1.47356075193309,11.3252028802458,-16.2769583548483));
#39858=CARTESIAN_POINT('Ctrl Pts',(1.62863385522641,11.3081658687316,-16.2876375935685));
#39859=CARTESIAN_POINT('Ctrl Pts',(1.68658092645764,11.3017995492422,-16.2916281670055));
#39860=CARTESIAN_POINT('Ctrl Pts',(1.74523421223448,11.2950160271918,-16.2958825353738));
#39861=CARTESIAN_POINT('Ctrl Pts',(1.80458351108733,11.2877912174214,-16.3004161770378));
#39862=CARTESIAN_POINT('Ctrl Pts',(1.96231932538665,11.268589453048,-16.3124654796149));
#39863=CARTESIAN_POINT('Ctrl Pts',(2.12497514213533,11.2462709846675,-16.3264872932238));
#39864=CARTESIAN_POINT('Ctrl Pts',(2.29233589177227,11.2203922801793,-16.3427662443591));
#39865=CARTESIAN_POINT('Ctrl Pts',(2.31271087216276,11.2172417320513,-16.3447480908247));
#39866=CARTESIAN_POINT('Ctrl Pts',(2.33315552275998,11.2140384090245,-16.3467633944773));
#39867=CARTESIAN_POINT('Ctrl Pts',(2.35366940187776,11.2107815052252,-16.3488126712752));
#39868=CARTESIAN_POINT('Ctrl Pts',(2.36244348092684,11.2093884809598,-16.3496891762265));
#39869=CARTESIAN_POINT('Ctrl Pts',(2.37123022445249,11.2079856546398,-16.3505718962139));
#39870=CARTESIAN_POINT('Ctrl Pts',(2.38002959914226,11.2065729651554,-16.3514608704435));
#39871=CARTESIAN_POINT('Ctrl Pts',(2.44796695689478,11.1956660093453,-16.3583243763625));
#39872=CARTESIAN_POINT('Ctrl Pts',(2.51665736075251,11.1841711117674,-16.365560699008));
#39873=CARTESIAN_POINT('Ctrl Pts',(2.58608470263645,11.172060185812,-16.3731878432196));
#39874=CARTESIAN_POINT('Ctrl Pts',(2.62079837357841,11.1660047228343,-16.3770014153254));
#39875=CARTESIAN_POINT('Ctrl Pts',(2.65569627858871,11.1597952502236,-16.3809126927319));
#39876=CARTESIAN_POINT('Ctrl Pts',(2.69077624810768,11.1534282705164,-16.3849239162302));
#39877=CARTESIAN_POINT('Ctrl Pts',(2.70831623286716,11.1502447806628,-16.3869295279793));
#39878=CARTESIAN_POINT('Ctrl Pts',(2.72590173373479,11.1470219139176,-16.3889601262475));
#39879=CARTESIAN_POINT('Ctrl Pts',(2.7435324742445,11.1437592333271,-16.3910159905811));
#39880=CARTESIAN_POINT('Ctrl Pts',(2.75885712424319,11.1409233094429,-16.3928029490664));
#39881=CARTESIAN_POINT('Ctrl Pts',(2.77563471566203,11.1377908818067,-16.3947768843287));
#39882=CARTESIAN_POINT('Ctrl Pts',(2.79016543957015,11.1350561816445,-16.3965003301687));
#39883=CARTESIAN_POINT('Ctrl Pts',(2.79235205815691,11.1346446573295,-16.39675967848));
#39884=CARTESIAN_POINT('Ctrl Pts',(2.79448781861613,11.1342422193846,-16.3970133028468));
#39885=CARTESIAN_POINT('Ctrl Pts',(2.79656013539408,11.1338513131024,-16.3972596610821));
#39886=CARTESIAN_POINT('Ctrl Pts',(2.81155090954738,11.1310235659868,-16.3990417731148));
#39887=CARTESIAN_POINT('Ctrl Pts',(2.82653561969514,11.1281742204883,-16.4008378183665));
#39888=CARTESIAN_POINT('Ctrl Pts',(2.84151418411467,11.1253033432094,-16.402647751769));
#39889=CARTESIAN_POINT('Ctrl Pts',(2.98776286620042,11.0972724847966,-16.4203196973143));
#39890=CARTESIAN_POINT('Ctrl Pts',(3.13342565900406,11.067188944468,-16.4393156419953));
#39891=CARTESIAN_POINT('Ctrl Pts',(3.27843552237667,11.0351214013139,-16.4595893383465));
#39892=CARTESIAN_POINT('Ctrl Pts',(3.40982472733808,11.0060659363815,-16.4779587429046));
#39893=CARTESIAN_POINT('Ctrl Pts',(3.5406779002364,10.9753816751959,-16.4973771362034));
#39894=CARTESIAN_POINT('Ctrl Pts',(3.67095144391563,10.943123139663,-16.5178077455709));
#39895=CARTESIAN_POINT('Ctrl Pts',(3.78812567273624,10.9141082766509,-16.5361840085432));
#39896=CARTESIAN_POINT('Ctrl Pts',(3.90483097783149,10.8838198162215,-16.5553791605345));
#39897=CARTESIAN_POINT('Ctrl Pts',(4.02103992397148,10.8522990627777,-16.5753651336091));
#39898=CARTESIAN_POINT('Ctrl Pts',(4.12468261995777,10.8241868048582,-16.5931899242141));
#39899=CARTESIAN_POINT('Ctrl Pts',(4.22793050029308,10.7950943527066,-16.6116437523539));
#39900=CARTESIAN_POINT('Ctrl Pts',(4.33076689523681,10.7650516875563,-16.6307059990957));
#39901=CARTESIAN_POINT('Ctrl Pts',(4.42239699687154,10.7382828333719,-16.6476909936328));
#39902=CARTESIAN_POINT('Ctrl Pts',(4.51370040736879,10.7107595762264,-16.6651590304519));
#39903=CARTESIAN_POINT('Ctrl Pts',(4.60466714131258,10.6825033517688,-16.6830951531163));
#39904=CARTESIAN_POINT('Ctrl Pts',(4.68608821708453,10.6572122140875,-16.6991491361406));
#39905=CARTESIAN_POINT('Ctrl Pts',(4.76723956751118,10.6313338673615,-16.7155781214801));
#39906=CARTESIAN_POINT('Ctrl Pts',(4.84811525533268,10.6048836944837,-16.7323712567022));
#39907=CARTESIAN_POINT('Ctrl Pts',(4.92103851396308,10.5810343418595,-16.7475131389664));
#39908=CARTESIAN_POINT('Ctrl Pts',(4.99373765565988,10.5567200890228,-16.7629510788517));
#39909=CARTESIAN_POINT('Ctrl Pts',(5.06620920273585,10.5319521148902,-16.7786772584776));
#39910=CARTESIAN_POINT('Ctrl Pts',(5.13210920773643,10.5094300398822,-16.7929774267202));
#39911=CARTESIAN_POINT('Ctrl Pts',(5.19782102170716,10.4865327979589,-16.8075159308807));
#39912=CARTESIAN_POINT('Ctrl Pts',(5.26334266567217,10.4632686283996,-16.8222874368434));
#39913=CARTESIAN_POINT('Ctrl Pts',(5.32292443051119,10.4421134772773,-16.8357198286658));
#39914=CARTESIAN_POINT('Ctrl Pts',(5.38234894166926,10.4206549108743,-16.8493448913841));
#39915=CARTESIAN_POINT('Ctrl Pts',(5.44161508240666,10.3988989162237,-16.8631598859357));
#39916=CARTESIAN_POINT('Ctrl Pts',(5.49538235744157,10.3791614989821,-16.87569308959));
#39917=CARTESIAN_POINT('Ctrl Pts',(5.54901928600415,10.359179284877,-16.8883826152172));
#39918=CARTESIAN_POINT('Ctrl Pts',(5.60252500722285,10.3389565104295,-16.9012289578158));
#39919=CARTESIAN_POINT('Ctrl Pts',(5.6472564469046,10.3220500227719,-16.9119686579076));
#39920=CARTESIAN_POINT('Ctrl Pts',(5.69189618355805,10.3049754018566,-16.9228179599782));
#39921=CARTESIAN_POINT('Ctrl Pts',(5.73644276371256,10.2877350949212,-16.9337809951185));
#39922=CARTESIAN_POINT('Ctrl Pts',(-5.843530256063,10.2251612018568,-17.1593147457631));
#39923=CARTESIAN_POINT('Ctrl Pts',(-3.895686837375,11.0033631167315,-16.6619433466125));
#39924=CARTESIAN_POINT('Ctrl Pts',(0.0001633689297129,11.7816837051417,
-16.1645459237592));
#39925=CARTESIAN_POINT('Ctrl Pts',(3.896013575235,11.0032978376656,-16.6619850641797));
#39926=CARTESIAN_POINT('Ctrl Pts',(5.844020362852,10.2249653863089,-17.1594398971657));
#39927=CARTESIAN_POINT('Ctrl Pts',(-5.843530256063,10.3258757938396,-16.2770692610481));
#39928=CARTESIAN_POINT('Ctrl Pts',(-3.895686837375,11.0553896787781,-15.8346873902757));
#39929=CARTESIAN_POINT('Ctrl Pts',(0.0001633689297129,11.7876693634894,
-15.3921230864179));
#39930=CARTESIAN_POINT('Ctrl Pts',(3.896013575235,11.0553282612408,-15.8347245088966));
#39931=CARTESIAN_POINT('Ctrl Pts',(5.844020362852,10.3256922294701,-16.2771805756635));
#39932=CARTESIAN_POINT('Ctrl Pts',(-5.843530256063,10.2973084286348,-14.4766645869159));
#39933=CARTESIAN_POINT('Ctrl Pts',(-3.895686837375,10.9728038432035,-14.1582375728196));
#39934=CARTESIAN_POINT('Ctrl Pts',(0.0001633689297129,11.6469744444563,
-13.8399446100658));
#39935=CARTESIAN_POINT('Ctrl Pts',(3.896013575235,10.9727472993719,-14.1582642685905));
#39936=CARTESIAN_POINT('Ctrl Pts',(5.844020362852,10.2971384566574,-14.4767447113191));
#39937=CARTESIAN_POINT('Ctrl Pts',(-5.843530256063,9.5578304148104,-11.8732201296631));
#39938=CARTESIAN_POINT('Ctrl Pts',(-3.895686837375,10.2763900787824,-11.7328262507199));
#39939=CARTESIAN_POINT('Ctrl Pts',(0.0001633689297128,10.9955719605871,
-11.5921562078845));
#39940=CARTESIAN_POINT('Ctrl Pts',(3.896013575235,10.276329759774,-11.7328380489468));
#39941=CARTESIAN_POINT('Ctrl Pts',(5.844020362852,9.55764960678671,-11.8732554563657));
#39942=CARTESIAN_POINT('Ctrl Pts',(-5.843530256063,8.22106676100552,-9.63752328128312));
#39943=CARTESIAN_POINT('Ctrl Pts',(-3.895686837375,9.09189067503903,-9.61305770160358));
#39944=CARTESIAN_POINT('Ctrl Pts',(0.0001633689297132,9.96180813993581,
-9.58947419762877));
#39945=CARTESIAN_POINT('Ctrl Pts',(3.896013575235,9.09181771358517,-9.61305967959051));
#39946=CARTESIAN_POINT('Ctrl Pts',(5.844020362852,8.22084763937311,-9.63752943746074));
#39947=CARTESIAN_POINT('Ctrl Pts',(-5.843530256063,7.02207811294743,-8.43809751774869));
#39948=CARTESIAN_POINT('Ctrl Pts',(-3.895686837375,8.04135302927588,-8.43217964834793));
#39949=CARTESIAN_POINT('Ctrl Pts',(0.0001633689297125,9.06228035038236,
-8.42461129239938));
#39950=CARTESIAN_POINT('Ctrl Pts',(3.896013575235,8.04126740236864,-8.43218028311409));
#39951=CARTESIAN_POINT('Ctrl Pts',(5.844020362852,7.0218216372639,-8.4380990068179));
#39952=CARTESIAN_POINT('Ctrl Pts',(-5.843530256063,6.40544655073385,-7.9486149548088));
#39953=CARTESIAN_POINT('Ctrl Pts',(-3.895686837375,7.5011200872024,-7.93456153010133));
#39954=CARTESIAN_POINT('Ctrl Pts',(0.0001633689297125,8.59741267407606,
-7.91992172805397));
#39955=CARTESIAN_POINT('Ctrl Pts',(3.896013575235,7.50102813928303,-7.93456275796333));
#39956=CARTESIAN_POINT('Ctrl Pts',(5.844020362852,6.40517085118626,-7.94861849100275));
#39957=CARTESIAN_POINT('',(-5.73278772553971,6.65588342589818,-8.10254678308617));
#39958=CARTESIAN_POINT('Ctrl Pts',(-5.73644356954166,10.2877321244828,-16.9337807348495));
#39959=CARTESIAN_POINT('Ctrl Pts',(-5.73766037024604,10.3633357381801,-16.1063574319785));
#39960=CARTESIAN_POINT('Ctrl Pts',(-5.73849618482932,10.3386824461305,-15.2703428362758));
#39961=CARTESIAN_POINT('Ctrl Pts',(-5.73940756701684,10.0903333007246,-13.6301040101181));
#39962=CARTESIAN_POINT('Ctrl Pts',(-5.73948313455368,9.86673834048807,-12.8258709788125));
#39963=CARTESIAN_POINT('Ctrl Pts',(-5.7388740224731,9.23545640664265,-11.2957057307492));
#39964=CARTESIAN_POINT('Ctrl Pts',(-5.73818934285567,8.82745509879148,-10.5699144590352));
#39965=CARTESIAN_POINT('Ctrl Pts',(-5.73605973646658,7.85267849992233,-9.23785246261833));
#39966=CARTESIAN_POINT('Ctrl Pts',(-5.7346148096949,7.28539108565082,-8.63201128890514));
#39967=CARTESIAN_POINT('Ctrl Pts',(-5.73278797082,6.65588387270908,-8.10254625058942));
#39968=CARTESIAN_POINT('Ctrl Pts',(5.73278688057609,6.65588777859083,-8.10254157115373));
#39969=CARTESIAN_POINT('Ctrl Pts',(5.37901145696501,6.85200131459071,-8.10465302967502));
#39970=CARTESIAN_POINT('Ctrl Pts',(5.01621448638398,7.03118682771357,-8.10373337999374));
#39971=CARTESIAN_POINT('Ctrl Pts',(4.64600910147529,7.19213776342579,-8.10100488069798));
#39972=CARTESIAN_POINT('Ctrl Pts',(4.37165673834806,7.31141552479892,-8.09898284033849));
#39973=CARTESIAN_POINT('Ctrl Pts',(4.09323566077892,7.42067530523888,-8.09596915441615));
#39974=CARTESIAN_POINT('Ctrl Pts',(3.81140241906258,7.51940929188303,-8.09247479094618));
#39975=CARTESIAN_POINT('Ctrl Pts',(3.57236173411404,7.60315186125273,-8.08951099919389));
#39976=CARTESIAN_POINT('Ctrl Pts',(3.33086640167441,7.67932161809156,-8.08620166972316));
#39977=CARTESIAN_POINT('Ctrl Pts',(3.08731701794449,7.74764923593218,-8.08286091596895));
#39978=CARTESIAN_POINT('Ctrl Pts',(3.04371732347713,7.7598811012562,-8.08226286131267));
#39979=CARTESIAN_POINT('Ctrl Pts',(3.00005180200329,7.7718617807475,-8.08166380201583));
#39980=CARTESIAN_POINT('Ctrl Pts',(2.95632275176659,7.78358991883312,-8.08106554250556));
#39981=CARTESIAN_POINT('Ctrl Pts',(2.75787639428296,7.83681326282433,-8.07835058711549));
#39982=CARTESIAN_POINT('Ctrl Pts',(2.55811712333055,7.88487916025936,-8.07569724649496));
#39983=CARTESIAN_POINT('Ctrl Pts',(2.35731173231339,7.92759052582829,-8.0731958413278));
#39984=CARTESIAN_POINT('Ctrl Pts',(2.16334914198626,7.96884642568334,-8.07077967598871));
#39985=CARTESIAN_POINT('Ctrl Pts',(1.96841051361373,8.00510644711771,-8.06850527824001));
#39986=CARTESIAN_POINT('Ctrl Pts',(1.77273628508688,8.03624111800075,-8.06645356836242));
#39987=CARTESIAN_POINT('Ctrl Pts',(1.58015286697596,8.06688399512134,-8.06443426666811));
#39988=CARTESIAN_POINT('Ctrl Pts',(1.38685690380679,8.09256199738575,-8.06263068304187));
#39989=CARTESIAN_POINT('Ctrl Pts',(1.19307761884276,8.11320098306076,-8.06111934189182));
#39990=CARTESIAN_POINT('Ctrl Pts',(0.994919648475874,8.13430633244087,-8.05957385009748));
#39991=CARTESIAN_POINT('Ctrl Pts',(0.796256267013193,8.15014186612969,-8.05833397011766));
#39992=CARTESIAN_POINT('Ctrl Pts',(0.597332590239811,8.16068573962992,-8.05748069792611));
#39993=CARTESIAN_POINT('Ctrl Pts',(0.40855170583876,8.1706919982949,-8.05667093268564));
#39994=CARTESIAN_POINT('Ctrl Pts',(0.219536393470747,8.17593270670312,-8.05620935321766));
#39995=CARTESIAN_POINT('Ctrl Pts',(0.0304961540370044,8.17644103763726,
-8.05616438298739));
#39996=CARTESIAN_POINT('Ctrl Pts',(0.0203394270745499,8.17646834916902,
-8.05616196683329));
#39997=CARTESIAN_POINT('Ctrl Pts',(0.0101826281555681,8.17648201238107,
-8.05616075310184));
#39998=CARTESIAN_POINT('Ctrl Pts',(2.57897726576351E-5,8.17648203672123,
-8.05616075233821));
#39999=CARTESIAN_POINT('Ctrl Pts',(1.71931816709343E-5,8.17648203674183,
-8.05616075233757));
#40000=CARTESIAN_POINT('Ctrl Pts',(8.59659071081628E-6,8.17648203675266,
-8.05616075233779));
#40001=CARTESIAN_POINT('Ctrl Pts',(-2.20960885290795E-13,8.17648203675372,
-8.05616075233888));
#40002=CARTESIAN_POINT('Ctrl Pts',(-0.189394108313583,8.17648206011399,
-8.05616077638705));
#40003=CARTESIAN_POINT('Ctrl Pts',(-0.378774674464551,8.17173533196982,
-8.05658262828894));
#40004=CARTESIAN_POINT('Ctrl Pts',(-0.567931019578452,8.1622056991069,-8.05735754707092));
#40005=CARTESIAN_POINT('Ctrl Pts',(-0.769333664674303,8.15205910178166,
-8.05818263539842));
#40006=CARTESIAN_POINT('Ctrl Pts',(-0.970482116019627,8.13648985922757,
-8.05940799112298));
#40007=CARTESIAN_POINT('Ctrl Pts',(-1.17112206928258,8.11551790495007,-8.06094962786347));
#40008=CARTESIAN_POINT('Ctrl Pts',(-1.36692420168941,8.09505162542053,-8.06245409273338));
#40009=CARTESIAN_POINT('Ctrl Pts',(-1.56224206214246,8.0694405548821,-8.0642597569665));
#40010=CARTESIAN_POINT('Ctrl Pts',(-1.75683930164901,8.03875939082742,-8.06628774535347));
#40011=CARTESIAN_POINT('Ctrl Pts',(-1.95864861723658,8.00694113515736,-8.06839089414134));
#40012=CARTESIAN_POINT('Ctrl Pts',(-2.15968290739831,7.96967000868949,-8.07073314300512));
#40013=CARTESIAN_POINT('Ctrl Pts',(-2.35967855880933,7.92708729785437,-8.07322578424444));
#40014=CARTESIAN_POINT('Ctrl Pts',(-2.55967421022036,7.88450458701924,-8.07571842548375));
#40015=CARTESIAN_POINT('Ctrl Pts',(-2.75863122288067,7.83661067021283,-8.07836144421808));
#40016=CARTESIAN_POINT('Ctrl Pts',(-2.95628598346539,7.78360035556706,-8.08106560032508));
#40017=CARTESIAN_POINT('Ctrl Pts',(-3.19878486586875,7.71856300448368,-8.0843832782391));
#40018=CARTESIAN_POINT('Ctrl Pts',(-3.43933039900217,7.64575489262882,-8.0877255164212));
#40019=CARTESIAN_POINT('Ctrl Pts',(-3.6775306242641,7.56543015431638,-8.09078481904143));
#40020=CARTESIAN_POINT('Ctrl Pts',(-3.96235759097273,7.46938216972677,-8.09444296791431));
#40021=CARTESIAN_POINT('Ctrl Pts',(-4.24383121655615,7.36258759907886,-8.09769624835467));
#40022=CARTESIAN_POINT('Ctrl Pts',(-4.52128137417785,7.24555633741688,-8.10002218723693));
#40023=CARTESIAN_POINT('Ctrl Pts',(-4.88829810139467,7.09074499758769,-8.1030989866289));
#40024=CARTESIAN_POINT('Ctrl Pts',(-5.24827434791527,6.91802662505855,-8.10455035959127));
#40025=CARTESIAN_POINT('Ctrl Pts',(-5.59965894280897,6.72865801645831,-8.10319481985575));
#40026=CARTESIAN_POINT('Ctrl Pts',(-5.64417482545532,6.70466746342937,-8.10302309050658));
#40027=CARTESIAN_POINT('Ctrl Pts',(-5.68855281542513,6.68040966675613,-8.10280638090245));
#40028=CARTESIAN_POINT('Ctrl Pts',(-5.7327897587563,6.65588714131628,-8.10254235865644));
#40029=CARTESIAN_POINT('Ctrl Pts',(5.8442109276592,6.60975781659273,-8.11489313945908));
#40030=CARTESIAN_POINT('Ctrl Pts',(5.39516759795808,6.86923202515899,-8.12241643595089));
#40031=CARTESIAN_POINT('Ctrl Pts',(4.36936999562943,7.380526520853,-8.12655400963949));
#40032=CARTESIAN_POINT('Ctrl Pts',(2.70735887873967,7.93435136477757,-8.10987588460702));
#40033=CARTESIAN_POINT('Ctrl Pts',(0.904594091570436,8.22878805472967,-8.09288686312857));
#40034=CARTESIAN_POINT('Ctrl Pts',(-0.901198823780471,8.22906308886219,
-8.09286831827879));
#40035=CARTESIAN_POINT('Ctrl Pts',(-2.70398663593974,7.93518345288968,-8.1098357600967));
#40036=CARTESIAN_POINT('Ctrl Pts',(-4.36726502917644,7.38148399620803,-8.12654684250591));
#40037=CARTESIAN_POINT('Ctrl Pts',(-5.39421917802381,6.8697862795005,-8.12243344312352));
#40038=CARTESIAN_POINT('Ctrl Pts',(-5.84432678346674,6.60969083810708,-8.11489124898177));
#40039=CARTESIAN_POINT('Ctrl Pts',(5.72537981142124,6.40696257187108,-7.90741414418503));
#40040=CARTESIAN_POINT('Ctrl Pts',(5.28537605413658,6.66000489116012,-7.91604649446402));
#40041=CARTESIAN_POINT('Ctrl Pts',(4.28025648075084,7.15876699709817,-7.92256998014448));
#40042=CARTESIAN_POINT('Ctrl Pts',(2.6519626539299,7.69915973752875,-7.90889401748803));
#40043=CARTESIAN_POINT('Ctrl Pts',(0.886045026031056,7.98647110079696,-7.89367199191233));
#40044=CARTESIAN_POINT('Ctrl Pts',(-0.882719338489682,7.98673947796939,
-7.89365515637576));
#40045=CARTESIAN_POINT('Ctrl Pts',(-2.64865910398843,7.69997168607342,-7.90885871599316));
#40046=CARTESIAN_POINT('Ctrl Pts',(-4.27819398429727,7.15970115468978,-7.92256756530623));
#40047=CARTESIAN_POINT('Ctrl Pts',(-5.28444672405522,6.66054540297074,-7.9160658522132));
#40048=CARTESIAN_POINT('Ctrl Pts',(-5.72549333439,6.4068972576017,-7.90741196554548));
#40049=CARTESIAN_POINT('Ctrl Pts',(5.71943373791309,6.40363111006797,-7.59396822918313));
#40050=CARTESIAN_POINT('Ctrl Pts',(5.28070658173558,6.65404878042135,-7.60260325901111));
#40051=CARTESIAN_POINT('Ctrl Pts',(4.27825102124085,7.14800517646924,-7.6092187454652));
#40052=CARTESIAN_POINT('Ctrl Pts',(2.6523390834295,7.68419247725851,-7.59572769065918));
#40053=CARTESIAN_POINT('Ctrl Pts',(0.886530195119529,7.96977217997496,-7.58059743549267));
#40054=CARTESIAN_POINT('Ctrl Pts',(-0.8832030571043,7.97003912961983,-7.58058067281829));
#40055=CARTESIAN_POINT('Ctrl Pts',(-2.64903784070115,7.68499899712703,-7.59569267513307));
#40056=CARTESIAN_POINT('Ctrl Pts',(-4.27619364792927,7.14893090541477,-7.60921659325103));
#40057=CARTESIAN_POINT('Ctrl Pts',(-5.27977997084161,6.6545836524422,-7.60262263134438));
#40058=CARTESIAN_POINT('Ctrl Pts',(-5.71954693670857,6.40356646873755,-7.59396605610153));
#40059=CARTESIAN_POINT('Ctrl Pts',(5.83023063406281,6.60192618672222,-7.3778700458245));
#40060=CARTESIAN_POINT('Ctrl Pts',(5.38418897415298,6.85522895262948,-7.38539963283444));
#40061=CARTESIAN_POINT('Ctrl Pts',(4.3646552438395,7.35522359613006,-7.38975351198828));
#40062=CARTESIAN_POINT('Ctrl Pts',(2.70824450483877,7.89916004901893,-7.37351014503725));
#40063=CARTESIAN_POINT('Ctrl Pts',(0.905735068707309,8.18952504203874,-7.35673689298432));
#40064=CARTESIAN_POINT('Ctrl Pts',(-0.902336389694713,8.18979671959776,
-7.35671851944764));
#40065=CARTESIAN_POINT('Ctrl Pts',(-2.70487768650738,7.8999793725258,-7.37347069289444));
#40066=CARTESIAN_POINT('Ctrl Pts',(-4.36256232336407,7.35616125289302,-7.38974696233364));
#40067=CARTESIAN_POINT('Ctrl Pts',(-5.38324694783943,6.85576994589504,-7.38541667426304));
#40068=CARTESIAN_POINT('Ctrl Pts',(-5.83034572764334,6.60186079054662,-7.3778681684244));
#40069=CARTESIAN_POINT('',(-5.72001815070041,6.64700889995603,-7.39409229753282));
#40070=CARTESIAN_POINT('Origin',(-5.89877671949853,6.95919955112704,-7.74135717571565));
#40071=CARTESIAN_POINT('Ctrl Pts',(5.72001488685505,6.64700976236097,-7.39409060170019));
#40072=CARTESIAN_POINT('Ctrl Pts',(5.54310206102047,6.74533606056453,-7.39676017670215));
#40073=CARTESIAN_POINT('Ctrl Pts',(5.36158785252199,6.84067954195826,-7.39860465582333));
#40074=CARTESIAN_POINT('Ctrl Pts',(5.1754616574481,6.93251781017533,-7.39975339332922));
#40075=CARTESIAN_POINT('Ctrl Pts',(4.99269419995749,7.02269881224069,-7.40088140130893));
#40076=CARTESIAN_POINT('Ctrl Pts',(4.80547960727636,7.10949997762252,-7.40133851378473));
#40077=CARTESIAN_POINT('Ctrl Pts',(4.6138337175032,7.19238904742863,-7.40126841792195));
#40078=CARTESIAN_POINT('Ctrl Pts',(4.55683580273732,7.21704130655834,-7.40124757052461));
#40079=CARTESIAN_POINT('Ctrl Pts',(4.49944610286399,7.24134726660044,-7.40118023619262));
#40080=CARTESIAN_POINT('Ctrl Pts',(4.44166550877915,7.26529226398299,-7.40107057479409));
#40081=CARTESIAN_POINT('Ctrl Pts',(4.42850790010658,7.27074494078937,-7.40104560305762));
#40082=CARTESIAN_POINT('Ctrl Pts',(4.41533002256282,7.27617889864318,-7.40101843718722));
#40083=CARTESIAN_POINT('Ctrl Pts',(4.40213190278768,7.28159396299967,-7.40098912934694));
#40084=CARTESIAN_POINT('Ctrl Pts',(4.21117034315222,7.35994369407183,-7.40056507872579));
#40085=CARTESIAN_POINT('Ctrl Pts',(4.01596862780368,7.43435233647871,-7.39968081201011));
#40086=CARTESIAN_POINT('Ctrl Pts',(3.8165986469795,7.50434439156106,-7.39843718528071));
#40087=CARTESIAN_POINT('Ctrl Pts',(3.77349781704224,7.51947563474317,-7.39816833164514));
#40088=CARTESIAN_POINT('Ctrl Pts',(3.73020224843773,7.53440030208692,-7.3978827611826));
#40089=CARTESIAN_POINT('Ctrl Pts',(3.68671278435282,7.54911331686161,-7.39758162520437));
#40090=CARTESIAN_POINT('Ctrl Pts',(3.56438421629974,7.59049855963255,-7.39673458020663));
#40091=CARTESIAN_POINT('Ctrl Pts',(3.44052193650649,7.63021118821232,-7.39576239974459));
#40092=CARTESIAN_POINT('Ctrl Pts',(3.31515060744115,7.66814403300511,-7.39468104272607));
#40093=CARTESIAN_POINT('Ctrl Pts',(3.25246494290849,7.68711045540151,-7.39414036421681));
#40094=CARTESIAN_POINT('Ctrl Pts',(3.18940201028333,7.70563191107659,-7.39357237190721));
#40095=CARTESIAN_POINT('Ctrl Pts',(3.1259655539031,7.72369515016552,-7.3929784612098));
#40096=CARTESIAN_POINT('Ctrl Pts',(3.09424732571298,7.73272676970999,-7.3926815058611));
#40097=CARTESIAN_POINT('Ctrl Pts',(3.06243571634816,7.74164383392144,-7.3923780698253));
#40098=CARTESIAN_POINT('Ctrl Pts',(3.03053121358297,7.75044469037029,-7.3920683036439));
#40099=CARTESIAN_POINT('Ctrl Pts',(3.01457896220038,7.75484511859471,-7.3919134205532));
#40100=CARTESIAN_POINT('Ctrl Pts',(2.99860348745703,7.75921649480437,-7.39175695485891));
#40101=CARTESIAN_POINT('Ctrl Pts',(2.98260485279153,7.76355861313257,-7.39159892310988));
#40102=CARTESIAN_POINT('Ctrl Pts',(2.96757448754333,7.76763793776173,-7.39145045575887));
#40103=CARTESIAN_POINT('Ctrl Pts',(2.9513816149432,7.77199691858728,-7.39128914173787));
#40104=CARTESIAN_POINT('Ctrl Pts',(2.93724511216979,7.77577436204495,-7.39114730518404));
#40105=CARTESIAN_POINT('Ctrl Pts',(2.93633442616335,7.77601770829204,-7.39113816794785));
#40106=CARTESIAN_POINT('Ctrl Pts',(2.93543227902122,7.77625865832359,-7.39112911177721));
#40107=CARTESIAN_POINT('Ctrl Pts',(2.93453953320978,7.77649698869763,-7.39112014540118));
#40108=CARTESIAN_POINT('Ctrl Pts',(2.84807339415212,7.79958027511503,-7.39025171464965));
#40109=CARTESIAN_POINT('Ctrl Pts',(2.76126214800757,7.8216862190474,-7.38937821303356));
#40110=CARTESIAN_POINT('Ctrl Pts',(2.67411779411,7.84279743750039,-7.38851198570502));
#40111=CARTESIAN_POINT('Ctrl Pts',(2.42339777807464,7.90353579623881,-7.38601979292385));
#40112=CARTESIAN_POINT('Ctrl Pts',(2.16992012160589,7.95604400160564,-7.38358730623505));
#40113=CARTESIAN_POINT('Ctrl Pts',(1.91409726142779,7.99999663393151,-7.38140756716427));
#40114=CARTESIAN_POINT('Ctrl Pts',(1.66581451969773,8.042653807151,-7.37929207368423));
#40115=CARTESIAN_POINT('Ctrl Pts',(1.41532240940271,8.07725234402325,-7.37741450777488));
#40116=CARTESIAN_POINT('Ctrl Pts',(1.16300478372367,8.10344682314147,-7.37595930986092));
#40117=CARTESIAN_POINT('Ctrl Pts',(1.07270633115421,8.11282120166089,-7.37543852927947));
#40118=CARTESIAN_POINT('Ctrl Pts',(0.982174166778356,8.12111876850057,-7.37497192963931));
#40119=CARTESIAN_POINT('Ctrl Pts',(0.891426247545732,8.1283221166188,-7.37456827777986));
#40120=CARTESIAN_POINT('Ctrl Pts',(0.634296538441118,8.14873244472201,-7.37342455034148));
#40121=CARTESIAN_POINT('Ctrl Pts',(0.37543293836073,8.16036115306758,-7.37278610170794));
#40122=CARTESIAN_POINT('Ctrl Pts',(0.115324552487338,8.16301820257557,-7.37263966809104));
#40123=CARTESIAN_POINT('Ctrl Pts',(0.0769167899751985,8.16341054412251,
-7.37261804561407));
#40124=CARTESIAN_POINT('Ctrl Pts',(0.0384819294165527,8.16360718853533,
-7.37260715563853));
#40125=CARTESIAN_POINT('Ctrl Pts',(2.15925475930276E-5,8.16360743803404,
-7.37260696056192));
#40126=CARTESIAN_POINT('Ctrl Pts',(-0.258129994921792,8.16360911270702,
-7.3726056511783));
#40127=CARTESIAN_POINT('Ctrl Pts',(-0.515109037614368,8.15480586118552,
-7.37304260681286));
#40128=CARTESIAN_POINT('Ctrl Pts',(-0.770460315820714,8.13735601892008,
-7.37396937370198));
#40129=CARTESIAN_POINT('Ctrl Pts',(-0.809708757097711,8.13467391325662,
-7.37411182122009));
#40130=CARTESIAN_POINT('Ctrl Pts',(-0.848918766915221,8.13178743638375,
-7.37426584593983));
#40131=CARTESIAN_POINT('Ctrl Pts',(-0.888088715740413,8.12869705861704,
-7.37443164063193));
#40132=CARTESIAN_POINT('Ctrl Pts',(-1.08981987124167,8.11278114612515,-7.3752855083498));
#40133=CARTESIAN_POINT('Ctrl Pts',(-1.29048836738904,8.09145876435622,-7.3764512185077));
#40134=CARTESIAN_POINT('Ctrl Pts',(-1.48990484646398,8.06489626046362,-7.37785293389087));
#40135=CARTESIAN_POINT('Ctrl Pts',(-1.73493161452673,8.03225841372874,-7.37957524787252));
#40136=CARTESIAN_POINT('Ctrl Pts',(-1.97805598588168,7.9916870343962,-7.38168071551812));
#40137=CARTESIAN_POINT('Ctrl Pts',(-2.21892777462716,7.94350514881498,-7.3839752327673));
#40138=CARTESIAN_POINT('Ctrl Pts',(-2.33936366899991,7.91941420602437,-7.38512249139189));
#40139=CARTESIAN_POINT('Ctrl Pts',(-2.45923687164102,7.89342169547882,-7.38631515545542));
#40140=CARTESIAN_POINT('Ctrl Pts',(-2.57850627791965,7.86557417008048,-7.38751823647971));
#40141=CARTESIAN_POINT('Ctrl Pts',(-2.60930159135434,7.8583839500586,-7.3878288715234));
#40142=CARTESIAN_POINT('Ctrl Pts',(-2.64005670289387,7.85107009617181,-7.38814014048465));
#40143=CARTESIAN_POINT('Ctrl Pts',(-2.67077082458501,7.84363339425458,-7.38845145415508));
#40144=CARTESIAN_POINT('Ctrl Pts',(-2.69953417933264,7.83666902465455,-7.38874299514819));
#40145=CARTESIAN_POINT('Ctrl Pts',(-2.72826158585112,7.82959691648446,-7.38903457532465));
#40146=CARTESIAN_POINT('Ctrl Pts',(-2.75695259273191,7.82241789298791,-7.38932555207471));
#40147=CARTESIAN_POINT('Ctrl Pts',(-2.78661652972273,7.81499542428396,-7.38962639602959));
#40148=CARTESIAN_POINT('Ctrl Pts',(-2.81624150333557,7.80745862641934,-7.38992665046021));
#40149=CARTESIAN_POINT('Ctrl Pts',(-2.8458269132347,7.79980834038875,-7.39022570062281));
#40150=CARTESIAN_POINT('Ctrl Pts',(-2.86061961818427,7.79598319737345,-7.3903752257041));
#40151=CARTESIAN_POINT('Ctrl Pts',(-2.87540243220805,7.79212968229107,-7.39052444969649));
#40152=CARTESIAN_POINT('Ctrl Pts',(-2.89017528111123,7.7882479020018,-7.39067329341478));
#40153=CARTESIAN_POINT('Ctrl Pts',(-2.90420328195651,7.78456184134173,-7.39081463242254));
#40154=CARTESIAN_POINT('Ctrl Pts',(-2.91705775282148,7.78116066606872,-7.39094394101347));
#40155=CARTESIAN_POINT('Ctrl Pts',(-2.93205612393056,7.77716033250627,-7.39109444591867));
#40156=CARTESIAN_POINT('Ctrl Pts',(-2.93285249596642,7.7769479258549,-7.391102437313));
#40157=CARTESIAN_POINT('Ctrl Pts',(-2.93365490901664,7.77673381813008,-7.39111048831088));
#40158=CARTESIAN_POINT('Ctrl Pts',(-2.93446385852311,7.77651787282764,-7.39111860382889));
#40159=CARTESIAN_POINT('Ctrl Pts',(-3.14099738938505,7.72138470885261,-7.39319058307616));
#40160=CARTESIAN_POINT('Ctrl Pts',(-3.34369757065512,7.66128569454362,-7.39509711240524));
#40161=CARTESIAN_POINT('Ctrl Pts',(-3.54245550567647,7.59674786722476,-7.3966933083795));
#40162=CARTESIAN_POINT('Ctrl Pts',(-3.74549187236312,7.53082080891001,-7.39832386381418));
#40163=CARTESIAN_POINT('Ctrl Pts',(-3.94441448021563,7.46026173758937,-7.39963065398707));
#40164=CARTESIAN_POINT('Ctrl Pts',(-4.13913195941006,7.38558994759841,-7.40048304455997));
#40165=CARTESIAN_POINT('Ctrl Pts',(-4.23997658616605,7.34691725718564,-7.40092449958255));
#40166=CARTESIAN_POINT('Ctrl Pts',(-4.33969369867562,7.30714075765009,-7.40124445291142));
#40167=CARTESIAN_POINT('Ctrl Pts',(-4.43827307181376,7.26632831536047,-7.40142708854303));
#40168=CARTESIAN_POINT('Ctrl Pts',(-4.63592436459349,7.18449951362183,-7.40179327233531));
#40169=CARTESIAN_POINT('Ctrl Pts',(-4.82900095119531,7.09850894800746,-7.4016060823059));
#40170=CARTESIAN_POINT('Ctrl Pts',(-5.01748502204055,7.00887300417893,-7.40076120591469));
#40171=CARTESIAN_POINT('Ctrl Pts',(-5.20992697392762,6.9173548408018,-7.3998985883943));
#40172=CARTESIAN_POINT('Ctrl Pts',(-5.39758156089646,6.82203653720136,-7.39835044074719));
#40173=CARTESIAN_POINT('Ctrl Pts',(-5.5804485117512,6.72342214887826,-7.39602844414171));
#40174=CARTESIAN_POINT('Ctrl Pts',(-5.62728543047245,6.69816447345334,-7.39543372122554));
#40175=CARTESIAN_POINT('Ctrl Pts',(-5.67380837004966,6.67269034805117,-7.39478834450131));
#40176=CARTESIAN_POINT('Ctrl Pts',(-5.72001751101611,6.64700778276234,-7.39409105480892));
#40177=CARTESIAN_POINT('Ctrl Pts',(-5.71200137201152,6.68631702029758,-8.11922551140502));
#40178=CARTESIAN_POINT('Ctrl Pts',(-5.71752593264098,6.68350451781287,-8.11887479851681));
#40179=CARTESIAN_POINT('Ctrl Pts',(-5.76529466296359,6.65838320673758,-8.11644404322045));
#40180=CARTESIAN_POINT('Ctrl Pts',(-5.85056684041905,6.60034318303366,-8.12199201673112));
#40181=CARTESIAN_POINT('Ctrl Pts',(-5.9485659051434,6.49937427859963,-8.15388804757165));
#40182=CARTESIAN_POINT('Ctrl Pts',(-6.01626018410924,6.3902222746575,-8.20520228410394));
#40183=CARTESIAN_POINT('Ctrl Pts',(-6.04733840082506,6.29406348953598,-8.26306349687466));
#40184=CARTESIAN_POINT('Ctrl Pts',(-6.0514193600241,6.23884558946966,-8.30253412448785));
#40185=CARTESIAN_POINT('Ctrl Pts',(-6.05072408266302,6.21774110434867,-8.31866918503377));
#40186=CARTESIAN_POINT('Ctrl Pts',(-5.59593758434029,6.47862795026978,-7.91168787081027));
#40187=CARTESIAN_POINT('Ctrl Pts',(-5.60109254679665,6.47602393259023,-7.91133523079966));
#40188=CARTESIAN_POINT('Ctrl Pts',(-5.64567310121454,6.45276591384098,-7.90883421003711));
#40189=CARTESIAN_POINT('Ctrl Pts',(-5.72536150005282,6.39904474865737,-7.91338893404229));
#40190=CARTESIAN_POINT('Ctrl Pts',(-5.81694503696564,6.30576471974002,-7.94197422327985));
#40191=CARTESIAN_POINT('Ctrl Pts',(-5.88005388554802,6.20535296458813,-7.98843005024452));
#40192=CARTESIAN_POINT('Ctrl Pts',(-5.90885936553763,6.11755368429137,-8.04085370327794));
#40193=CARTESIAN_POINT('Ctrl Pts',(-5.9126015749991,6.06763592744995,-8.076478249824));
#40194=CARTESIAN_POINT('Ctrl Pts',(-5.91196326125511,6.04865028217018,-8.09100475681771));
#40195=CARTESIAN_POINT('Ctrl Pts',(-5.57882413750114,6.48053453245818,-7.59643955907908));
#40196=CARTESIAN_POINT('Ctrl Pts',(-5.58615398423115,6.47687427905703,-7.59596288053133));
#40197=CARTESIAN_POINT('Ctrl Pts',(-5.64947523397066,6.44422885305795,-7.59263309125204));
#40198=CARTESIAN_POINT('Ctrl Pts',(-5.76170274087936,6.3695931524597,-7.59961231738624));
#40199=CARTESIAN_POINT('Ctrl Pts',(-5.89066796668504,6.24048464928553,-7.64046879782618));
#40200=CARTESIAN_POINT('Ctrl Pts',(-5.98090855899055,6.09972137569547,-7.70688735341896));
#40201=CARTESIAN_POINT('Ctrl Pts',(-6.0235971880795,5.97279316563431,-7.78342716853378));
#40202=CARTESIAN_POINT('Ctrl Pts',(-6.02950570161484,5.89741576079667,-7.83730334457995));
#40203=CARTESIAN_POINT('Ctrl Pts',(-6.02850469510944,5.86813423963277,-7.85968193391842));
#40204=CARTESIAN_POINT('Ctrl Pts',(-5.67187599726008,6.6907870813339,-7.38007458214567));
#40205=CARTESIAN_POINT('Ctrl Pts',(-5.68249992573452,6.68549806344202,-7.37943304082086));
#40206=CARTESIAN_POINT('Ctrl Pts',(-5.77420924649652,6.63836645847544,-7.37505910349267));
#40207=CARTESIAN_POINT('Ctrl Pts',(-5.93577462414858,6.53128892558299,-7.38629171363848));
#40208=CARTESIAN_POINT('Ctrl Pts',(-6.12142110281481,6.34631437177203,-7.44695953508515));
#40209=CARTESIAN_POINT('Ctrl Pts',(-6.25273014201225,6.14255171031536,-7.54507961510835));
#40210=CARTESIAN_POINT('Ctrl Pts',(-6.31635964671171,5.95464882433744,-7.65948506785012));
#40211=CARTESIAN_POINT('Ctrl Pts',(-6.32551985612253,5.839736663941,-7.74174959118279));
#40212=CARTESIAN_POINT('Ctrl Pts',(-6.32397418693164,5.79449183343361,-7.77629512811694));
#40213=CARTESIAN_POINT('',(-5.99998809173015,6.09546018036231,-8.13557732097441));
#40214=CARTESIAN_POINT('',(-5.99999999616315,6.4401456877457,-7.42970720374052));
#40215=CARTESIAN_POINT('Ctrl Pts',(-5.99998809173015,6.09546018036231,-8.13557732097441));
#40216=CARTESIAN_POINT('Ctrl Pts',(-5.99998614033837,6.09852832454662,-8.11172602130616));
#40217=CARTESIAN_POINT('Ctrl Pts',(-5.99998781129153,6.10206242548599,-8.08802362797946));
#40218=CARTESIAN_POINT('Ctrl Pts',(-6.00000062824682,6.10612629471922,-8.06456699740365));
#40219=CARTESIAN_POINT('Ctrl Pts',(-6.00000707142059,6.10816923042823,-8.05277518387173));
#40220=CARTESIAN_POINT('Ctrl Pts',(-6.00001566896851,6.11034552813368,-8.04104576003382));
#40221=CARTESIAN_POINT('Ctrl Pts',(-6.0000244752749,6.11265957726614,-8.02939240223511));
#40222=CARTESIAN_POINT('Ctrl Pts',(-6.00004292770159,6.11750835496144,-8.00497436349195));
#40223=CARTESIAN_POINT('Ctrl Pts',(-6.0000639885888,6.12296503416167,-7.98088990423614));
#40224=CARTESIAN_POINT('Ctrl Pts',(-6.00008526219676,6.12903222827216,-7.95725886271824));
#40225=CARTESIAN_POINT('Ctrl Pts',(-6.00009914086696,6.13299039965054,-7.94184222852553));
#40226=CARTESIAN_POINT('Ctrl Pts',(-6.00011245325555,6.13720738562287,-7.92661880791639));
#40227=CARTESIAN_POINT('Ctrl Pts',(-6.00012171175195,6.14167237067045,-7.91162211399328));
#40228=CARTESIAN_POINT('Ctrl Pts',(-6.00013624555423,6.14868141479889,-7.88808060414107));
#40229=CARTESIAN_POINT('Ctrl Pts',(-6.00013967179948,6.15630399211504,-7.86509883736143));
#40230=CARTESIAN_POINT('Ctrl Pts',(-6.00012396232579,6.16445611094957,-7.84279762684001));
#40231=CARTESIAN_POINT('Ctrl Pts',(-6.00011958298537,6.1667286825347,-7.83658070356233));
#40232=CARTESIAN_POINT('Ctrl Pts',(-6.00011380591016,6.16904212195121,-7.83041656999937));
#40233=CARTESIAN_POINT('Ctrl Pts',(-6.00010670568612,6.17139398746753,-7.82430758167122));
#40234=CARTESIAN_POINT('Ctrl Pts',(-6.00010098822625,6.17328782865677,-7.81938831496988));
#40235=CARTESIAN_POINT('Ctrl Pts',(-6.00009441688719,6.17520658170548,-7.81450480268433));
#40236=CARTESIAN_POINT('Ctrl Pts',(-6.00008719772562,6.17714893736528,-7.80965812022649));
#40237=CARTESIAN_POINT('Ctrl Pts',(-6.00006865390096,6.1821382567506,-7.79720847094657));
#40238=CARTESIAN_POINT('Ctrl Pts',(-6.00005102576016,6.18734715796721,-7.78482922322189));
#40239=CARTESIAN_POINT('Ctrl Pts',(-6.00003057015073,6.19268901813973,-7.77273754654777));
#40240=CARTESIAN_POINT('Ctrl Pts',(-6.00000992968195,6.19807915322845,-7.76053659620135));
#40241=CARTESIAN_POINT('Ctrl Pts',(-5.99998595813927,6.20360451483891,-7.7486289442589));
#40242=CARTESIAN_POINT('Ctrl Pts',(-5.9999679154756,6.20912493297519,-7.73722698573307));
#40243=CARTESIAN_POINT('Ctrl Pts',(-5.99995722328527,6.21239636575918,-7.73047011695934));
#40244=CARTESIAN_POINT('Ctrl Pts',(-5.99994890968132,6.21566508061159,-7.72389058671366));
#40245=CARTESIAN_POINT('Ctrl Pts',(-5.99994782973637,6.21889429253799,-7.71752989090999));
#40246=CARTESIAN_POINT('Ctrl Pts',(-5.99994380484488,6.23092937595653,-7.69382395077915));
#40247=CARTESIAN_POINT('Ctrl Pts',(-5.99996594985854,6.2438453349866,-7.67052094837828));
#40248=CARTESIAN_POINT('Ctrl Pts',(-5.99999369856138,6.2576313664447,-7.6478095149004));
#40249=CARTESIAN_POINT('Ctrl Pts',(-6.00002003739153,6.27071694897144,-7.62625201751771));
#40250=CARTESIAN_POINT('Ctrl Pts',(-6.0000506789523,6.28458595267117,-7.60522848329486));
#40251=CARTESIAN_POINT('Ctrl Pts',(-6.00007008721582,6.29917668151905,-7.58489634214688));
#40252=CARTESIAN_POINT('Ctrl Pts',(-6.00007112610709,6.2999576983678,-7.5838079972826));
#40253=CARTESIAN_POINT('Ctrl Pts',(-6.000072134762,6.30074077123508,-7.58272163050395));
#40254=CARTESIAN_POINT('Ctrl Pts',(-6.00007311154347,6.30152588665487,-7.58163726482764));
#40255=CARTESIAN_POINT('Ctrl Pts',(-6.00009137615595,6.31620657972263,-7.56136095988436));
#40256=CARTESIAN_POINT('Ctrl Pts',(-6.00009744663363,6.33160530345637,-7.54178609901824));
#40257=CARTESIAN_POINT('Ctrl Pts',(-6.00008943235725,6.34761295506631,-7.5230490340063));
#40258=CARTESIAN_POINT('Ctrl Pts',(-6.00008131870252,6.36381910421309,-7.50407962627832));
#40259=CARTESIAN_POINT('Ctrl Pts',(-6.00005836465068,6.38064866194837,-7.48596970036587));
#40260=CARTESIAN_POINT('Ctrl Pts',(-6.00003565608961,6.39794656555899,-7.46883145061165));
#40261=CARTESIAN_POINT('Ctrl Pts',(-6.00001753956961,6.41174655120251,-7.45515883421331));
#40262=CARTESIAN_POINT('Ctrl Pts',(-5.99999991840031,6.42584360010603,-7.4421041232633));
#40263=CARTESIAN_POINT('Ctrl Pts',(-5.99999992131821,6.44014555029568,-7.42970704517059));
#40264=CARTESIAN_POINT('Ctrl Pts',(-5.7200186792313,6.64700982300718,-7.39409332430001));
#40265=CARTESIAN_POINT('Ctrl Pts',(-5.77263456945053,6.61776016162055,-7.39330425574794));
#40266=CARTESIAN_POINT('Ctrl Pts',(-5.82217073198462,6.58571612012162,-7.39609700292507));
#40267=CARTESIAN_POINT('Ctrl Pts',(-5.868800030588,6.55119618956499,-7.40209721534042));
#40268=CARTESIAN_POINT('Ctrl Pts',(-5.91542932731003,6.51667626040112,-7.40809742751368));
#40269=CARTESIAN_POINT('Ctrl Pts',(-5.95915199503726,6.47968081216783,-7.41730553493613));
#40270=CARTESIAN_POINT('Ctrl Pts',(-6.00000008250492,6.44014582409289,-7.42970735400782));
#40271=CARTESIAN_POINT('Ctrl Pts',(-5.73278520173054,6.65587881687604,-8.10255227250958));
#40272=CARTESIAN_POINT('Ctrl Pts',(-5.74762629760419,6.64186178191593,-8.09760842313734));
#40273=CARTESIAN_POINT('Ctrl Pts',(-5.76162678132051,6.62763291182143,-8.0934228773982));
#40274=CARTESIAN_POINT('Ctrl Pts',(-5.77478496304676,6.61338734380077,-8.08987534016305));
#40275=CARTESIAN_POINT('Ctrl Pts',(-5.78881567284001,6.59819714238114,-8.08609256329747));
#40276=CARTESIAN_POINT('Ctrl Pts',(-5.80188881891289,6.58298772744398,-8.08303539958181));
#40277=CARTESIAN_POINT('Ctrl Pts',(-5.81403036341231,6.56794750122288,-8.08057762221901));
#40278=CARTESIAN_POINT('Ctrl Pts',(-5.81727080485107,6.56393343428951,-8.0799216691305));
#40279=CARTESIAN_POINT('Ctrl Pts',(-5.8204450272239,6.55993117890586,-8.07930850351914));
#40280=CARTESIAN_POINT('Ctrl Pts',(-5.82355381037148,6.55594381974502,-8.07873591648801));
#40281=CARTESIAN_POINT('Ctrl Pts',(-5.83603219891105,6.53993890254953,-8.07643760132479));
#40282=CARTESIAN_POINT('Ctrl Pts',(-5.84745527801701,6.52417836019587,-8.07479074156169));
#40283=CARTESIAN_POINT('Ctrl Pts',(-5.85790553240099,6.50885077338267,-8.0736434501055));
#40284=CARTESIAN_POINT('Ctrl Pts',(-5.86877308233067,6.49291113125786,-8.07245034544738));
#40285=CARTESIAN_POINT('Ctrl Pts',(-5.87858892580013,6.47743905626987,-8.07179789810214));
#40286=CARTESIAN_POINT('Ctrl Pts',(-5.88745828632321,6.46259199003365,-8.0715436304873));
#40287=CARTESIAN_POINT('Ctrl Pts',(-5.89162957320336,6.45560937021132,-8.07142404766472));
#40288=CARTESIAN_POINT('Ctrl Pts',(-5.8955916611711,6.44876428570152,-8.07139290003505));
#40289=CARTESIAN_POINT('Ctrl Pts',(-5.8993561323307,6.44206972988576,-8.07143712060889));
#40290=CARTESIAN_POINT('Ctrl Pts',(-5.90168368711965,6.43793051755335,-8.07146446198144));
#40291=CARTESIAN_POINT('Ctrl Pts',(-5.90393570203241,6.4338488111739,-8.07152063639131));
#40292=CARTESIAN_POINT('Ctrl Pts',(-5.90611496800989,6.42982732608125,-8.0716027422794));
#40293=CARTESIAN_POINT('Ctrl Pts',(-5.90944521738537,6.42368188612273,-8.0717282125457));
#40294=CARTESIAN_POINT('Ctrl Pts',(-5.91260560611597,6.41767715783716,-8.07191417930119));
#40295=CARTESIAN_POINT('Ctrl Pts',(-5.91560709582519,6.41182246680458,-8.07215001690292));
#40296=CARTESIAN_POINT('Ctrl Pts',(-5.91808990593493,6.4069795096422,-8.07234510002448));
#40297=CARTESIAN_POINT('Ctrl Pts',(-5.92046392144401,6.40223928765411,-8.07257430320933));
#40298=CARTESIAN_POINT('Ctrl Pts',(-5.92273529257371,6.39760620780249,-8.07283214767203));
#40299=CARTESIAN_POINT('Ctrl Pts',(-5.92387097813855,6.39528966787668,-8.07296106990338));
#40300=CARTESIAN_POINT('Ctrl Pts',(-5.9249809953795,6.39299991032722,-8.07309715638919));
#40301=CARTESIAN_POINT('Ctrl Pts',(-5.92606609131996,6.39073744462867,-8.07323976033666));
#40302=CARTESIAN_POINT('Ctrl Pts',(-5.926827454153,6.3891499745906,-8.07333981908851));
#40303=CARTESIAN_POINT('Ctrl Pts',(-5.92726381041733,6.38823388318992,-8.07339909990531));
#40304=CARTESIAN_POINT('Ctrl Pts',(-5.92803487088773,6.38660482663352,-8.07350917997331));
#40305=CARTESIAN_POINT('Ctrl Pts',(-5.92836272745133,6.38591214829637,-8.07355598625401));
#40306=CARTESIAN_POINT('Ctrl Pts',(-5.92875078185222,6.38509044622351,-8.07361219599087));
#40307=CARTESIAN_POINT('Ctrl Pts',(-5.92924734241237,6.3840324112441,-8.07368649483813));
#40308=CARTESIAN_POINT('Ctrl Pts',(-5.93919299879007,6.36284093293236,-8.07517463317085));
#40309=CARTESIAN_POINT('Ctrl Pts',(-5.94793107358897,6.3420071871622,-8.07733441703594));
#40310=CARTESIAN_POINT('Ctrl Pts',(-5.95553872020091,6.32169894627584,-8.08002898480051));
#40311=CARTESIAN_POINT('Ctrl Pts',(-5.95863181590775,6.31344207842914,-8.08112453463471));
#40312=CARTESIAN_POINT('Ctrl Pts',(-5.96153809863311,6.30527152009402,-8.08230877042614));
#40313=CARTESIAN_POINT('Ctrl Pts',(-5.96426303055246,6.29719641142837,-8.08357353496591));
#40314=CARTESIAN_POINT('Ctrl Pts',(-5.97109019756844,6.27696467090637,-8.0867423329412));
#40315=CARTESIAN_POINT('Ctrl Pts',(-5.97677989589696,6.25733527366989,-8.09041450330044));
#40316=CARTESIAN_POINT('Ctrl Pts',(-5.98146315778518,6.23843868552022,-8.09444883517228));
#40317=CARTESIAN_POINT('Ctrl Pts',(-5.98644690024909,6.21832968221606,-8.09874201192454));
#40318=CARTESIAN_POINT('Ctrl Pts',(-5.99029046242889,6.19905036821662,-8.10344555835054));
#40319=CARTESIAN_POINT('Ctrl Pts',(-5.99314481922394,6.18070836123524,-8.10841954843399));
#40320=CARTESIAN_POINT('Ctrl Pts',(-5.99383961628356,6.17624361718492,-8.10963029885263));
#40321=CARTESIAN_POINT('Ctrl Pts',(-5.99447578898681,6.17183419912674,-8.11085719687801));
#40322=CARTESIAN_POINT('Ctrl Pts',(-5.99505550273162,6.16748126860043,-8.11209845041418));
#40323=CARTESIAN_POINT('Ctrl Pts',(-5.99754124264647,6.14881644781163,-8.11742079008077));
#40324=CARTESIAN_POINT('Ctrl Pts',(-5.99899094575813,6.13119319818402,-8.12300451323803));
#40325=CARTESIAN_POINT('Ctrl Pts',(-5.9996181811312,6.11467246052096,-8.12870975260029));
#40326=CARTESIAN_POINT('Ctrl Pts',(-5.99986797364141,6.10809318149992,-8.13098182800101));
#40327=CARTESIAN_POINT('Ctrl Pts',(-5.99998707059393,6.10168833650056,-8.13327352536238));
#40328=CARTESIAN_POINT('Ctrl Pts',(-5.99998809173015,6.09546018036231,-8.13557732097441));
#40329=CARTESIAN_POINT('Ctrl Pts',(-5.72202397771648,10.2826310612706,-17.037335075537));
#40330=CARTESIAN_POINT('Ctrl Pts',(-5.72274491315933,10.3310956803065,-16.560067518738));
#40331=CARTESIAN_POINT('Ctrl Pts',(-5.72404046055613,10.3627269173045,-15.5563860123165));
#40332=CARTESIAN_POINT('Ctrl Pts',(-5.72530462330493,10.1890957103804,-14.0392334779456));
#40333=CARTESIAN_POINT('Ctrl Pts',(-5.72546453572454,9.77722809651949,-12.5261342131263));
#40334=CARTESIAN_POINT('Ctrl Pts',(-5.72471277436271,9.14170964943181,-11.0927040517244));
#40335=CARTESIAN_POINT('Ctrl Pts',(-5.72306496928055,8.29718534881308,-9.7712877786294));
#40336=CARTESIAN_POINT('Ctrl Pts',(-5.7203882568828,7.319416170681,-8.65807750094687));
#40337=CARTESIAN_POINT('Ctrl Pts',(-5.7182966466807,6.59327323403327,-8.03228802666557));
#40338=CARTESIAN_POINT('Ctrl Pts',(-5.71724105953304,6.24681320759565,-7.76998411580299));
#40339=CARTESIAN_POINT('Ctrl Pts',(-5.90002812422718,10.2259058223041,-17.0315448724223));
#40340=CARTESIAN_POINT('Ctrl Pts',(-5.90064109140466,10.273764758127,-16.5568923148414));
#40341=CARTESIAN_POINT('Ctrl Pts',(-5.901741328884,10.3046069941456,-15.5587623015314));
#40342=CARTESIAN_POINT('Ctrl Pts',(-5.90281088151832,10.1313725119932,-14.0503248888921));
#40343=CARTESIAN_POINT('Ctrl Pts',(-5.90294613974592,9.72176930505232,-12.5458334775211));
#40344=CARTESIAN_POINT('Ctrl Pts',(-5.90231016726573,9.09020456074211,-11.1204468081396));
#40345=CARTESIAN_POINT('Ctrl Pts',(-5.90091446861734,8.25108189201988,-9.80603023482109));
#40346=CARTESIAN_POINT('Ctrl Pts',(-5.89863677263844,7.27969287036672,-8.69816806086486));
#40347=CARTESIAN_POINT('Ctrl Pts',(-5.89685243426304,6.55808918076619,-8.07498723699972));
#40348=CARTESIAN_POINT('Ctrl Pts',(-5.89594596532901,6.2137775747096,-7.81368830926344));
#40349=CARTESIAN_POINT('Ctrl Pts',(-6.0072809883487,10.0734860462671,-17.0159867249596));
#40350=CARTESIAN_POINT('Ctrl Pts',(-6.00760395029268,10.1204165494032,-16.548432100775));
#40351=CARTESIAN_POINT('Ctrl Pts',(-6.00818201264186,10.1504140238049,-15.5651446473605));
#40352=CARTESIAN_POINT('Ctrl Pts',(-6.00873882863447,9.97943362493164,-14.0795567262227));
#40353=CARTESIAN_POINT('Ctrl Pts',(-6.0088091981725,9.57592251317866,-12.5976212484565));
#40354=CARTESIAN_POINT('Ctrl Pts',(-6.00847818312919,8.95410325942813,-11.1936935666068));
#40355=CARTESIAN_POINT('Ctrl Pts',(-6.00774957909008,8.12794887207174,-9.89868029665919));
#40356=CARTESIAN_POINT('Ctrl Pts',(-6.00654714904829,7.17173485299533,-8.80693139848031));
#40357=CARTESIAN_POINT('Ctrl Pts',(-6.00559943123166,6.46120738736004,-8.1924918516984));
#40358=CARTESIAN_POINT('Ctrl Pts',(-6.00511044224782,6.12220788075211,-7.9348294930684));
#40359=CARTESIAN_POINT('Ctrl Pts',(-5.99966790381059,9.88747851054264,-16.9970001412723));
#40360=CARTESIAN_POINT('Ctrl Pts',(-5.99963699265514,9.93353691820315,-16.5381342555582));
#40361=CARTESIAN_POINT('Ctrl Pts',(-5.99957878926884,9.96297950349812,-15.5729324201564));
#40362=CARTESIAN_POINT('Ctrl Pts',(-5.99951367917714,9.79519339046945,-14.1150172035289));
#40363=CARTESIAN_POINT('Ctrl Pts',(-5.9995053673528,9.39911971302706,-12.6603941934467));
#40364=CARTESIAN_POINT('Ctrl Pts',(-5.99954420986514,8.78886574866588,-11.2825968892181));
#40365=CARTESIAN_POINT('Ctrl Pts',(-5.99962585484118,7.97796036473452,-10.0114848862901));
#40366=CARTESIAN_POINT('Ctrl Pts',(-5.99973680304981,7.03953062065321,-8.94005066472971));
#40367=CARTESIAN_POINT('Ctrl Pts',(-5.99981416734842,6.34210186098044,-8.33692512051669));
#40368=CARTESIAN_POINT('Ctrl Pts',(-5.99984092736157,6.0094130898816,-8.08405015709546));
#40369=CARTESIAN_POINT('',(-5.99999988467789,9.9132994413493,-16.899370324403));
#40370=CARTESIAN_POINT('Origin',(-5.59998164335621,9.91328771266205,-16.8993697091815));
#40371=CARTESIAN_POINT('Ctrl Pts',(-6.,9.91329812083799,-16.8993691889257));
#40372=CARTESIAN_POINT('Ctrl Pts',(-6.,9.95683978041412,-16.4254094363205));
#40373=CARTESIAN_POINT('Ctrl Pts',(-6.,9.96638815220342,-15.9532839355417));
#40374=CARTESIAN_POINT('Ctrl Pts',(-6.,9.94189523357363,-15.4800412069182));
#40375=CARTESIAN_POINT('Ctrl Pts',(-6.,9.91740229762106,-15.0067981435907));
#40376=CARTESIAN_POINT('Ctrl Pts',(-6.,9.85886802309754,-14.5324378508381));
#40377=CARTESIAN_POINT('Ctrl Pts',(-6.,9.76681037528992,-14.0658326605446));
#40378=CARTESIAN_POINT('Ctrl Pts',(-6.,9.67475272748236,-13.5992274702515));
#40379=CARTESIAN_POINT('Ctrl Pts',(-6.,9.54917170639076,-13.1403773824174));
#40380=CARTESIAN_POINT('Ctrl Pts',(-6.,9.39100129395212,-12.691978875132));
#40381=CARTESIAN_POINT('Ctrl Pts',(-6.,9.23283088151338,-12.2435803678463));
#40382=CARTESIAN_POINT('Ctrl Pts',(-6.,9.04207107772757,-11.8056334411093));
#40383=CARTESIAN_POINT('Ctrl Pts',(-6.,8.82146087395316,-11.3843740208869));
#40384=CARTESIAN_POINT('Ctrl Pts',(-6.,8.60085067017891,-10.9631146006647));
#40385=CARTESIAN_POINT('Ctrl Pts',(-6.,8.35039006641611,-10.5585426869571));
#40386=CARTESIAN_POINT('Ctrl Pts',(-6.,8.07150645159638,-10.1733978041594));
#40387=CARTESIAN_POINT('Ctrl Pts',(-6.,7.79262283677646,-9.78825292136152));
#40388=CARTESIAN_POINT('Ctrl Pts',(-6.,7.48531621089955,-9.42253506947359));
#40389=CARTESIAN_POINT('Ctrl Pts',(-6.,7.15537147961372,-9.08219260210466));
#40390=CARTESIAN_POINT('Ctrl Pts',(-6.,6.82542674832812,-8.74185013473596));
#40391=CARTESIAN_POINT('Ctrl Pts',(-6.,6.47284391163362,-8.42688305188624));
#40392=CARTESIAN_POINT('Ctrl Pts',(-6.,6.09546018150529,-8.13557732045525));
#40393=CARTESIAN_POINT('Origin',(-5.599999999997,9.91330329093349,-16.899368849389));
#40394=CARTESIAN_POINT('Origin',(-5.6,9.91330329095944,-16.8993688494318));
#40395=CARTESIAN_POINT('Ctrl Pts',(-6.05069755286452,4.09530921457736,-9.54399861839001));
#40396=CARTESIAN_POINT('Ctrl Pts',(-6.05139439140886,4.07077799860572,-9.55420987696813));
#40397=CARTESIAN_POINT('Ctrl Pts',(-6.04731517240641,4.00898140897246,-9.58229613908414));
#40398=CARTESIAN_POINT('Ctrl Pts',(-6.01623683914788,3.9107894786984,-9.63664297345575));
#40399=CARTESIAN_POINT('Ctrl Pts',(-5.9485470217377,3.81177761901256,-9.70551105786188));
#40400=CARTESIAN_POINT('Ctrl Pts',(-5.85055617149809,3.73367302953022,-9.77700044850094));
#40401=CARTESIAN_POINT('Ctrl Pts',(-5.76530789870929,3.69985386375794,-9.82447901550751));
#40402=CARTESIAN_POINT('Ctrl Pts',(-5.71756150656501,3.68939776309269,-9.84744168818631));
#40403=CARTESIAN_POINT('Ctrl Pts',(-5.71205470319225,3.68829782904571,-9.85004476031037));
#40404=CARTESIAN_POINT('Ctrl Pts',(-5.91199537999528,3.98270422300683,-9.2837621698363));
#40405=CARTESIAN_POINT('Ctrl Pts',(-5.91263520020597,3.9606235181659,-9.29294359029123));
#40406=CARTESIAN_POINT('Ctrl Pts',(-5.90889416717406,3.90480218592893,-9.31836542063868));
#40407=CARTESIAN_POINT('Ctrl Pts',(-5.88008575414045,3.81549053213944,-9.36819605709431));
#40408=CARTESIAN_POINT('Ctrl Pts',(-5.81697549178688,3.72504770653924,-9.43192966962737));
#40409=CARTESIAN_POINT('Ctrl Pts',(-5.72539191842396,3.65364813821231,-9.49842128531275));
#40410=CARTESIAN_POINT('Ctrl Pts',(-5.64571912788174,3.62284523330527,-9.54266060677016));
#40411=CARTESIAN_POINT('Ctrl Pts',(-5.601155517203,3.61338071461377,-9.5640471330943));
#40412=CARTESIAN_POINT('Ctrl Pts',(-5.59601666916031,3.61238633551412,-9.56647137060792));
#40413=CARTESIAN_POINT('Ctrl Pts',(-6.02851531559025,3.87266147843904,-9.01181418246432));
#40414=CARTESIAN_POINT('Ctrl Pts',(-6.02951858501767,3.83863157203546,-9.02598629563478));
#40415=CARTESIAN_POINT('Ctrl Pts',(-6.02361237825883,3.75427593904666,-9.0643298376604));
#40416=CARTESIAN_POINT('Ctrl Pts',(-5.98092300637074,3.62451976792727,-9.13598611800144));
#40417=CARTESIAN_POINT('Ctrl Pts',(-5.89068726945848,3.49662036141256,-9.22467856542358));
#40418=CARTESIAN_POINT('Ctrl Pts',(-5.76173137337581,3.39668502760156,-9.31605732679907));
#40419=CARTESIAN_POINT('Ctrl Pts',(-5.64953417929655,3.35332938988757,-9.37718983283142));
#40420=CARTESIAN_POINT('Ctrl Pts',(-5.58624215424927,3.33988942963279,-9.40711563376416));
#40421=CARTESIAN_POINT('Ctrl Pts',(-5.57893584696836,3.3384754226433,-9.41051341605323));
#40422=CARTESIAN_POINT('Ctrl Pts',(-6.32391758555148,3.83727685773935,-8.90632479261494));
#40423=CARTESIAN_POINT('Ctrl Pts',(-6.32546665298515,3.78472672174695,-8.92823840796942));
#40424=CARTESIAN_POINT('Ctrl Pts',(-6.31631045619702,3.65602187178656,-8.98662396698808));
#40425=CARTESIAN_POINT('Ctrl Pts',(-6.25268354791552,3.46299417507872,-9.09214836051762));
#40426=CARTESIAN_POINT('Ctrl Pts',(-6.1213889355671,3.27615277066782,-9.21954082369584));
#40427=CARTESIAN_POINT('Ctrl Pts',(-5.93576610989893,3.1311364871012,-9.34938649381138));
#40428=CARTESIAN_POINT('Ctrl Pts',(-5.77425343810608,3.06788321990275,-9.43647681126404));
#40429=CARTESIAN_POINT('Ctrl Pts',(-5.68259198183112,3.04810536026742,-9.47946268409793));
#40430=CARTESIAN_POINT('Ctrl Pts',(-5.67200284155713,3.04602146758907,-9.48434855924641));
#40431=CARTESIAN_POINT('',(-5.7327876945012,3.68906971078177,-9.8154375057469));
#40432=CARTESIAN_POINT('',(-5.7200181592662,3.07996731899951,-9.45352474346443));
#40433=CARTESIAN_POINT('Origin',(-5.89876031575697,3.22462567369242,-9.89750035628898));
#40434=CARTESIAN_POINT('',(-5.99999999681367,3.21424228399819,-9.29218338999141));
#40435=CARTESIAN_POINT('Ctrl Pts',(-6.00000008328868,3.21424234556147,-9.29218358296574));
#40436=CARTESIAN_POINT('Ctrl Pts',(-5.9591513766782,3.1837340995611,-9.32022140189732));
#40437=CARTESIAN_POINT('Ctrl Pts',(-5.91542827662098,3.15726183429538,-9.34765654781793));
#40438=CARTESIAN_POINT('Ctrl Pts',(-5.86879893709601,3.13480561381036,-9.37455156189743));
#40439=CARTESIAN_POINT('Ctrl Pts',(-5.8221695955671,3.11234939236026,-9.40144657713277));
#40440=CARTESIAN_POINT('Ctrl Pts',(-5.77263377979091,3.09390902843134,-9.42780092518505));
#40441=CARTESIAN_POINT('Ctrl Pts',(-5.72001867762027,3.07996773844747,-9.45352603095761));
#40442=CARTESIAN_POINT('',(-5.99998808311064,3.99788652747824,-9.34661203061488));
#40443=CARTESIAN_POINT('Ctrl Pts',(-5.99998808311064,3.99788652747824,-9.34661203061488));
#40444=CARTESIAN_POINT('Ctrl Pts',(-5.99998579341305,3.97186927865861,-9.33574485652103));
#40445=CARTESIAN_POINT('Ctrl Pts',(-5.99998684304345,3.94595612801873,-9.32570975247612));
#40446=CARTESIAN_POINT('Ctrl Pts',(-5.99998299235381,3.92014869004665,-9.31654001952392));
#40447=CARTESIAN_POINT('Ctrl Pts',(-5.99998186343085,3.91258261440246,-9.31385169016598));
#40448=CARTESIAN_POINT('Ctrl Pts',(-5.9999801250393,3.90502573855629,-9.31123744936816));
#40449=CARTESIAN_POINT('Ctrl Pts',(-5.99997728605667,3.89747832269323,-9.30869745889218));
#40450=CARTESIAN_POINT('Ctrl Pts',(-5.99996366357526,3.8612630492276,-9.29650965165367));
#40451=CARTESIAN_POINT('Ctrl Pts',(-5.99992845379828,3.82526738685101,-9.28603455207253));
#40452=CARTESIAN_POINT('Ctrl Pts',(-5.99991579096825,3.78947379315245,-9.2772235887423));
#40453=CARTESIAN_POINT('Ctrl Pts',(-5.99991509405309,3.78750384661685,-9.27673866602585));
#40454=CARTESIAN_POINT('Ctrl Pts',(-5.99991445984403,3.78553450404061,-9.27625877781718));
#40455=CARTESIAN_POINT('Ctrl Pts',(-5.99991389460418,3.78356575918368,-9.2757839149007));
#40456=CARTESIAN_POINT('Ctrl Pts',(-5.99990496077822,3.75244901488712,-9.26827852998715));
#40457=CARTESIAN_POINT('Ctrl Pts',(-5.99990285316706,3.72148342877298,-9.26205336045457));
#40458=CARTESIAN_POINT('Ctrl Pts',(-5.99990386436181,3.6906829130877,-9.25710757884461));
#40459=CARTESIAN_POINT('Ctrl Pts',(-5.99990457445796,3.66905371924126,-9.25363447890509));
#40460=CARTESIAN_POINT('Ctrl Pts',(-5.99990726531124,3.64750534606039,-9.25079193579496));
#40461=CARTESIAN_POINT('Ctrl Pts',(-5.99991517820639,3.62603054452835,-9.24858550131508));
#40462=CARTESIAN_POINT('Ctrl Pts',(-5.99991811031894,3.61807308597285,-9.24776791001381));
#40463=CARTESIAN_POINT('Ctrl Pts',(-5.99992619871551,3.60985636020238,-9.24700745409626));
#40464=CARTESIAN_POINT('Ctrl Pts',(-5.99993158137481,3.60174918672314,-9.24635368447191));
#40465=CARTESIAN_POINT('Ctrl Pts',(-5.99993703257443,3.59353878021062,-9.24569159004464));
#40466=CARTESIAN_POINT('Ctrl Pts',(-5.99993943567107,3.5854410647341,-9.24513895522679));
#40467=CARTESIAN_POINT('Ctrl Pts',(-5.99994447713256,3.57785510414327,-9.24469688598806));
#40468=CARTESIAN_POINT('Ctrl Pts',(-5.99994531264981,3.5765978891561,-9.24462362221802));
#40469=CARTESIAN_POINT('Ctrl Pts',(-5.99994625522812,3.57535475773664,-9.24455328746695));
#40470=CARTESIAN_POINT('Ctrl Pts',(-5.9999473718635,3.57412755605516,-9.24448576306536));
#40471=CARTESIAN_POINT('Ctrl Pts',(-5.99997424819204,3.54459000396275,-9.24286051632755));
#40472=CARTESIAN_POINT('Ctrl Pts',(-5.9999604183843,3.51545932585125,-9.24253390810929));
#40473=CARTESIAN_POINT('Ctrl Pts',(-5.99993587232395,3.48674320219651,-9.24342539985017));
#40474=CARTESIAN_POINT('Ctrl Pts',(-5.99991530510076,3.46268186950695,-9.24417238365708));
#40475=CARTESIAN_POINT('Ctrl Pts',(-5.99988812252707,3.43891057700592,-9.2457750610003));
#40476=CARTESIAN_POINT('Ctrl Pts',(-5.99987117432901,3.41542447440808,-9.24821300048202));
#40477=CARTESIAN_POINT('Ctrl Pts',(-5.99985202935563,3.38889417263689,-9.25096693847068));
#40478=CARTESIAN_POINT('Ctrl Pts',(-5.99984750936127,3.36272649206113,-9.25478616413407));
#40479=CARTESIAN_POINT('Ctrl Pts',(-5.99986528824152,3.33691195950075,-9.25968264302251));
#40480=CARTESIAN_POINT('Ctrl Pts',(-5.9998825122732,3.31190305453613,-9.26442631114418));
#40481=CARTESIAN_POINT('Ctrl Pts',(-5.99992124729762,3.28722486563241,-9.27018190377966));
#40482=CARTESIAN_POINT('Ctrl Pts',(-5.9999558782658,3.26288698839438,-9.27699111499168));
#40483=CARTESIAN_POINT('Ctrl Pts',(-5.99997917531694,3.24651433696959,-9.28157182844347));
#40484=CARTESIAN_POINT('Ctrl Pts',(-5.99999991524942,3.23029611050298,-9.28663002149779));
#40485=CARTESIAN_POINT('Ctrl Pts',(-5.99999992273962,3.2142422154948,-9.29218319195217));
#40486=CARTESIAN_POINT('Ctrl Pts',(-5.99998808311064,3.99788652747824,-9.34661203061488));
#40487=CARTESIAN_POINT('Ctrl Pts',(-5.99998551891527,3.98506101158456,-9.35726021948571));
#40488=CARTESIAN_POINT('Ctrl Pts',(-5.99924019469057,3.97174114049352,-9.36891242702109));
#40489=CARTESIAN_POINT('Ctrl Pts',(-5.99754680958626,3.9580607789439,-9.3815924924929));
#40490=CARTESIAN_POINT('Ctrl Pts',(-5.99687196577081,3.95260891370579,-9.38664572211056));
#40491=CARTESIAN_POINT('Ctrl Pts',(-5.9960463470293,3.94710027549565,-9.39186201124298));
#40492=CARTESIAN_POINT('Ctrl Pts',(-5.99505598210094,3.94154535750297,-9.39724211738209));
#40493=CARTESIAN_POINT('Ctrl Pts',(-5.99264929769866,3.92804635919838,-9.41031630565024));
#40494=CARTESIAN_POINT('Ctrl Pts',(-5.98926946557905,3.9142709411533,-9.42435983375565));
#40495=CARTESIAN_POINT('Ctrl Pts',(-5.98476114128937,3.90038875329463,-9.43935506675853));
#40496=CARTESIAN_POINT('Ctrl Pts',(-5.98055933660131,3.88745041117965,-9.45333077841581));
#40497=CARTESIAN_POINT('Ctrl Pts',(-5.97537763920637,3.87441904409948,-9.46813319482114));
#40498=CARTESIAN_POINT('Ctrl Pts',(-5.96908598668068,3.86147236049078,-9.48372558770977));
#40499=CARTESIAN_POINT('Ctrl Pts',(-5.96754611687718,3.85830368468373,-9.48754179575297));
#40500=CARTESIAN_POINT('Ctrl Pts',(-5.96593972225518,3.85514029170247,-9.49140521264629));
#40501=CARTESIAN_POINT('Ctrl Pts',(-5.96426481102341,3.85198521734112,-9.49531507433625));
#40502=CARTESIAN_POINT('Ctrl Pts',(-5.96381007643915,3.85112862183875,-9.49637659287905));
#40503=CARTESIAN_POINT('Ctrl Pts',(-5.96335029114559,3.85027264058767,-9.49744153437959));
#40504=CARTESIAN_POINT('Ctrl Pts',(-5.96288542932361,3.84941732573222,-9.49850988238613));
#40505=CARTESIAN_POINT('Ctrl Pts',(-5.95829898380248,3.84097857081097,-9.50905047681218));
#40506=CARTESIAN_POINT('Ctrl Pts',(-5.95321825980051,3.83260404402286,-9.51992311623898));
#40507=CARTESIAN_POINT('Ctrl Pts',(-5.94761928869927,3.8243480581809,-9.53110902528923));
#40508=CARTESIAN_POINT('Ctrl Pts',(-5.94481980314865,3.82022006525991,-9.53670197981435));
#40509=CARTESIAN_POINT('Ctrl Pts',(-5.94189071380441,3.81612173192298,-9.54237324806219));
#40510=CARTESIAN_POINT('Ctrl Pts',(-5.93882920492322,3.81206076166437,-9.54811985199363));
#40511=CARTESIAN_POINT('Ctrl Pts',(-5.93729845048262,3.81003027653507,-9.55099315395935));
#40512=CARTESIAN_POINT('Ctrl Pts',(-5.93573458786337,3.80800913398943,-9.55388528957284));
#40513=CARTESIAN_POINT('Ctrl Pts',(-5.93413726119774,3.8059983378373,-9.5567958628498));
#40514=CARTESIAN_POINT('Ctrl Pts',(-5.93307815099486,3.80466507597769,-9.5587257234852));
#40515=CARTESIAN_POINT('Ctrl Pts',(-5.93173234157703,3.80300231282774,-9.56115325118467));
#40516=CARTESIAN_POINT('Ctrl Pts',(-5.93063879374801,3.80167632426087,-9.563104569513));
#40517=CARTESIAN_POINT('Ctrl Pts',(-5.93008307684265,3.80100248609542,-9.5640961864812));
#40518=CARTESIAN_POINT('Ctrl Pts',(-5.92959342566296,3.80041492290089,-9.56496479343206));
#40519=CARTESIAN_POINT('Ctrl Pts',(-5.92924452537267,3.79999801751792,-9.56558248670613));
#40520=CARTESIAN_POINT('Ctrl Pts',(-5.92334532745876,3.79294899109437,-9.57602643007663));
#40521=CARTESIAN_POINT('Ctrl Pts',(-5.91666160167339,3.78561043952302,-9.58734919508044));
#40522=CARTESIAN_POINT('Ctrl Pts',(-5.90905328822459,3.77814425919953,-9.59952402406024));
#40523=CARTESIAN_POINT('Ctrl Pts',(-5.9080903040565,3.7771992648199,-9.60106499206));
#40524=CARTESIAN_POINT('Ctrl Pts',(-5.90711249699386,3.7762522872061,-9.60261958067031));
#40525=CARTESIAN_POINT('Ctrl Pts',(-5.90611957387601,3.77530371017949,-9.60418770868075));
#40526=CARTESIAN_POINT('Ctrl Pts',(-5.89855598182255,3.76807792448518,-9.6161329241212));
#40527=CARTESIAN_POINT('Ctrl Pts',(-5.89011475648501,3.76075622121118,-9.62886574624393));
#40528=CARTESIAN_POINT('Ctrl Pts',(-5.88068114333654,3.75351428035395,-9.64233988204093));
#40529=CARTESIAN_POINT('Ctrl Pts',(-5.87365864584871,3.74812329063701,-9.65237019421252));
#40530=CARTESIAN_POINT('Ctrl Pts',(-5.8660862667034,3.74277711608668,-9.66281092509877));
#40531=CARTESIAN_POINT('Ctrl Pts',(-5.85791979596359,3.7375640109276,-9.67363288992283));
#40532=CARTESIAN_POINT('Ctrl Pts',(-5.84746904137633,3.73089272238804,-9.68748191995446));
#40533=CARTESIAN_POINT('Ctrl Pts',(-5.83604469511993,3.72443720624922,-9.70195661253992));
#40534=CARTESIAN_POINT('Ctrl Pts',(-5.82356408767723,3.71842356605161,-9.71696952444098));
#40535=CARTESIAN_POINT('Ctrl Pts',(-5.81185652587554,3.71278240919366,-9.7310525404089));
#40536=CARTESIAN_POINT('Ctrl Pts',(-5.79921851722962,3.7075311182103,-9.74560902264382));
#40537=CARTESIAN_POINT('Ctrl Pts',(-5.78561697672598,3.70286691787578,-9.76054504582999));
#40538=CARTESIAN_POINT('Ctrl Pts',(-5.77289240786099,3.69850344608074,-9.77451805539834));
#40539=CARTESIAN_POINT('Ctrl Pts',(-5.75932443077255,3.69465358063561,-9.78882332260751));
#40540=CARTESIAN_POINT('Ctrl Pts',(-5.74490786027132,3.69151076355338,-9.80335875951711));
#40541=CARTESIAN_POINT('Ctrl Pts',(-5.74093131861722,3.69064387617281,-9.80736808824939));
#40542=CARTESIAN_POINT('Ctrl Pts',(-5.73689035526843,3.68983099223883,-9.81139476874628));
#40543=CARTESIAN_POINT('Ctrl Pts',(-5.73278520331761,3.68907667806357,-9.81543627503468));
#40544=CARTESIAN_POINT('Ctrl Pts',(-5.71725897249954,3.60560105360399,-9.29487899241727));
#40545=CARTESIAN_POINT('Ctrl Pts',(-5.71831455425541,3.65953286909643,-9.72607755489095));
#40546=CARTESIAN_POINT('Ctrl Pts',(-5.72040614738814,3.838411285377,-10.6678342160512));
#40547=CARTESIAN_POINT('Ctrl Pts',(-5.72308282462462,4.31359609435923,-12.0712148773345));
#40548=CARTESIAN_POINT('Ctrl Pts',(-5.72473060493935,5.03571368099359,-13.4633017408292));
#40549=CARTESIAN_POINT('Ctrl Pts',(-5.72548235451857,5.95934088934631,-14.7303911815181));
#40550=CARTESIAN_POINT('Ctrl Pts',(-5.72532244465371,7.06378884116024,-15.8436279992245));
#40551=CARTESIAN_POINT('Ctrl Pts',(-5.72405830482639,8.29086173581263,-16.7525703081706));
#40552=CARTESIAN_POINT('Ctrl Pts',(-5.72276278486364,9.17588634241873,-17.2270158545483));
#40553=CARTESIAN_POINT('Ctrl Pts',(-5.7220418682695,9.61344013988758,-17.4236767878015));
#40554=CARTESIAN_POINT('Ctrl Pts',(-5.8959561156602,3.65997454462387,-9.28812061696448));
#40555=CARTESIAN_POINT('Ctrl Pts',(-5.89686256011918,3.71411017760644,-9.71695579985479));
#40556=CARTESIAN_POINT('Ctrl Pts',(-5.89864683886563,3.89299890606486,-10.6534764015069));
#40557=CARTESIAN_POINT('Ctrl Pts',(-5.90092445355812,4.36674183318056,-12.0486567166572));
#40558=CARTESIAN_POINT('Ctrl Pts',(-5.90232009808801,5.0854978237521,-13.4325649000885));
#40559=CARTESIAN_POINT('Ctrl Pts',(-5.90295604583695,6.00413540577092,-14.6922077788471));
#40560=CARTESIAN_POINT('Ctrl Pts',(-5.9028207928619,7.10226023811067,-15.799178922291));
#40561=CARTESIAN_POINT('Ctrl Pts',(-5.90175128485163,8.32198322005073,-16.7034195001779));
#40562=CARTESIAN_POINT('Ctrl Pts',(-5.90065109597932,9.20180506054372,-17.175772271617));
#40563=CARTESIAN_POINT('Ctrl Pts',(-5.90003815923874,9.63679110521912,-17.3716501036199));
#40564=CARTESIAN_POINT('Ctrl Pts',(-6.00511200699231,3.81066937852945,-9.26938986800578));
#40565=CARTESIAN_POINT('Ctrl Pts',(-6.0056009722777,3.86431168765211,-9.69180636116294));
#40566=CARTESIAN_POINT('Ctrl Pts',(-6.0065486299692,4.04116833572064,-10.6143641034697));
#40567=CARTESIAN_POINT('Ctrl Pts',(-6.00775098846849,4.50854425402217,-11.9883460169313));
#40568=CARTESIAN_POINT('Ctrl Pts',(-6.00847954447436,5.21698070534443,-13.3513219104762));
#40569=CARTESIAN_POINT('Ctrl Pts',(-6.00881053804551,6.12190713121469,-14.5917956565363));
#40570=CARTESIAN_POINT('Ctrl Pts',(-6.00874017300846,7.20354417012326,-15.6822130904412));
#40571=CARTESIAN_POINT('Ctrl Pts',(-6.00818339521858,8.40460620805652,-16.5730769807682));
#40572=CARTESIAN_POINT('Ctrl Pts',(-6.00760537290816,9.27115183997566,-17.0387401214206));
#40573=CARTESIAN_POINT('Ctrl Pts',(-6.00728243546019,9.69952680962233,-17.2318730621056));
#40574=CARTESIAN_POINT('Ctrl Pts',(-5.9998408175774,3.99628885031533,-9.24631810374516));
#40575=CARTESIAN_POINT('Ctrl Pts',(-5.99981404844536,4.04894055408171,-9.66087586636771));
#40576=CARTESIAN_POINT('Ctrl Pts',(-5.99973665412961,4.22254844296643,-10.5664333418028));
#40577=CARTESIAN_POINT('Ctrl Pts',(-5.99962568094289,4.68122376165327,-11.9148571729911));
#40578=CARTESIAN_POINT('Ctrl Pts',(-5.99954401753405,5.37658608631832,-13.2526773418967));
#40579=CARTESIAN_POINT('Ctrl Pts',(-5.9995051673635,6.26466620718276,-14.4700709223921));
#40580=CARTESIAN_POINT('Ctrl Pts',(-5.99951348071399,7.32636941191874,-15.540391859643));
#40581=CARTESIAN_POINT('Ctrl Pts',(-5.99957860435503,8.5050642212501,-16.4146537204691));
#40582=CARTESIAN_POINT('Ctrl Pts',(-5.99963682031295,9.35567047233198,-16.8717549394652));
#40583=CARTESIAN_POINT('Ctrl Pts',(-5.99966773898728,9.77608509663727,-17.0612989188918));
#40584=CARTESIAN_POINT('',(-5.99999997114735,9.67863337142275,-17.0348538902779));
#40585=CARTESIAN_POINT('Ctrl Pts',(-6.,3.99788652645587,-9.34661203134569));
#40586=CARTESIAN_POINT('Ctrl Pts',(-6.,4.06147282871,-9.81908885364613));
#40587=CARTESIAN_POINT('Ctrl Pts',(-6.,4.15795093339124,-10.2819181268309));
#40588=CARTESIAN_POINT('Ctrl Pts',(-6.,4.28772381294125,-10.7378299097621));
#40589=CARTESIAN_POINT('Ctrl Pts',(-6.,4.41749669249136,-11.1937416926937));
#40590=CARTESIAN_POINT('Ctrl Pts',(-6.,4.5805643469103,-11.6427359853717));
#40591=CARTESIAN_POINT('Ctrl Pts',(-6.,4.77466779593315,-12.0768287139941));
#40592=CARTESIAN_POINT('Ctrl Pts',(-6.,4.96877124495587,-12.5109214426161));
#40593=CARTESIAN_POINT('Ctrl Pts',(-6.,5.19391048858245,-12.9301126071823));
#40594=CARTESIAN_POINT('Ctrl Pts',(-6.,5.44842673883702,-13.3317963333689));
#40595=CARTESIAN_POINT('Ctrl Pts',(-6.,5.70294298909176,-13.7334800595558));
#40596=CARTESIAN_POINT('Ctrl Pts',(-6.,5.98683624597452,-14.1176563473629));
#40597=CARTESIAN_POINT('Ctrl Pts',(-6.,6.29607553925051,-14.4788351908868));
#40598=CARTESIAN_POINT('Ctrl Pts',(-6.,6.60531483252628,-14.8400140344105));
#40599=CARTESIAN_POINT('Ctrl Pts',(-6.,6.93990016219523,-15.1781954336509));
#40600=CARTESIAN_POINT('Ctrl Pts',(-6.,7.29796328415509,-15.49122228417));
#40601=CARTESIAN_POINT('Ctrl Pts',(-6.,7.6560264061152,-15.8042491346892));
#40602=CARTESIAN_POINT('Ctrl Pts',(-6.,8.03756732036623,-16.092121436487));
#40603=CARTESIAN_POINT('Ctrl Pts',(-6.,8.43516135621591,-16.3499544612483));
#40604=CARTESIAN_POINT('Ctrl Pts',(-6.,8.83275511078938,-16.6077873036066));
#40605=CARTESIAN_POINT('Ctrl Pts',(-6.,9.24640196424807,-16.8355809114308));
#40606=CARTESIAN_POINT('Ctrl Pts',(-6.,9.67863396563729,-17.0348526013916));
#40607=CARTESIAN_POINT('',(-5.736443569433,9.52121843706297,-17.3763278265689));
#40608=CARTESIAN_POINT('Origin',(-5.59998163814024,9.67863859077867,-17.0348433699263));
#40609=CARTESIAN_POINT('Ctrl Pts',(-5.73278790982,3.68906911002063,-9.81543761164561));
#40610=CARTESIAN_POINT('Ctrl Pts',(-5.73461480971437,3.83284536504953,-10.625338532278));
#40611=CARTESIAN_POINT('Ctrl Pts',(-5.73605973940222,4.07387518415476,-11.4195438253679));
#40612=CARTESIAN_POINT('Ctrl Pts',(-5.73818934991407,4.74008576935209,-12.9297554454633));
#40613=CARTESIAN_POINT('Ctrl Pts',(-5.73887403073807,5.16463847589479,-13.645990507428));
#40614=CARTESIAN_POINT('Ctrl Pts',(-5.73948314352221,6.17415914950061,-14.9577795832333));
#40615=CARTESIAN_POINT('Ctrl Pts',(-5.73940757548236,6.75884789279361,-15.5535353420817));
#40616=CARTESIAN_POINT('Ctrl Pts',(-5.7384961905792,8.05516229836731,-16.5887322234374));
#40617=CARTESIAN_POINT('Ctrl Pts',(-5.73766037378333,8.76684603319029,-17.0280903649815));
#40618=CARTESIAN_POINT('Ctrl Pts',(-5.73644356975675,9.52121823635002,-17.3763277339147));
#40619=CARTESIAN_POINT('Origin',(-5.599999999997,9.67863108576248,-17.0348569102134));
#40620=CARTESIAN_POINT('',(-5.593361696257,9.87744142979155,-17.381887715825));
#40621=CARTESIAN_POINT('Origin',(-5.599999999997,9.67863108576248,-17.0348569102134));
#40622=CARTESIAN_POINT('Origin',(-5.6,9.67863108578652,-17.0348569102573));
#40623=CARTESIAN_POINT('Ctrl Pts',(-5.59335880963397,9.87743876208659,-17.3818891889333));
#40624=CARTESIAN_POINT('Ctrl Pts',(-5.59335897597999,9.88085962292803,-17.3799294167645));
#40625=CARTESIAN_POINT('Ctrl Pts',(-5.59336249921671,9.95658496857357,-17.3365326542547));
#40626=CARTESIAN_POINT('Ctrl Pts',(-5.59336249921671,10.0355852075694,-17.2909218450052));
#40627=CARTESIAN_POINT('Ctrl Pts',(-5.59335897598,10.111030579166,-17.2470401532232));
#40628=CARTESIAN_POINT('Ctrl Pts',(-5.59335880963398,10.1144382220706,-17.2450574869161));
#40629=CARTESIAN_POINT('Ctrl Pts',(-5.83074004396025,9.87939819740572,-17.3853094563155));
#40630=CARTESIAN_POINT('Ctrl Pts',(-5.83074021194161,9.88281933951928,-17.3833494092223));
#40631=CARTESIAN_POINT('Ctrl Pts',(-5.83074376981389,9.95855095781735,-17.3399466417504));
#40632=CARTESIAN_POINT('Ctrl Pts',(-5.83074376981389,10.037558812847,-17.2943314353818));
#40633=CARTESIAN_POINT('Ctrl Pts',(-5.83074021194162,10.1130125212196,-17.2504473138044));
#40634=CARTESIAN_POINT('Ctrl Pts',(-5.83074004396027,10.1164205428518,-17.2484645413707));
#40635=CARTESIAN_POINT('Ctrl Pts',(-6.00000347484088,9.79664251978775,-17.2408563365192));
#40636=CARTESIAN_POINT('Ctrl Pts',(-6.00000357357708,9.800049674696,-17.2389042214154));
#40637=CARTESIAN_POINT('Ctrl Pts',(-6.00000566482435,9.87547170312966,-17.1956771557313));
#40638=CARTESIAN_POINT('Ctrl Pts',(-6.00000566482435,9.95415740030959,-17.1502479472839));
#40639=CARTESIAN_POINT('Ctrl Pts',(-6.00000357357708,10.0293041515383,-17.1065440874999));
#40640=CARTESIAN_POINT('Ctrl Pts',(-6.00000347484088,10.0326983102635,-17.1045694623467));
#40641=CARTESIAN_POINT('Ctrl Pts',(-5.9999999999769,9.67862555753756,-17.0348533301202));
#40642=CARTESIAN_POINT('Ctrl Pts',(-5.99999999996752,9.68201281535372,-17.0329126138548));
#40643=CARTESIAN_POINT('Ctrl Pts',(-5.99999999976693,9.75699439869606,-16.9899379593609));
#40644=CARTESIAN_POINT('Ctrl Pts',(-5.99999999976693,9.83522068191858,-16.9447739936855));
#40645=CARTESIAN_POINT('Ctrl Pts',(-5.99999999996752,9.90992861609885,-16.9013253649444));
#40646=CARTESIAN_POINT('Ctrl Pts',(-5.9999999999769,9.91330295459431,-16.8993622717592));
#40647=CARTESIAN_POINT('Origin',(-5.47625714583714,-8.61393265067164,14.9197686319482));
#40648=CARTESIAN_POINT('Ctrl Pts',(-6.00000000001697,9.67863488297892,-17.0348530243128));
#40649=CARTESIAN_POINT('Ctrl Pts',(-6.00000000001004,9.6820198209521,-17.0329138284621));
#40650=CARTESIAN_POINT('Ctrl Pts',(-6.00000000000346,9.68540450272322,-17.0309741411835));
#40651=CARTESIAN_POINT('Ctrl Pts',(-5.9999999999973,9.68878892526243,-17.0290339620093));
#40652=CARTESIAN_POINT('Ctrl Pts',(-5.99999999993208,9.72458345046399,-17.0085141269286));
#40653=CARTESIAN_POINT('Ctrl Pts',(-5.99999999990817,9.76034897938042,-16.9879392663609));
#40654=CARTESIAN_POINT('Ctrl Pts',(-5.99999999990817,9.79608195797508,-16.9673088199789));
#40655=CARTESIAN_POINT('Ctrl Pts',(-5.99999999990817,9.83181480046151,-16.9466784521789));
#40656=CARTESIAN_POINT('Ctrl Pts',(-5.99999999993208,9.86751509308548,-16.9259924988652));
#40657=CARTESIAN_POINT('Ctrl Pts',(-5.9999999999973,9.90318155031143,-16.9052543226814));
#40658=CARTESIAN_POINT('Ctrl Pts',(-6.00000000000346,9.90655401254468,-16.9032934125881));
#40659=CARTESIAN_POINT('Ctrl Pts',(-6.00000000001004,9.90992617229324,-16.9013320355928));
#40660=CARTESIAN_POINT('Ctrl Pts',(-6.00000000001697,9.91329802845247,-16.8993701945575));
#40661=CARTESIAN_POINT('Ctrl Pts',(-5.67770424700723,9.69013290714839,-17.4901834495681));
#40662=CARTESIAN_POINT('Ctrl Pts',(-3.78513616467149,8.87579171292761,-17.9133901356215));
#40663=CARTESIAN_POINT('Ctrl Pts',(-2.06853043374644E-10,8.0559151625809,
-18.3263289253002));
#40664=CARTESIAN_POINT('Ctrl Pts',(3.78513616425752,8.87579171283821,-17.913390135667));
#40665=CARTESIAN_POINT('Ctrl Pts',(5.67770424638677,9.69013290687893,-17.4901834497026));
#40666=CARTESIAN_POINT('Ctrl Pts',(-5.67770424700723,9.88675274008847,-17.3789457438659));
#40667=CARTESIAN_POINT('Ctrl Pts',(-3.78513616467149,9.58462619244214,-17.5169198758068));
#40668=CARTESIAN_POINT('Ctrl Pts',(-2.06853045109368E-10,9.35278546520724,
-17.7857301779258));
#40669=CARTESIAN_POINT('Ctrl Pts',(3.78513616425752,9.58462619241777,-17.5169198758378));
#40670=CARTESIAN_POINT('Ctrl Pts',(5.67770424638677,9.88675273998615,-17.3789457439054));
#40671=CARTESIAN_POINT('Ctrl Pts',(-5.67770424700723,10.0824918035142,-17.2660281226572));
#40672=CARTESIAN_POINT('Ctrl Pts',(-3.78513616467149,10.2888806489686,-17.1108358236266));
#40673=CARTESIAN_POINT('Ctrl Pts',(-2.06853409401297E-10,10.576208809251,
-17.0878170844136));
#40674=CARTESIAN_POINT('Ctrl Pts',(3.78513616425752,10.2888806489984,-17.1108358236215));
#40675=CARTESIAN_POINT('Ctrl Pts',(5.67770424638677,10.0824918035797,-17.2660281226026));
#40676=CARTESIAN_POINT('Ctrl Pts',(-5.67770424700723,10.2772218172614,-17.1515046485292));
#40677=CARTESIAN_POINT('Ctrl Pts',(-3.78513616467149,10.9871582910923,-16.6959444169702));
#40678=CARTESIAN_POINT('Ctrl Pts',(-2.0685344062632E-10,11.7011732380177,
-16.2470303047039));
#40679=CARTESIAN_POINT('Ctrl Pts',(3.78513616425752,10.9871582911679,-16.6959444169159));
#40680=CARTESIAN_POINT('Ctrl Pts',(5.67770424638677,10.2772218174911,-17.1515046483743));
#40681=CARTESIAN_POINT('Ctrl Pts',(-5.5933616962572,9.8774414297856,-17.3818877158146));
#40682=CARTESIAN_POINT('Ctrl Pts',(-5.58011194449613,9.87199617872778,-17.3847537905975));
#40683=CARTESIAN_POINT('Ctrl Pts',(-5.56077715143487,9.86405587308934,-17.3889346813685));
#40684=CARTESIAN_POINT('Ctrl Pts',(-5.53532113652999,9.85368788323714,-17.3943993484187));
#40685=CARTESIAN_POINT('Ctrl Pts',(-5.50995410366162,9.84335613491194,-17.3998449136101));
#40686=CARTESIAN_POINT('Ctrl Pts',(-5.47850841230432,9.83061363966293,-17.4065654390655));
#40687=CARTESIAN_POINT('Ctrl Pts',(-5.440927579018,9.81556929477701,-17.4145088993808));
#40688=CARTESIAN_POINT('Ctrl Pts',(-5.41351892178665,9.80459707154005,-17.420302266956));
#40689=CARTESIAN_POINT('Ctrl Pts',(-5.38284643787845,9.79240132902821,-17.4267457139548));
#40690=CARTESIAN_POINT('Ctrl Pts',(-5.34888208855784,9.77903861936218,-17.4338110542043));
#40691=CARTESIAN_POINT('Ctrl Pts',(-5.30328372218514,9.76109869873152,-17.4432965288177));
#40692=CARTESIAN_POINT('Ctrl Pts',(-5.25175264298193,9.74105373926007,-17.4539038384112));
#40693=CARTESIAN_POINT('Ctrl Pts',(-5.19420651583573,9.71907748007655,-17.465544925654));
#40694=CARTESIAN_POINT('Ctrl Pts',(-5.15775181712237,9.70515581502086,-17.4729193980846));
#40695=CARTESIAN_POINT('Ctrl Pts',(-5.11888293091578,9.69045994364656,-17.4807082620169));
#40696=CARTESIAN_POINT('Ctrl Pts',(-5.0775760599003,9.67504302649964,-17.4888837519901));
#40697=CARTESIAN_POINT('Ctrl Pts',(-5.01428285603189,9.65142017499784,-17.5014107950915));
#40698=CARTESIAN_POINT('Ctrl Pts',(-4.94526616581234,9.62610223170551,-17.5148467864822));
#40699=CARTESIAN_POINT('Ctrl Pts',(-4.87042972055464,9.59931641119694,-17.5290729156207));
#40700=CARTESIAN_POINT('Ctrl Pts',(-4.84061386073117,9.58864457521129,-17.5347407993739));
#40701=CARTESIAN_POINT('Ctrl Pts',(-4.80987409122418,9.57774022043901,-17.5405338235698));
#40702=CARTESIAN_POINT('Ctrl Pts',(-4.77820388113395,9.56661968261119,-17.5464433139158));
#40703=CARTESIAN_POINT('Ctrl Pts',(-4.70106691667843,9.53953414927539,-17.5608366553389));
#40704=CARTESIAN_POINT('Ctrl Pts',(-4.61841080073076,9.51116306793432,-17.5759226414519));
#40705=CARTESIAN_POINT('Ctrl Pts',(-4.53013500070397,9.48177397814663,-17.5915598828748));
#40706=CARTESIAN_POINT('Ctrl Pts',(-4.50293141539754,9.47271726485856,-17.5963787463784));
#40707=CARTESIAN_POINT('Ctrl Pts',(-4.47519409959358,9.46356419349808,-17.6012497792823));
#40708=CARTESIAN_POINT('Ctrl Pts',(-4.44691998668231,9.45432346338256,-17.6061683461136));
#40709=CARTESIAN_POINT('Ctrl Pts',(-4.35781348566433,9.4252010951573,-17.6216693198041));
#40710=CARTESIAN_POINT('Ctrl Pts',(-4.26337571436441,9.39520473748902,-17.6376442626533));
#40711=CARTESIAN_POINT('Ctrl Pts',(-4.16350853538153,9.36463621112325,-17.6539330750319));
#40712=CARTESIAN_POINT('Ctrl Pts',(-4.13544286586689,9.35604553932027,-17.6585107193557));
#40713=CARTESIAN_POINT('Ctrl Pts',(-4.10694837447457,9.3474099522417,-17.6631130001808));
#40714=CARTESIAN_POINT('Ctrl Pts',(-4.07802284616762,9.3387368036049,-17.6677359985849));
#40715=CARTESIAN_POINT('Ctrl Pts',(-3.98966527509743,9.31224330834538,-17.681857673588));
#40716=CARTESIAN_POINT('Ctrl Pts',(-3.89728568477082,9.28539730969706,-17.6961737677151));
#40717=CARTESIAN_POINT('Ctrl Pts',(-3.80082222259122,9.25842603150079,-17.7105635640497));
#40718=CARTESIAN_POINT('Ctrl Pts',(-3.75631511471526,9.24598180068934,-17.7172028469792));
#40719=CARTESIAN_POINT('Ctrl Pts',(-3.71093864267729,9.23351127863602,-17.7238576120777));
#40720=CARTESIAN_POINT('Ctrl Pts',(-3.66468681174934,9.22103880866935,-17.7305148894988));
#40721=CARTESIAN_POINT('Ctrl Pts',(-3.6291388814236,9.21145279911104,-17.7356314963266));
#40722=CARTESIAN_POINT('Ctrl Pts',(-3.59307387138023,9.20186566495838,-17.7407495726304));
#40723=CARTESIAN_POINT('Ctrl Pts',(-3.55648921837644,9.19228894191619,-17.7458629834574));
#40724=CARTESIAN_POINT('Ctrl Pts',(-3.51439653036569,9.18127038680953,-17.7517462484041));
#40725=CARTESIAN_POINT('Ctrl Pts',(-3.47161588281534,9.1702654167767,-17.7576234419693));
#40726=CARTESIAN_POINT('Ctrl Pts',(-3.42814354335167,9.1592925882825,-17.7634846849554));
#40727=CARTESIAN_POINT('Ctrl Pts',(-3.40640737361983,9.1538061740354,-17.7664153064484));
#40728=CARTESIAN_POINT('Ctrl Pts',(-3.38449828090911,9.1483277950983,-17.7693419401528));
#40729=CARTESIAN_POINT('Ctrl Pts',(-3.36241579598645,9.14285982146657,-17.7722633232205));
#40730=CARTESIAN_POINT('Ctrl Pts',(-3.35137455352512,9.1401258346507,-17.7737240147544));
#40731=CARTESIAN_POINT('Ctrl Pts',(-3.34028996301079,9.13739444915452,-17.7751833936165));
#40732=CARTESIAN_POINT('Ctrl Pts',(-3.32916196703421,9.13466596612807,-17.776641299268));
#40733=CARTESIAN_POINT('Ctrl Pts',(-3.32359796904591,9.13330172461484,-17.7773702520937));
#40734=CARTESIAN_POINT('Ctrl Pts',(-3.31802311969206,9.1319382087186,-17.778098836616));
#40735=CARTESIAN_POINT('Ctrl Pts',(-3.31243741184863,9.13057545642724,-17.7788270325796));
#40736=CARTESIAN_POINT('Ctrl Pts',(-3.3068517040052,9.12921270413588,-17.7795552285433));
#40737=CARTESIAN_POINT('Ctrl Pts',(-3.30243415517163,9.12813691830816,-17.7801300933024));
#40738=CARTESIAN_POINT('Ctrl Pts',(-3.29564770574228,9.12648952845955,-17.7810104344809));
#40739=CARTESIAN_POINT('Ctrl Pts',(-3.26393770760084,9.11879202336772,-17.7851238692638));
#40740=CARTESIAN_POINT('Ctrl Pts',(-3.23232942717988,9.11123014550933,-17.7891654603057));
#40741=CARTESIAN_POINT('Ctrl Pts',(-3.20082427869682,9.10380211593025,-17.7931361187594));
#40742=CARTESIAN_POINT('Ctrl Pts',(-3.02528951599938,9.06241594661338,-17.8152591247753));
#40743=CARTESIAN_POINT('Ctrl Pts',(-2.85295938427949,9.02518586220078,-17.8351795195926));
#40744=CARTESIAN_POINT('Ctrl Pts',(-2.68407158453179,8.99178486883743,-17.8530663542106));
#40745=CARTESIAN_POINT('Ctrl Pts',(-2.50184039212567,8.95574494850426,-17.8723663818364));
#40746=CARTESIAN_POINT('Ctrl Pts',(-2.32361766415623,8.9241624222754,-17.8892991455982));
#40747=CARTESIAN_POINT('Ctrl Pts',(-2.14966969634919,8.89659677674154,-17.9040935676009));
#40748=CARTESIAN_POINT('Ctrl Pts',(-2.13682621314835,8.89456146175742,-17.9051859167261));
#40749=CARTESIAN_POINT('Ctrl Pts',(-2.12400601123722,8.89254804288692,-17.9062666104474));
#40750=CARTESIAN_POINT('Ctrl Pts',(-2.11120918688827,8.89055634176565,-17.9073357418195));
#40751=CARTESIAN_POINT('Ctrl Pts',(-1.93623842500656,8.86332384617726,-17.9219539569042));
#40752=CARTESIAN_POINT('Ctrl Pts',(-1.76564250964608,8.84015095694756,-17.9344106798837));
#40753=CARTESIAN_POINT('Ctrl Pts',(-1.59965452899343,8.82056074414114,-17.9449536053094));
#40754=CARTESIAN_POINT('Ctrl Pts',(-1.55746334879606,8.81558126191978,-17.9476334286599));
#40755=CARTESIAN_POINT('Ctrl Pts',(-1.51556961880659,8.81083328673493,-17.95018959672));
#40756=CARTESIAN_POINT('Ctrl Pts',(-1.47397664556802,8.8063090668019,-17.9526261566541));
#40757=CARTESIAN_POINT('Ctrl Pts',(-1.30951026857606,8.78841945701537,-17.9622607692697));
#40758=CARTESIAN_POINT('Ctrl Pts',(-1.14975024394602,8.77402676598206,-17.9700258867514));
#40759=CARTESIAN_POINT('Ctrl Pts',(-0.994879319579393,8.76263737856074,
-17.9761785830586));
#40760=CARTESIAN_POINT('Ctrl Pts',(-0.923028843571489,8.75735341121175,
-17.9790330514503));
#40761=CARTESIAN_POINT('Ctrl Pts',(-0.852229999824751,8.75271615434218,
-17.9815403518941));
#40762=CARTESIAN_POINT('Ctrl Pts',(-0.782497653221542,8.74867785693833,
-17.9837255207404));
#40763=CARTESIAN_POINT('Ctrl Pts',(-0.633185211092702,8.74003096526203,
-17.988404452582));
#40764=CARTESIAN_POINT('Ctrl Pts',(-0.48876513848955,8.73412787932249,-17.9916073647212));
#40765=CARTESIAN_POINT('Ctrl Pts',(-0.349359262933425,8.73049489884206,
-17.9935789001746));
#40766=CARTESIAN_POINT('Ctrl Pts',(-0.262262031653481,8.72822510540704,
-17.9948106651822));
#40767=CARTESIAN_POINT('Ctrl Pts',(-0.177121215541505,8.72684207671218,
-17.9955615210256));
#40768=CARTESIAN_POINT('Ctrl Pts',(-0.0939590014244084,8.72623675497946,
-17.9958885074368));
#40769=CARTESIAN_POINT('Ctrl Pts',(0.0408293133112234,8.72525565680773,
-17.9964184830725));
#40770=CARTESIAN_POINT('Ctrl Pts',(0.170418217022037,8.72631579691311,-17.9958363492441));
#40771=CARTESIAN_POINT('Ctrl Pts',(0.294737354709391,8.72898124266637,-17.9943858101474));
#40772=CARTESIAN_POINT('Ctrl Pts',(0.343121177597331,8.730018608736,-17.9938212741632));
#40773=CARTESIAN_POINT('Ctrl Pts',(0.390707155839702,8.73129949621115,-17.9931249665939));
#40774=CARTESIAN_POINT('Ctrl Pts',(0.437492444106394,8.73279961278336,-17.9923103622705));
#40775=CARTESIAN_POINT('Ctrl Pts',(0.473998627888868,8.73397014166774,-17.991674733075));
#40776=CARTESIAN_POINT('Ctrl Pts',(0.510017321629045,8.73527416507888,-17.990967068312));
#40777=CARTESIAN_POINT('Ctrl Pts',(0.545547455340001,8.7367004771479,-17.9901935606565));
#40778=CARTESIAN_POINT('Ctrl Pts',(0.575306016459619,8.73789509676928,-17.9895457028402));
#40779=CARTESIAN_POINT('Ctrl Pts',(0.604721856468692,8.73917550597213,-17.988851653594));
#40780=CARTESIAN_POINT('Ctrl Pts',(0.633794572981875,8.74053515190824,-17.9881150240992));
#40781=CARTESIAN_POINT('Ctrl Pts',(0.665686567166257,8.74202664721683,-17.987306961201));
#40782=CARTESIAN_POINT('Ctrl Pts',(0.697165584262103,8.74361348041315,-17.9864476655722));
#40783=CARTESIAN_POINT('Ctrl Pts',(0.728231308503099,8.74528723796721,-17.985541761664));
#40784=CARTESIAN_POINT('Ctrl Pts',(0.743764170623598,8.74612411674424,-17.9850888097099));
#40785=CARTESIAN_POINT('Ctrl Pts',(0.759193709529455,8.74698272644005,-17.984624205335));
#40786=CARTESIAN_POINT('Ctrl Pts',(0.774519880040027,8.74786203977384,-17.9841485121783));
#40787=CARTESIAN_POINT('Ctrl Pts',(0.782182965295312,8.74830169644073,-17.9839106656));
#40788=CARTESIAN_POINT('Ctrl Pts',(0.789820208451713,8.74874652900686,-17.983670046805));
#40789=CARTESIAN_POINT('Ctrl Pts',(0.797431605159051,8.74919640992754,-17.9834267256678));
#40790=CARTESIAN_POINT('Ctrl Pts',(0.805043001866389,8.74964629084823,-17.9831834045305));
#40791=CARTESIAN_POINT('Ctrl Pts',(0.814391076480518,8.7502084329586,-17.9828794075472));
#40792=CARTESIAN_POINT('Ctrl Pts',(0.820188251806143,8.75056107063619,-17.982688724792));
#40793=CARTESIAN_POINT('Ctrl Pts',(0.913106248232728,8.75621320027285,-17.9796324329662));
#40794=CARTESIAN_POINT('Ctrl Pts',(1.01092014190408,8.76311877591221,-17.9759012853841));
#40795=CARTESIAN_POINT('Ctrl Pts',(1.11357262060553,8.77158708174356,-17.971331569502));
#40796=CARTESIAN_POINT('Ctrl Pts',(1.22621187672514,8.78087924576631,-17.9663172785259));
#40797=CARTESIAN_POINT('Ctrl Pts',(1.34467778636123,8.79205294515384,-17.9602933731797));
#40798=CARTESIAN_POINT('Ctrl Pts',(1.46886551454821,8.80554585695815,-17.9530280626319));
#40799=CARTESIAN_POINT('Ctrl Pts',(1.5153544234466,8.81059684514194,-17.9503083385085));
#40800=CARTESIAN_POINT('Ctrl Pts',(1.56264480959407,8.81597318478322,-17.9474144792473));
#40801=CARTESIAN_POINT('Ctrl Pts',(1.61072987577884,8.82169907113468,-17.9443337255254));
#40802=CARTESIAN_POINT('Ctrl Pts',(1.74016701018894,8.83711222079,-17.9360408403276));
#40803=CARTESIAN_POINT('Ctrl Pts',(1.87536541077607,8.8550562939364,-17.9263946075971));
#40804=CARTESIAN_POINT('Ctrl Pts',(2.01616865939584,8.87601506459434,-17.9151402743103));
#40805=CARTESIAN_POINT('Ctrl Pts',(2.02947228666054,8.87799532908038,-17.9140769220323));
#40806=CARTESIAN_POINT('Ctrl Pts',(2.04282591751082,8.88000252588665,-17.9129992048174));
#40807=CARTESIAN_POINT('Ctrl Pts',(2.05622939953854,8.88203707503234,-17.9119069022469));
#40808=CARTESIAN_POINT('Ctrl Pts',(2.18612622307218,8.90175444927892,-17.9013210982043));
#40809=CARTESIAN_POINT('Ctrl Pts',(2.32070785844954,8.92403976017556,-17.8893658762888));
#40810=CARTESIAN_POINT('Ctrl Pts',(2.45982125553463,8.94927553327455,-17.8758403317894));
#40811=CARTESIAN_POINT('Ctrl Pts',(2.57753274685146,8.97062890791897,-17.8643956251885));
#40812=CARTESIAN_POINT('Ctrl Pts',(2.69848834972096,8.99409519305475,-17.8518263861054));
#40813=CARTESIAN_POINT('Ctrl Pts',(2.82257920276446,9.01990720279287,-17.8380107025425));
#40814=CARTESIAN_POINT('Ctrl Pts',(2.92927450828348,9.04210078271857,-17.8261317562499));
#40815=CARTESIAN_POINT('Ctrl Pts',(3.0382873664991,9.06602868485195,-17.8133312539005));
#40816=CARTESIAN_POINT('Ctrl Pts',(3.149539801541,9.09183746377786,-17.7995327346023));
#40817=CARTESIAN_POINT('Ctrl Pts',(3.24642781372313,9.11431392720122,-17.787515819149));
#40818=CARTESIAN_POINT('Ctrl Pts',(3.34501424878886,9.13821698171628,-17.77474193929));
#40819=CARTESIAN_POINT('Ctrl Pts',(3.44524276091874,9.1636416709327,-17.7611617882135));
#40820=CARTESIAN_POINT('Ctrl Pts',(3.44871466880745,9.16452238019579,-17.7606913728332));
#40821=CARTESIAN_POINT('Ctrl Pts',(3.45218854645181,9.1654049152036,-17.7602199900659));
#40822=CARTESIAN_POINT('Ctrl Pts',(3.45566439144633,9.16628927984497,-17.7597476379063));
#40823=CARTESIAN_POINT('Ctrl Pts',(3.53373654223191,9.18615329844753,-17.7491379734686));
#40824=CARTESIAN_POINT('Ctrl Pts',(3.61280142985509,9.20694044006577,-17.7380392030405));
#40825=CARTESIAN_POINT('Ctrl Pts',(3.69283061359466,9.22869446064501,-17.7264288224018));
#40826=CARTESIAN_POINT('Ctrl Pts',(3.69949261699861,9.23050536702162,-17.725462320037));
#40827=CARTESIAN_POINT('Ctrl Pts',(3.70616130265311,9.23232297332201,-17.7244922725653));
#40828=CARTESIAN_POINT('Ctrl Pts',(3.71283665319058,9.23414730455173,-17.7235186671645));
#40829=CARTESIAN_POINT('Ctrl Pts',(3.74625606261466,9.24328061851759,-17.7186444186405));
#40830=CARTESIAN_POINT('Ctrl Pts',(3.77984252556761,9.25258248776584,-17.7136809929659));
#40831=CARTESIAN_POINT('Ctrl Pts',(3.81359387701825,9.26205601500284,-17.7086268127341));
#40832=CARTESIAN_POINT('Ctrl Pts',(3.83384037984567,9.26773892213829,-17.7055949497137));
#40833=CARTESIAN_POINT('Ctrl Pts',(3.85414621761188,9.27348360048981,-17.7025304286917));
#40834=CARTESIAN_POINT('Ctrl Pts',(3.8745109209936,9.27929071539973,-17.6994329122567));
#40835=CARTESIAN_POINT('Ctrl Pts',(3.88469327268447,9.2821942728547,-17.6978841540392));
#40836=CARTESIAN_POINT('Ctrl Pts',(3.89489034077921,9.28511343945291,-17.6963271469753));
#40837=CARTESIAN_POINT('Ctrl Pts',(3.90510206547525,9.2880482981763,-17.6947618490399));
#40838=CARTESIAN_POINT('Ctrl Pts',(3.91020792782327,9.289515727538,-17.6939792000721));
#40839=CARTESIAN_POINT('Ctrl Pts',(3.91531745432161,9.29098707993123,-17.6931944783869));
#40840=CARTESIAN_POINT('Ctrl Pts',(3.92043063744515,9.29246236570345,-17.6924076787479));
#40841=CARTESIAN_POINT('Ctrl Pts',(3.92554382056869,9.29393765147567,-17.6916208791089));
#40842=CARTESIAN_POINT('Ctrl Pts',(3.93242661853467,9.29592838500546,-17.6905592143405));
#40843=CARTESIAN_POINT('Ctrl Pts',(3.93578114914916,9.29690003349812,-17.6900410407387));
#40844=CARTESIAN_POINT('Ctrl Pts',(3.94207838550102,9.2987240443397,-17.6890683080328));
#40845=CARTESIAN_POINT('Ctrl Pts',(3.94835838647121,9.30054739878747,-17.6880959557532));
#40846=CARTESIAN_POINT('Ctrl Pts',(3.95462116944837,9.30237003113425,-17.6871240188475));
#40847=CARTESIAN_POINT('Ctrl Pts',(4.02983425200072,9.32425898971077,-17.6754515130318));
#40848=CARTESIAN_POINT('Ctrl Pts',(4.1025639945611,9.34604295765425,-17.6638393840448));
#40849=CARTESIAN_POINT('Ctrl Pts',(4.17284111891252,9.36761359660687,-17.6523453170107));
#40850=CARTESIAN_POINT('Ctrl Pts',(4.24076842735754,9.38846299047454,-17.6412355705048));
#40851=CARTESIAN_POINT('Ctrl Pts',(4.30640441838942,9.40911317057249,-17.6302360787778));
#40852=CARTESIAN_POINT('Ctrl Pts',(4.36977697048984,9.42947505700555,-17.6193942607279));
#40853=CARTESIAN_POINT('Ctrl Pts',(4.43122693487369,9.44921920734554,-17.6088813602538));
#40854=CARTESIAN_POINT('Ctrl Pts',(4.49054873063997,9.46869236090643,-17.5985166775392));
#40855=CARTESIAN_POINT('Ctrl Pts',(4.5477674454098,9.48782062019841,-17.5883395360635));
#40856=CARTESIAN_POINT('Ctrl Pts',(4.60352144780265,9.50645922504345,-17.578422913985));
#40857=CARTESIAN_POINT('Ctrl Pts',(4.65727867302525,9.52477042143705,-17.5686843289927));
#40858=CARTESIAN_POINT('Ctrl Pts',(4.70906171444353,9.54269206233632,-17.5591568289019));
#40859=CARTESIAN_POINT('Ctrl Pts',(4.75987978164253,9.56027973441181,-17.5498068732679));
#40860=CARTESIAN_POINT('Ctrl Pts',(4.8087965634695,9.57749227523871,-17.5406601907414));
#40861=CARTESIAN_POINT('Ctrl Pts',(4.85583261242937,9.59427637097178,-17.5317450928251));
#40862=CARTESIAN_POINT('Ctrl Pts',(4.90207267825761,9.61077643228066,-17.5229808636088));
#40863=CARTESIAN_POINT('Ctrl Pts',(4.94649513038224,9.6268624611947,-17.5144404326597));
#40864=CARTESIAN_POINT('Ctrl Pts',(4.98911858191001,9.6424885761226,-17.5061481039024));
#40865=CARTESIAN_POINT('Ctrl Pts',(4.98947832141365,9.64262045964274,-17.5060781171199));
#40866=CARTESIAN_POINT('Ctrl Pts',(4.98983793276467,9.64275231042812,-17.5060081479946));
#40867=CARTESIAN_POINT('Ctrl Pts',(4.99019741597397,9.64288412845248,-17.5059381965404));
#40868=CARTESIAN_POINT('Ctrl Pts',(5.03326309494624,9.65867577761138,-17.4975580920137));
#40869=CARTESIAN_POINT('Ctrl Pts',(5.07448979202937,9.67399688545065,-17.4894318230365));
#40870=CARTESIAN_POINT('Ctrl Pts',(5.1138956704581,9.68880469390431,-17.4815819379706));
#40871=CARTESIAN_POINT('Ctrl Pts',(5.15370025521237,9.70376232687992,-17.4736526282362));
#40872=CARTESIAN_POINT('Ctrl Pts',(5.19164699321678,9.71819623298685,-17.4660053223283));
#40873=CARTESIAN_POINT('Ctrl Pts',(5.22775340220523,9.73206688375502,-17.4586607148637));
#40874=CARTESIAN_POINT('Ctrl Pts',(5.26453906456748,9.74619847673802,-17.4511779366548));
#40875=CARTESIAN_POINT('Ctrl Pts',(5.29941451023093,9.75974542755134,-17.444009355409));
#40876=CARTESIAN_POINT('Ctrl Pts',(5.33239691037664,9.77267052382948,-17.4371742321374));
#40877=CARTESIAN_POINT('Ctrl Pts',(5.3664114649273,9.78600009931467,-17.4301252098602));
#40878=CARTESIAN_POINT('Ctrl Pts',(5.3984126497053,9.79866828470103,-17.4234308497413));
#40879=CARTESIAN_POINT('Ctrl Pts',(5.42841772935895,9.81063913570891,-17.4171094389117));
#40880=CARTESIAN_POINT('Ctrl Pts',(5.45996541482443,9.82322542598741,-17.410463034941));
#40881=CARTESIAN_POINT('Ctrl Pts',(5.48930650010712,9.83504080994725,-17.4042289291992));
#40882=CARTESIAN_POINT('Ctrl Pts',(5.51645909150323,9.84604910464715,-17.3984250783859));
#40883=CARTESIAN_POINT('Ctrl Pts',(5.54440583240798,9.8573793661052,-17.3924514785713));
#40884=CARTESIAN_POINT('Ctrl Pts',(5.57003422426587,9.86785462335406,-17.3869336679418));
#40885=CARTESIAN_POINT('Ctrl Pts',(5.59336166006701,9.87744149966146,-17.3818876748619));
#40886=CARTESIAN_POINT('Ctrl Pts',(-5.84637331455752,9.55547474172696,-17.3476041564549));
#40887=CARTESIAN_POINT('Ctrl Pts',(-5.81071185191775,9.54063160033165,-17.3552733651954));
#40888=CARTESIAN_POINT('Ctrl Pts',(-5.69191847149354,9.49167373167442,-17.3806024305499));
#40889=CARTESIAN_POINT('Ctrl Pts',(-5.48049361555364,9.40739237367748,-17.4243722057435));
#40890=CARTESIAN_POINT('Ctrl Pts',(-5.2021495036308,9.30184459029148,-17.479369066501));
#40891=CARTESIAN_POINT('Ctrl Pts',(-4.89414309097487,9.19156149103333,-17.536962878198));
#40892=CARTESIAN_POINT('Ctrl Pts',(-4.55276432929974,9.07723438519874,-17.5967675196366));
#40893=CARTESIAN_POINT('Ctrl Pts',(-4.17238112667691,8.95957671976703,-17.6583984118004));
#40894=CARTESIAN_POINT('Ctrl Pts',(-3.74657532026531,8.84000882077894,-17.721111142741));
#40895=CARTESIAN_POINT('Ctrl Pts',(-3.27004047448275,8.72141187442827,-17.7834030530746));
#40896=CARTESIAN_POINT('Ctrl Pts',(-2.73870586769555,8.60813163533864,-17.8430067909733));
#40897=CARTESIAN_POINT('Ctrl Pts',(-2.14779200690435,8.50556187107943,-17.897101921995));
#40898=CARTESIAN_POINT('Ctrl Pts',(-1.49669793916356,8.42117401415249,-17.9417588875659));
#40899=CARTESIAN_POINT('Ctrl Pts',(-0.805489886452122,8.36490960362597,
-17.971684220105));
#40900=CARTESIAN_POINT('Ctrl Pts',(-0.11337925692961,8.34312729743292,-17.9833787418543));
#40901=CARTESIAN_POINT('Ctrl Pts',(0.536146508488068,8.35364625772937,-17.977717202363));
#40902=CARTESIAN_POINT('Ctrl Pts',(1.11983353235545,8.38851236910003,-17.9591191164996));
#40903=CARTESIAN_POINT('Ctrl Pts',(1.63691904071335,8.4393404653141,-17.9321437229463));
#40904=CARTESIAN_POINT('Ctrl Pts',(2.09764269443844,8.50038183956579,-17.8998528831987));
#40905=CARTESIAN_POINT('Ctrl Pts',(2.51227845886102,8.56810417229776,-17.8641129073894));
#40906=CARTESIAN_POINT('Ctrl Pts',(2.88626565936715,8.63960400139166,-17.8264469425659));
#40907=CARTESIAN_POINT('Ctrl Pts',(3.2232840470072,8.71248864803032,-17.7881049412844));
#40908=CARTESIAN_POINT('Ctrl Pts',(3.52770199605896,8.78521869171782,-17.7498872415768));
#40909=CARTESIAN_POINT('Ctrl Pts',(3.80294640697365,8.85662163053349,-17.7124022350257));
#40910=CARTESIAN_POINT('Ctrl Pts',(4.05165902840887,8.92575523409715,-17.6761384257067));
#40911=CARTESIAN_POINT('Ctrl Pts',(4.27618401348504,8.99192944160887,-17.6414529589729));
#40912=CARTESIAN_POINT('Ctrl Pts',(4.47887700846266,9.05473894280456,-17.6085545575236));
#40913=CARTESIAN_POINT('Ctrl Pts',(4.66209438678431,9.11402294515649,-17.577524623232));
#40914=CARTESIAN_POINT('Ctrl Pts',(4.82815454959788,9.16981751996399,-17.5483421923328));
#40915=CARTESIAN_POINT('Ctrl Pts',(4.97929846125148,9.22230881982344,-17.5209084312054));
#40916=CARTESIAN_POINT('Ctrl Pts',(5.11759084189312,9.27176794816472,-17.4950807348835));
#40917=CARTESIAN_POINT('Ctrl Pts',(5.24463362120297,9.31841543321117,-17.4707435021366));
#40918=CARTESIAN_POINT('Ctrl Pts',(5.36151919418637,9.36236488162901,-17.4478372925747));
#40919=CARTESIAN_POINT('Ctrl Pts',(5.46894871897953,9.40363638206334,-17.4263514514219));
#40920=CARTESIAN_POINT('Ctrl Pts',(5.56756023616595,9.44226580283917,-17.406266900768));
#40921=CARTESIAN_POINT('Ctrl Pts',(5.6579973458819,9.47832606039999,-17.3875449759112));
#40922=CARTESIAN_POINT('Ctrl Pts',(5.74090606562001,9.51192223555312,-17.3701299000524));
#40923=CARTESIAN_POINT('Ctrl Pts',(5.80283958810511,9.53739134960786,-17.3569501787337));
#40924=CARTESIAN_POINT('Ctrl Pts',(5.83721149049653,9.55166218125863,-17.3495747889199));
#40925=CARTESIAN_POINT('Ctrl Pts',(5.8463475925958,9.55546502788484,-17.3476101108887));
#40926=CARTESIAN_POINT('Ctrl Pts',(-5.81214069693568,9.6776290300071,-17.4225528946938));
#40927=CARTESIAN_POINT('Ctrl Pts',(-5.77669403943401,9.66284974879393,-17.4302160824804));
#40928=CARTESIAN_POINT('Ctrl Pts',(-5.65860780706729,9.6140989355557,-17.4555273035572));
#40929=CARTESIAN_POINT('Ctrl Pts',(-5.44840103507682,9.53015694427974,-17.4992760054666));
#40930=CARTESIAN_POINT('Ctrl Pts',(-5.1716235662445,9.42501829450879,-17.5542570073678));
#40931=CARTESIAN_POINT('Ctrl Pts',(-4.86534001924691,9.31515643154803,-17.6118405916567));
#40932=CARTESIAN_POINT('Ctrl Pts',(-4.52587676502638,9.20126515974296,-17.6716387378284));
#40933=CARTESIAN_POINT('Ctrl Pts',(-4.14764618194598,9.08405852203899,-17.7332657288787));
#40934=CARTESIAN_POINT('Ctrl Pts',(-3.72427796798699,8.96495349815562,-17.7959764462078));
#40935=CARTESIAN_POINT('Ctrl Pts',(-3.25050693887968,8.8468213189703,-17.8582676328334));
#40936=CARTESIAN_POINT('Ctrl Pts',(-2.72229502793864,8.7339908807422,-17.9178712771889));
#40937=CARTESIAN_POINT('Ctrl Pts',(-2.13489630729917,8.63183353884197,-17.9719662105889));
#40938=CARTESIAN_POINT('Ctrl Pts',(-1.48771081717117,8.54778848442007,-18.0166222406388));
#40939=CARTESIAN_POINT('Ctrl Pts',(-0.800671855351995,8.49175380188948,
-18.0465458816406));
#40940=CARTESIAN_POINT('Ctrl Pts',(-0.112708541201747,8.47005970746182,
-18.0582390465695));
#40941=CARTESIAN_POINT('Ctrl Pts',(0.532949978621521,8.48053622101904,-18.0525782429442));
#40942=CARTESIAN_POINT('Ctrl Pts',(1.11311776538049,8.51526017793769,-18.0339815736975));
#40943=CARTESIAN_POINT('Ctrl Pts',(1.62709018905108,8.56588107546072,-18.0070072842141));
#40944=CARTESIAN_POINT('Ctrl Pts',(2.08504975370832,8.62667479118321,-17.9747170663004));
#40945=CARTESIAN_POINT('Ctrl Pts',(2.49721344229027,8.69412423447536,-17.9389773342653));
#40946=CARTESIAN_POINT('Ctrl Pts',(2.86898749461564,8.76533823308763,-17.9013114427223));
#40947=CARTESIAN_POINT('Ctrl Pts',(3.20402760911694,8.83793391897526,-17.8629695570604));
#40948=CARTESIAN_POINT('Ctrl Pts',(3.50667332561844,8.91037796332439,-17.8247521929843));
#40949=CARTESIAN_POINT('Ctrl Pts',(3.78032819766911,8.98150228244581,-17.7872678757862));
#40950=CARTESIAN_POINT('Ctrl Pts',(4.02761533238891,9.05036799932828,-17.7510052017049));
#40951=CARTESIAN_POINT('Ctrl Pts',(4.25086223368234,9.11628731866267,-17.7163213743395));
#40952=CARTESIAN_POINT('Ctrl Pts',(4.45240821357209,9.17885604156746,-17.6834251529964));
#40953=CARTESIAN_POINT('Ctrl Pts',(4.63459373937968,9.23791353477718,-17.6523979671745));
#40954=CARTESIAN_POINT('Ctrl Pts',(4.79972194542439,9.29349528775297,-17.6232188834924));
#40955=CARTESIAN_POINT('Ctrl Pts',(4.95001934007057,9.34578631988376,-17.5957891117641));
#40956=CARTESIAN_POINT('Ctrl Pts',(5.08753747324296,9.39505629485978,-17.5699661113688));
#40957=CARTESIAN_POINT('Ctrl Pts',(5.21386790054559,9.4415244999522,-17.5456343620477));
#40958=CARTESIAN_POINT('Ctrl Pts',(5.33009563895032,9.48530371309719,-17.5227345087097));
#40959=CARTESIAN_POINT('Ctrl Pts',(5.43691681896545,9.52641357738842,-17.5012559687883));
#40960=CARTESIAN_POINT('Ctrl Pts',(5.53496502099396,9.5648895099918,-17.4811797200827));
#40961=CARTESIAN_POINT('Ctrl Pts',(5.62487964845031,9.600803928118,-17.4624671215404));
#40962=CARTESIAN_POINT('Ctrl Pts',(5.70730293164213,9.63426144409487,-17.4450623578241));
#40963=CARTESIAN_POINT('Ctrl Pts',(5.76886861607727,9.65962318953327,-17.4318917174653));
#40964=CARTESIAN_POINT('Ctrl Pts',(5.80303452985547,9.67383305507474,-17.4245218566629));
#40965=CARTESIAN_POINT('Ctrl Pts',(5.81211577346237,9.67761960876587,-17.422558677682));
#40966=CARTESIAN_POINT('Ctrl Pts',(-5.75637685509934,9.8140410329922,-17.4252871788604));
#40967=CARTESIAN_POINT('Ctrl Pts',(-5.72124236127017,9.7993897878127,-17.4329279894493));
#40968=CARTESIAN_POINT('Ctrl Pts',(-5.60419107359204,9.75105931185798,-17.4581666988706));
#40969=CARTESIAN_POINT('Ctrl Pts',(-5.39580527606125,9.66783272587568,-17.5017964291619));
#40970=CARTESIAN_POINT('Ctrl Pts',(-5.12142095100228,9.56358874197378,-17.5566334095007));
#40971=CARTESIAN_POINT('Ctrl Pts',(-4.81781048341173,9.45467084686905,-17.6140674917309));
#40972=CARTESIAN_POINT('Ctrl Pts',(-4.48135661765004,9.34177398380753,-17.6737092386581));
#40973=CARTESIAN_POINT('Ctrl Pts',(-4.10654539124082,9.22561137506256,-17.7351721601088));
#40974=CARTESIAN_POINT('Ctrl Pts',(-3.68708984653772,9.10759142874642,-17.7977117189014));
#40975=CARTESIAN_POINT('Ctrl Pts',(-3.2178010218237,8.99056153156208,-17.8598276396926));
#40976=CARTESIAN_POINT('Ctrl Pts',(-2.69470548472169,8.87880960914205,-17.9192576327495));
#40977=CARTESIAN_POINT('Ctrl Pts',(-2.11312431732625,8.77765127324428,-17.9731888284785));
#40978=CARTESIAN_POINT('Ctrl Pts',(-1.47247131244265,8.69444440361395,-18.0177040810838));
#40979=CARTESIAN_POINT('Ctrl Pts',(-0.79246216940496,8.63897622205117,-18.0475294251907));
#40980=CARTESIAN_POINT('Ctrl Pts',(-0.111558320839529,8.61750183103525,
-18.059182549587));
#40981=CARTESIAN_POINT('Ctrl Pts',(0.52749191852145,8.6278723666929,-18.0535412908526));
#40982=CARTESIAN_POINT('Ctrl Pts',(1.10170577775085,8.66224461984375,-18.0350066389497));
#40983=CARTESIAN_POINT('Ctrl Pts',(1.61044334327689,8.71235628289372,-18.0081195170544));
#40984=CARTESIAN_POINT('Ctrl Pts',(2.06378679093631,8.77254508682486,-17.9759306394822));
#40985=CARTESIAN_POINT('Ctrl Pts',(2.4718495657996,8.83933224481332,-17.9402999855696));
#40986=CARTESIAN_POINT('Ctrl Pts',(2.83997682955784,8.90985712180265,-17.9027460783165));
#40987=CARTESIAN_POINT('Ctrl Pts',(3.17177856607899,8.98176081272291,-17.8645154707668));
#40988=CARTESIAN_POINT('Ctrl Pts',(3.47154177309266,9.05352460016479,-17.8264066164218));
#40989=CARTESIAN_POINT('Ctrl Pts',(3.74262739560875,9.12399074783355,-17.7890266501162));
#40990=CARTESIAN_POINT('Ctrl Pts',(3.98762439282825,9.19222800962803,-17.7528631841345));
#40991=CARTESIAN_POINT('Ctrl Pts',(4.20883005547312,9.25755353604305,-17.7182728316013));
#40992=CARTESIAN_POINT('Ctrl Pts',(4.40855467300355,9.3195653228394,-17.6854641626409));
#40993=CARTESIAN_POINT('Ctrl Pts',(4.58911102375203,9.37810272990502,-17.6545187345435));
#40994=CARTESIAN_POINT('Ctrl Pts',(4.7527761669793,9.43319958665139,-17.6254159783337));
#40995=CARTESIAN_POINT('Ctrl Pts',(4.90175235812833,9.48503807969688,-17.598057636747));
#40996=CARTESIAN_POINT('Ctrl Pts',(5.03806939881879,9.53388445863904,-17.5723017856496));
#40997=CARTESIAN_POINT('Ctrl Pts',(5.16330186304976,9.57995516360071,-17.5480334301608));
#40998=CARTESIAN_POINT('Ctrl Pts',(5.27852271290777,9.62336113040067,-17.5251935807664));
#40999=CARTESIAN_POINT('Ctrl Pts',(5.38441979560827,9.66412103109555,-17.5037718754277));
#41000=CARTESIAN_POINT('Ctrl Pts',(5.48161934164266,9.70226927265982,-17.4837495046991));
#41001=CARTESIAN_POINT('Ctrl Pts',(5.57075379922798,9.73787708217004,-17.4650880447167));
#41002=CARTESIAN_POINT('Ctrl Pts',(5.65245896154948,9.7710477993865,-17.4477318689615));
#41003=CARTESIAN_POINT('Ctrl Pts',(5.71348552357779,9.796191046643,-17.434598822889));
#41004=CARTESIAN_POINT('Ctrl Pts',(5.74735130046084,9.81027810305254,-17.4272502808467));
#41005=CARTESIAN_POINT('Ctrl Pts',(5.75635272233611,9.8140319128402,-17.4252927958575));
#41006=CARTESIAN_POINT('Ctrl Pts',(-5.69417743957803,9.92771327144431,-17.3549336348315));
#41007=CARTESIAN_POINT('Ctrl Pts',(-5.65936792101113,9.91321960471387,-17.3625417556048));
#41008=CARTESIAN_POINT('Ctrl Pts',(-5.54339907756701,9.86540905243201,-17.3876728669242));
#41009=CARTESIAN_POINT('Ctrl Pts',(-5.33694401269858,9.78308042667019,-17.4311178392296));
#41010=CARTESIAN_POINT('Ctrl Pts',(-5.06513131455385,9.67997470341483,-17.4857214910404));
#41011=CARTESIAN_POINT('Ctrl Pts',(-4.76442037050557,9.57226825687109,-17.5429071195401));
#41012=CARTESIAN_POINT('Ctrl Pts',(-4.43125498855782,9.46065550148003,-17.6022847388691));
#41013=CARTESIAN_POINT('Ctrl Pts',(-4.06020411559034,9.34584764235814,-17.663467660997));
#41014=CARTESIAN_POINT('Ctrl Pts',(-3.64507706599585,9.22924160764453,-17.7257130627828));
#41015=CARTESIAN_POINT('Ctrl Pts',(-3.18077544795952,9.11365349726097,-17.7875264269979));
#41016=CARTESIAN_POINT('Ctrl Pts',(-2.66340495859278,9.00331722991946,-17.8466560259837));
#41017=CARTESIAN_POINT('Ctrl Pts',(-2.08836900848276,8.90347441105333,-17.9003040865354));
#41018=CARTESIAN_POINT('Ctrl Pts',(-1.45510419309184,8.82137451837695,-17.9445766737933));
#41019=CARTESIAN_POINT('Ctrl Pts',(-0.783082843198929,8.76665646966238,
-17.9742336186812));
#41020=CARTESIAN_POINT('Ctrl Pts',(-0.110239903977575,8.7454738833116,-17.9858188158545));
#41021=CARTESIAN_POINT('Ctrl Pts',(0.521249582007313,8.75570355774493,-17.9802106405749));
#41022=CARTESIAN_POINT('Ctrl Pts',(1.08868634505104,8.78960963235603,-17.9617818848648));
#41023=CARTESIAN_POINT('Ctrl Pts',(1.59148420789597,8.83904768676422,-17.935044492473));
#41024=CARTESIAN_POINT('Ctrl Pts',(2.03960899817982,8.89843785453517,-17.9030303521735));
#41025=CARTESIAN_POINT('Ctrl Pts',(2.44305208407453,8.96435237350228,-17.8675882038322));
#41026=CARTESIAN_POINT('Ctrl Pts',(2.80708608283326,9.03397113821115,-17.8302280017904));
#41027=CARTESIAN_POINT('Ctrl Pts',(3.13526596976642,9.10496688075775,-17.7921898350716));
#41028=CARTESIAN_POINT('Ctrl Pts',(3.43181671015123,9.1758400646716,-17.7542684107075));
#41029=CARTESIAN_POINT('Ctrl Pts',(3.70004890813467,9.24544643262587,-17.7170683235269));
#41030=CARTESIAN_POINT('Ctrl Pts',(3.94251110847289,9.31286458365095,-17.6810753908391));
#41031=CARTESIAN_POINT('Ctrl Pts',(4.16146500019945,9.37741795690274,-17.646645145667));
#41032=CARTESIAN_POINT('Ctrl Pts',(4.35918701579828,9.43870723235016,-17.6139857940658));
#41033=CARTESIAN_POINT('Ctrl Pts',(4.53795795535941,9.49657159849751,-17.5831790868076));
#41034=CARTESIAN_POINT('Ctrl Pts',(4.70002505220228,9.55104259508925,-17.554205055054));
#41035=CARTESIAN_POINT('Ctrl Pts',(4.84756307655687,9.60229864215115,-17.5269663201844));
#41036=CARTESIAN_POINT('Ctrl Pts',(4.98257739074038,9.65060152385877,-17.501321960375));
#41037=CARTESIAN_POINT('Ctrl Pts',(5.10662357656201,9.69616399681796,-17.4771578087562));
#41038=CARTESIAN_POINT('Ctrl Pts',(5.22076112767138,9.7390946394701,-17.4544154229623));
#41039=CARTESIAN_POINT('Ctrl Pts',(5.32566859456254,9.77941088992731,-17.4330847501919));
#41040=CARTESIAN_POINT('Ctrl Pts',(5.42196395766287,9.81714585911028,-17.413147293363));
#41041=CARTESIAN_POINT('Ctrl Pts',(5.51027183420198,9.85236921482051,-17.3945649807498));
#41042=CARTESIAN_POINT('Ctrl Pts',(5.59122067258088,9.88518256407872,-17.3772825511604));
#41043=CARTESIAN_POINT('Ctrl Pts',(5.65168283897655,9.91005528387838,-17.3642054611152));
#41044=CARTESIAN_POINT('Ctrl Pts',(5.68523561929143,9.92399090717374,-17.3568882701779));
#41045=CARTESIAN_POINT('Ctrl Pts',(5.69415387512849,9.92770437916783,-17.3549391363549));
#41046=CARTESIAN_POINT('',(5.73644274980887,9.52121898128059,-17.3763264188351));
#41047=CARTESIAN_POINT('Origin',(5.599999999773,9.67863108544398,-17.0348569101664));
#41048=CARTESIAN_POINT('Ctrl Pts',(-5.73644387793582,9.52121721533315,-17.3763301032669));
#41049=CARTESIAN_POINT('Ctrl Pts',(-5.66411038342567,9.49169730160193,-17.3916242104899));
#41050=CARTESIAN_POINT('Ctrl Pts',(-5.58548129177106,9.46019526663674,-17.4079767022565));
#41051=CARTESIAN_POINT('Ctrl Pts',(-5.50055660135251,9.42702545331558,-17.4252224540635));
#41052=CARTESIAN_POINT('Ctrl Pts',(-5.41741954877212,9.39455385406014,-17.4421051882566));
#41053=CARTESIAN_POINT('Ctrl Pts',(-5.32824914863658,9.36048411499632,-17.4598438857157));
#41054=CARTESIAN_POINT('Ctrl Pts',(-5.23304539942654,9.32515773129678,-17.4782590784543));
#41055=CARTESIAN_POINT('Ctrl Pts',(-5.1347710008645,9.28869194985171,-17.4972682246886));
#41056=CARTESIAN_POINT('Ctrl Pts',(-5.03006778418147,9.25088688316903,-17.516998351475));
#41057=CARTESIAN_POINT('Ctrl Pts',(-4.91893574770631,9.21216969728679,-17.5372248895517));
#41058=CARTESIAN_POINT('Ctrl Pts',(-4.80780371123115,9.17345251140456,-17.5574514276284));
#41059=CARTESIAN_POINT('Ctrl Pts',(-4.69024285496385,9.13382320291011,-17.5781743787171));
#41060=CARTESIAN_POINT('Ctrl Pts',(-4.56625317723326,9.09376135229856,-17.5991415486935));
#41061=CARTESIAN_POINT('Ctrl Pts',(-4.44622761409869,9.05498033223404,-17.6194383704113));
#41062=CARTESIAN_POINT('Ctrl Pts',(-4.32017773615893,9.01579424100516,-17.6399639103149));
#41063=CARTESIAN_POINT('Ctrl Pts',(-4.18810354341397,8.97668495174031,-17.6604647153228));
#41064=CARTESIAN_POINT('Ctrl Pts',(-4.05161767055035,8.93626929315137,-17.6816503096298));
#41065=CARTESIAN_POINT('Ctrl Pts',(-3.90869830026241,8.89593536972225,-17.7028096379926));
#41066=CARTESIAN_POINT('Ctrl Pts',(-3.75934543255017,8.85626673446492,-17.7236357165823));
#41067=CARTESIAN_POINT('Ctrl Pts',(-3.60999256483792,8.81659809920759,-17.7444617951721));
#41068=CARTESIAN_POINT('Ctrl Pts',(-3.45420619970136,8.77759474677075,-17.7649546263512));
#41069=CARTESIAN_POINT('Ctrl Pts',(-3.29198633714049,8.73989291609286,-17.7847794700339));
#41070=CARTESIAN_POINT('Ctrl Pts',(-3.21175032065614,8.72124510897475,-17.7945850909943));
#41071=CARTESIAN_POINT('Ctrl Pts',(-3.1299404019154,8.70291652036431,-17.8042268665942));
#41072=CARTESIAN_POINT('Ctrl Pts',(-3.04655658560425,8.68498892402543,-17.8136617872421));
#41073=CARTESIAN_POINT('Ctrl Pts',(-3.00486467744867,8.67602512585599,-17.8183792475661));
#41074=CARTESIAN_POINT('Ctrl Pts',(-2.96277928617363,8.66716159628124,-17.8230449549843));
#41075=CARTESIAN_POINT('Ctrl Pts',(-2.92030042303628,8.65840888808932,-17.8276533930247));
#41076=CARTESIAN_POINT('Ctrl Pts',(-2.89906099146761,8.65403253399335,-17.8299576120449));
#41077=CARTESIAN_POINT('Ctrl Pts',(-2.87772319136642,8.64968388651658,-17.8322475112797));
#41078=CARTESIAN_POINT('Ctrl Pts',(-2.85628702258498,8.64536427823138,-17.8345223891241));
#41079=CARTESIAN_POINT('Ctrl Pts',(-2.84556893819426,8.64320447408879,-17.8356598280463));
#41080=CARTESIAN_POINT('Ctrl Pts',(-2.83482626160102,8.64105192982512,-17.836793511467));
#41081=CARTESIAN_POINT('Ctrl Pts',(-2.82405899279638,8.63890681319801,-17.8379233510875));
#41082=CARTESIAN_POINT('Ctrl Pts',(-2.81867535839406,8.63783425488446,-17.8384882708978));
#41083=CARTESIAN_POINT('Ctrl Pts',(-2.81328557593688,8.63676355348512,-17.8390522297484));
#41084=CARTESIAN_POINT('Ctrl Pts',(-2.80788964542488,8.63569473004595,-17.8396152165656));
#41085=CARTESIAN_POINT('Ctrl Pts',(-2.80249371491288,8.63462590660678,-17.8401782033829));
#41086=CARTESIAN_POINT('Ctrl Pts',(-2.79531868547233,8.63320981247684,-17.8409241382583));
#41087=CARTESIAN_POINT('Ctrl Pts',(-2.79168340972041,8.63249391468896,-17.8413012498115));
#41088=CARTESIAN_POINT('Ctrl Pts',(-2.04588093613951,8.48562243162411,-17.9186683461067));
#41089=CARTESIAN_POINT('Ctrl Pts',(-1.30009078784875,8.39776408503863,-17.9651455234455));
#41090=CARTESIAN_POINT('Ctrl Pts',(-0.554283333978138,8.36894043965146,
-17.9807044955084));
#41091=CARTESIAN_POINT('Ctrl Pts',(-0.369523434874257,8.36179991861496,
-17.9845589409065));
#41092=CARTESIAN_POINT('Ctrl Pts',(-0.184762473712586,8.35828264718359,
-17.986515842323));
#41093=CARTESIAN_POINT('Ctrl Pts',(-7.99360577730113E-13,8.35838942830133,
-17.9865746369497));
#41094=CARTESIAN_POINT('Ctrl Pts',(6.94550121454233E-5,8.35838946844197,
-17.9865746590515));
#41095=CARTESIAN_POINT('Ctrl Pts',(0.000138910025304622,8.35838950909474,
-17.9865746808851));
#41096=CARTESIAN_POINT('Ctrl Pts',(0.000208365038677248,8.35838955025963,
-17.9865747024504));
#41097=CARTESIAN_POINT('Ctrl Pts',(0.465533255570969,8.35866534097634,-17.9867191828595));
#41098=CARTESIAN_POINT('Ctrl Pts',(0.930858145081447,8.38166463295442,-17.9746778676881));
#41099=CARTESIAN_POINT('Ctrl Pts',(1.39618303357009,8.42737850509597,-17.9504583227467));
#41100=CARTESIAN_POINT('Ctrl Pts',(1.62884547781441,8.45023544116675,-17.9383485502759));
#41101=CARTESIAN_POINT('Ctrl Pts',(1.86150792191003,8.47877067136745,-17.9231942685957));
#41102=CARTESIAN_POINT('Ctrl Pts',(2.09417036449486,8.51298095415368,-17.9049967252316));
#41103=CARTESIAN_POINT('Ctrl Pts',(2.21050158578728,8.5300860955468,-17.8958979535495));
#41104=CARTESIAN_POINT('Ctrl Pts',(2.32683280861868,8.5486099938875,-17.8860383780086));
#41105=CARTESIAN_POINT('Ctrl Pts',(2.44316403066954,8.56855209163748,-17.8754181650244));
#41106=CARTESIAN_POINT('Ctrl Pts',(2.50132964169498,8.57852314051247,-17.8701080585323));
#41107=CARTESIAN_POINT('Ctrl Pts',(2.55949525262821,8.58884873884022,-17.8646077934184));
#41108=CARTESIAN_POINT('Ctrl Pts',(2.61766086348722,8.5995288113506,-17.8589173932483));
#41109=CARTESIAN_POINT('Ctrl Pts',(2.64674366891673,8.60486884760579,-17.8560721931632));
#41110=CARTESIAN_POINT('Ctrl Pts',(2.67582647433671,8.61029750238258,-17.8531794593596));
#41111=CARTESIAN_POINT('Ctrl Pts',(2.7049092797489,8.61581476573433,-17.8502391948578));
#41112=CARTESIAN_POINT('Ctrl Pts',(2.73217440982283,8.62098720012659,-17.8474826968874));
#41113=CARTESIAN_POINT('Ctrl Pts',(2.75943953989021,8.62623751314833,-17.8446844238911));
#41114=CARTESIAN_POINT('Ctrl Pts',(2.78670466995733,8.63156569635524,-17.8418443784168));
#41115=CARTESIAN_POINT('Ctrl Pts',(2.78852234529513,8.63192090856904,-17.8416550420518));
#41116=CARTESIAN_POINT('Ctrl Pts',(2.79172234575743,8.63254712883725,-17.8413212491149));
#41117=CARTESIAN_POINT('Ctrl Pts',(2.7921576959705,8.63263237126126,-17.8412758123555));
#41118=CARTESIAN_POINT('Ctrl Pts',(2.80635105401264,8.63541145855232,-17.839794475779));
#41119=CARTESIAN_POINT('Ctrl Pts',(2.82656971290414,8.63939945105124,-17.8376812591674));
#41120=CARTESIAN_POINT('Ctrl Pts',(2.85281367264499,8.64467374260481,-17.8348954844623));
#41121=CARTESIAN_POINT('Ctrl Pts',(2.87905792637246,8.64994809324134,-17.8321096785508));
#41122=CARTESIAN_POINT('Ctrl Pts',(2.9113276159417,8.65650877173247,-17.8286512992758));
#41123=CARTESIAN_POINT('Ctrl Pts',(2.9496227413527,8.66447932329167,-17.8244554218755));
#41124=CARTESIAN_POINT('Ctrl Pts',(2.9879183200816,8.67244996920214,-17.8202594948066));
#41125=CARTESIAN_POINT('Ctrl Pts',(3.03223947730509,8.68183052149572,-17.8153260518509));
#41126=CARTESIAN_POINT('Ctrl Pts',(3.08258621302318,8.69279067999899,-17.8095659239372));
#41127=CARTESIAN_POINT('Ctrl Pts',(3.13293393523487,8.70375105325554,-17.8038056831596));
#41128=CARTESIAN_POINT('Ctrl Pts',(3.18930747207375,8.7162910944596,-17.7972187246566));
#41129=CARTESIAN_POINT('Ctrl Pts',(3.25170682353982,8.7306266669751,-17.7896916363006));
#41130=CARTESIAN_POINT('Ctrl Pts',(3.31410687991243,8.7449624014352,-17.7821644629133));
#41131=CARTESIAN_POINT('Ctrl Pts',(3.3825328870566,8.76109370763203,-17.7736971379277));
#41132=CARTESIAN_POINT('Ctrl Pts',(3.45698484497233,8.77928261259938,-17.7641520138671));
#41133=CARTESIAN_POINT('Ctrl Pts',(3.53143822129211,8.79747186408838,-17.7546067079598));
#41134=CARTESIAN_POINT('Ctrl Pts',(3.61191777798963,8.81771879250422,-17.7439835613382));
#41135=CARTESIAN_POINT('Ctrl Pts',(3.69842351506488,8.84033160069405,-17.7321206943966));
#41136=CARTESIAN_POINT('Ctrl Pts',(3.77372180500989,8.86001475518896,-17.7217947481097));
#41137=CARTESIAN_POINT('Ctrl Pts',(3.85358595433381,8.88149117333469,-17.7105291312976));
#41138=CARTESIAN_POINT('Ctrl Pts',(3.93801596303663,8.90499259034002,-17.6982021477661));
#41139=CARTESIAN_POINT('Ctrl Pts',(3.98561503901163,8.91824197584575,-17.6912525686452));
#41140=CARTESIAN_POINT('Ctrl Pts',(4.0346653103836,8.93213545810003,-17.683965397655));
#41141=CARTESIAN_POINT('Ctrl Pts',(4.08516678273887,8.94671828866847,-17.6763168873926));
#41142=CARTESIAN_POINT('Ctrl Pts',(4.11041751891651,8.95400970395269,-17.6724926322615));
#41143=CARTESIAN_POINT('Ctrl Pts',(4.13603104579127,8.96147347239214,-17.6685780102973));
#41144=CARTESIAN_POINT('Ctrl Pts',(4.16200737546585,8.96911553234021,-17.6645699336875));
#41145=CARTESIAN_POINT('Ctrl Pts',(4.17499554030314,8.97293656231424,-17.6625658953826));
#41146=CARTESIAN_POINT('Ctrl Pts',(4.18807440525279,8.97680216617658,-17.6605384914099));
#41147=CARTESIAN_POINT('Ctrl Pts',(4.20124397016567,8.98071309740182,-17.6584873257955));
#41148=CARTESIAN_POINT('Ctrl Pts',(4.2078287526221,8.98266856301444,-17.6574617429884));
#41149=CARTESIAN_POINT('Ctrl Pts',(4.21443621003134,8.98463536053006,-17.6564302196462));
#41150=CARTESIAN_POINT('Ctrl Pts',(4.22106634239483,8.98661358516831,-17.6553927057802));
#41151=CARTESIAN_POINT('Ctrl Pts',(4.22769647475832,8.98859180980657,-17.6543551919142));
#41152=CARTESIAN_POINT('Ctrl Pts',(4.23593799439455,8.99105772534333,-17.65306190396));
#41153=CARTESIAN_POINT('Ctrl Pts',(4.24102476427196,8.99258263611854,-17.6522621422006));
#41154=CARTESIAN_POINT('Ctrl Pts',(4.37039571957259,9.03136543315713,-17.6319219370575));
#41155=CARTESIAN_POINT('Ctrl Pts',(4.49374081874749,9.070127787373,-17.6116087574268));
#41156=CARTESIAN_POINT('Ctrl Pts',(4.61106006309524,9.1083980751459,-17.5915706671761));
#41157=CARTESIAN_POINT('Ctrl Pts',(4.72934316492,9.14698277939176,-17.5713679503697));
#41158=CARTESIAN_POINT('Ctrl Pts',(4.84150099218696,9.185067237906,-17.5514448938586));
#41159=CARTESIAN_POINT('Ctrl Pts',(4.94753354622695,9.22221554440591,-17.5320307290879));
#41160=CARTESIAN_POINT('Ctrl Pts',(5.05275887907135,9.25908104247346,-17.5127643635043));
#41161=CARTESIAN_POINT('Ctrl Pts',(5.15195184655995,9.2950246503136,-17.4939991381214));
#41162=CARTESIAN_POINT('Ctrl Pts',(5.24511244999343,9.32966666640695,-17.4759346754223));
#41163=CARTESIAN_POINT('Ctrl Pts',(5.33934505593314,9.3647073094596,-17.4576623442834));
#41164=CARTESIAN_POINT('Ctrl Pts',(5.42740566978876,9.39841614503533,-17.4401070426611));
#41165=CARTESIAN_POINT('Ctrl Pts',(5.50929429290636,9.4304482037099,-17.4234500711274));
#41166=CARTESIAN_POINT('Ctrl Pts',(5.59118291602396,9.46248026238448,-17.4067930995937));
#41167=CARTESIAN_POINT('Ctrl Pts',(5.66689954840355,9.49283554612634,-17.3910344570249));
#41168=CARTESIAN_POINT('Ctrl Pts',(5.73644419139122,9.5212173172705,-17.3763300250116));
#41169=CARTESIAN_POINT('Origin',(5.6,9.67863108576213,-17.0348569102136));
#41170=CARTESIAN_POINT('Origin',(5.599974278086,9.67865015409865,-17.0348418886545));
#41171=CARTESIAN_POINT('Ctrl Pts',(5.71192057974457,3.68828900101138,-9.85023514350112));
#41172=CARTESIAN_POINT('Ctrl Pts',(5.71687909013046,3.68927746603566,-9.84789209427039));
#41173=CARTESIAN_POINT('Ctrl Pts',(5.76414655581842,3.69951923241957,-9.82520668560991));
#41174=CARTESIAN_POINT('Ctrl Pts',(5.84911010038005,3.73283091286591,-9.77805626709572));
#41175=CARTESIAN_POINT('Ctrl Pts',(5.94752938889343,3.81065413233525,-9.7065237214035));
#41176=CARTESIAN_POINT('Ctrl Pts',(6.01566971792523,3.90954242904105,-9.63753575219431));
#41177=CARTESIAN_POINT('Ctrl Pts',(6.04716489751294,4.00788517584066,-9.58296136794285));
#41178=CARTESIAN_POINT('Ctrl Pts',(6.05142143229536,4.0698892375096,-9.55471543074864));
#41179=CARTESIAN_POINT('Ctrl Pts',(6.0507700358332,4.09458285042653,-9.54441628184707));
#41180=CARTESIAN_POINT('Ctrl Pts',(5.59583289853465,3.61242448643793,-9.5665423944353));
#41181=CARTESIAN_POINT('Ctrl Pts',(5.60045925819736,3.61331789904416,-9.56436069032235));
#41182=CARTESIAN_POINT('Ctrl Pts',(5.64456722873301,3.62258540256811,-9.54323612999687));
#41183=CARTESIAN_POINT('Ctrl Pts',(5.7239592089636,3.65291740087055,-9.49930946581784));
#41184=CARTESIAN_POINT('Ctrl Pts',(5.81592915863889,3.72404613777338,-9.43278546471175));
#41185=CARTESIAN_POINT('Ctrl Pts',(5.87945135471979,3.81436258040131,-9.36894609262212));
#41186=CARTESIAN_POINT('Ctrl Pts',(5.90864330625533,3.90380035745063,-9.31890905716097));
#41187=CARTESIAN_POINT('Ctrl Pts',(5.91254704364485,3.95980194151539,-9.29334384463089));
#41188=CARTESIAN_POINT('Ctrl Pts',(5.91194908378594,3.98202534295877,-9.28408410725217));
#41189=CARTESIAN_POINT('Ctrl Pts',(5.5786770225829,3.33840156455887,-9.41055857489166));
#41190=CARTESIAN_POINT('Ctrl Pts',(5.58525591743157,3.33967221246092,-9.40750014613255));
#41191=CARTESIAN_POINT('Ctrl Pts',(5.64791910753711,3.35283604660006,-9.3779306843833));
#41192=CARTESIAN_POINT('Ctrl Pts',(5.75974886295832,3.39554420108066,-9.3172095505129));
#41193=CARTESIAN_POINT('Ctrl Pts',(5.88925468160274,3.49511101909614,-9.22577859145062));
#41194=CARTESIAN_POINT('Ctrl Pts',(5.98006530410807,3.6228200472589,-9.13695179587132));
#41195=CARTESIAN_POINT('Ctrl Pts',(6.02330455844228,3.75272356690769,-9.06502589944593));
#41196=CARTESIAN_POINT('Ctrl Pts',(6.02945981529473,3.83732356858628,-9.02648321068592));
#41197=CARTESIAN_POINT('Ctrl Pts',(6.02852200235225,3.871565851545,-9.01219518727837));
#41198=CARTESIAN_POINT('Ctrl Pts',(5.67169867046695,3.04584531044098,-9.48453249266367));
#41199=CARTESIAN_POINT('Ctrl Pts',(5.68123487669659,3.04771819915123,-9.48013397279952));
#41200=CARTESIAN_POINT('Ctrl Pts',(5.77200483704837,3.06709486655197,-9.43764959196145));
#41201=CARTESIAN_POINT('Ctrl Pts',(5.9330183650432,3.12942229883713,-9.35112473670729));
#41202=CARTESIAN_POINT('Ctrl Pts',(6.11944005804963,3.27391826346144,-9.22119812121329));
#41203=CARTESIAN_POINT('Ctrl Pts',(6.2515577828283,3.46047303546363,-9.09362743190567));
#41204=CARTESIAN_POINT('Ctrl Pts',(6.31598669919579,3.65368723849839,-8.98773487091865));
#41205=CARTESIAN_POINT('Ctrl Pts',(6.32552189499299,3.78273995333454,-8.92906339352892));
#41206=CARTESIAN_POINT('Ctrl Pts',(6.32407371695654,3.83561169243889,-8.90697548725414));
#41207=CARTESIAN_POINT('',(5.99998739574839,3.99788653423051,-9.34660672477245));
#41208=CARTESIAN_POINT('',(5.99999998791461,3.21424323425742,-9.29218306971572));
#41209=CARTESIAN_POINT('Ctrl Pts',(5.9999873957484,3.99788653423051,-9.34660672477246));
#41210=CARTESIAN_POINT('Ctrl Pts',(5.9999852507043,3.97568044757288,-9.33733089968698));
#41211=CARTESIAN_POINT('Ctrl Pts',(5.99998676083559,3.95337029535213,-9.328534099322));
#41212=CARTESIAN_POINT('Ctrl Pts',(5.99999979818264,3.93100830776541,-9.32032006028138));
#41213=CARTESIAN_POINT('Ctrl Pts',(6.00000674470619,3.91909345477917,-9.31594347849442));
#41214=CARTESIAN_POINT('Ctrl Pts',(6.00001622835211,3.90716442776862,-9.31173201822555));
#41215=CARTESIAN_POINT('Ctrl Pts',(6.00002591441227,3.89523282137244,-9.30769827794002));
#41216=CARTESIAN_POINT('Ctrl Pts',(6.00004505393926,3.87165612468503,-9.29972766039951));
#41217=CARTESIAN_POINT('Ctrl Pts',(6.00006657100939,3.84806757203079,-9.29245336782808));
#41218=CARTESIAN_POINT('Ctrl Pts',(6.00008776123526,3.82457051194069,-9.28593625304491));
#41219=CARTESIAN_POINT('Ctrl Pts',(6.00010095762279,3.8099375244107,-9.28187766618392));
#41220=CARTESIAN_POINT('Ctrl Pts',(6.00011344209019,3.79534069376842,-9.27811196626277));
#41221=CARTESIAN_POINT('Ctrl Pts',(6.00012222415269,3.78081005016456,-9.2746453820103));
#41222=CARTESIAN_POINT('Ctrl Pts',(6.0001366712745,3.75690610068274,-9.26894260262181));
#41223=CARTESIAN_POINT('Ctrl Pts',(6.00013999171371,3.73318089327534,-9.26405207526274));
#41224=CARTESIAN_POINT('Ctrl Pts',(6.00012429846304,3.70978124469432,-9.25996126528744));
#41225=CARTESIAN_POINT('Ctrl Pts',(6.00011929433188,3.70231976249024,-9.25865682237133));
#41226=CARTESIAN_POINT('Ctrl Pts',(6.0001124687567,3.69489145750722,-9.25743331593505));
#41227=CARTESIAN_POINT('Ctrl Pts',(6.00010395164358,3.68750121638747,-9.25628930568157));
#41228=CARTESIAN_POINT('Ctrl Pts',(6.00009904587385,3.68324451336532,-9.25563036751914));
#41229=CARTESIAN_POINT('Ctrl Pts',(6.00009358391438,3.6790004383084,-9.25499779435146));
#41230=CARTESIAN_POINT('Ctrl Pts',(6.00008768224772,3.67476986072246,-9.25439125254406));
#41231=CARTESIAN_POINT('Ctrl Pts',(6.00006914321531,3.66148025634672,-9.252485909717));
#41232=CARTESIAN_POINT('Ctrl Pts',(6.00005143457785,3.64814284857007,-9.25080653782235));
#41233=CARTESIAN_POINT('Ctrl Pts',(6.00003088539827,3.63498884507945,-9.24938653464367));
#41234=CARTESIAN_POINT('Ctrl Pts',(6.00001015026417,3.62171580780848,-9.24795368151047));
#41235=CARTESIAN_POINT('Ctrl Pts',(5.99998607093735,3.60863002122327,-9.24678503799945));
#41236=CARTESIAN_POINT('Ctrl Pts',(5.99996799233405,3.59598531542618,-9.24586523586959));
#41237=CARTESIAN_POINT('Ctrl Pts',(5.99995732843904,3.58852667423793,-9.24532267883735));
#41238=CARTESIAN_POINT('Ctrl Pts',(5.99994904811738,3.58122177219781,-9.24486573182062));
#41239=CARTESIAN_POINT('Ctrl Pts',(5.99994795245078,3.57412414233203,-9.24448341761151));
#41240=CARTESIAN_POINT('Ctrl Pts',(5.99994403955748,3.54877677088038,-9.24311808010406));
#41241=CARTESIAN_POINT('Ctrl Pts',(5.99996395296392,3.52334629616488,-9.24263149392783));
#41242=CARTESIAN_POINT('Ctrl Pts',(5.99998991135032,3.4979788568905,-9.24309866573729));
#41243=CARTESIAN_POINT('Ctrl Pts',(6.00001572107996,3.47275669017528,-9.2435631621784));
#41244=CARTESIAN_POINT('Ctrl Pts',(6.0000467896797,3.44759768203729,-9.24497095300123));
#41245=CARTESIAN_POINT('Ctrl Pts',(6.00006724836824,3.42266827285967,-9.2473496812447));
#41246=CARTESIAN_POINT('Ctrl Pts',(6.00007042323265,3.41879962341389,-9.24771882219126));
#41247=CARTESIAN_POINT('Ctrl Pts',(6.00007335753721,3.41493653288833,-9.24811124861399));
#41248=CARTESIAN_POINT('Ctrl Pts',(6.00007601149692,3.41107965124373,-9.24852695617774));
#41249=CARTESIAN_POINT('Ctrl Pts',(6.00009313069709,3.38620107876555,-9.25120845167268));
#41250=CARTESIAN_POINT('Ctrl Pts',(6.00009752492617,3.36158052757525,-9.25486277091957));
#41251=CARTESIAN_POINT('Ctrl Pts',(6.00008809909509,3.33739081585142,-9.2594608407126));
#41252=CARTESIAN_POINT('Ctrl Pts',(6.00007855584451,3.31289976799455,-9.26411618959132));
#41253=CARTESIAN_POINT('Ctrl Pts',(6.00005445404436,3.28885138994719,-9.26973869991398));
#41254=CARTESIAN_POINT('Ctrl Pts',(6.00003199288285,3.26541979533693,-9.27624752567763));
#41255=CARTESIAN_POINT('Ctrl Pts',(6.00001529299223,3.24799838696856,-9.28108684257062));
#41256=CARTESIAN_POINT('Ctrl Pts',(5.99999988409146,3.23091786654435,-9.28641496667356));
#41257=CARTESIAN_POINT('Ctrl Pts',(5.99999988834965,3.21424316874114,-9.29218288031211));
#41258=CARTESIAN_POINT('',(5.72001531699897,3.07996588268296,-9.45352634319216));
#41259=CARTESIAN_POINT('Ctrl Pts',(5.72001583933073,3.07996630535118,-9.4535276405668));
#41260=CARTESIAN_POINT('Ctrl Pts',(5.77262443154598,3.09390593168778,-9.42780571397045));
#41261=CARTESIAN_POINT('Ctrl Pts',(5.82215801010858,3.11234353252729,-9.40145328697083));
#41262=CARTESIAN_POINT('Ctrl Pts',(5.86878812167787,3.13479953409958,-9.37455809133654));
#41263=CARTESIAN_POINT('Ctrl Pts',(5.91541823324956,3.15725553567303,-9.34766289570087));
#41264=CARTESIAN_POINT('Ctrl Pts',(5.9591451108491,3.18373012441069,-9.32022546296157));
#41265=CARTESIAN_POINT('Ctrl Pts',(6.00000005306072,3.21424330184847,-9.2921832651174));
#41266=CARTESIAN_POINT('',(5.732785011186,3.68906787169418,-9.8154400921193));
#41267=CARTESIAN_POINT('Origin',(5.89877268707396,3.22461201072033,-9.89752207294649));
#41268=CARTESIAN_POINT('Ctrl Pts',(5.73278241140467,3.68907514109833,-9.81543880829859));
#41269=CARTESIAN_POINT('Ctrl Pts',(5.74767869655519,3.69181193174699,-9.80076990118021));
#41270=CARTESIAN_POINT('Ctrl Pts',(5.76173623909103,3.6953181596331,-9.78629106413066));
#41271=CARTESIAN_POINT('Ctrl Pts',(5.77495188027913,3.69939287286273,-9.77211145501697));
#41272=CARTESIAN_POINT('Ctrl Pts',(5.78903149098141,3.70373396953599,-9.75700485720687));
#41273=CARTESIAN_POINT('Ctrl Pts',(5.8021556712026,3.70872059120982,-9.7422377839714));
#41274=CARTESIAN_POINT('Ctrl Pts',(5.81434871324948,3.71415040708076,-9.72791047994506));
#41275=CARTESIAN_POINT('Ctrl Pts',(5.81704649346132,3.71535178486279,-9.7247404820772));
#41276=CARTESIAN_POINT('Ctrl Pts',(5.81969878836263,3.71657499800083,-9.72159190038994));
#41277=CARTESIAN_POINT('Ctrl Pts',(5.82230601989191,3.71781808030776,-9.7184656370051));
#41278=CARTESIAN_POINT('Ctrl Pts',(5.83435659809276,3.72356358483297,-9.70401610271081));
#41279=CARTESIAN_POINT('Ctrl Pts',(5.84544360969293,3.72972998718172,-9.69004559213706));
#41280=CARTESIAN_POINT('Ctrl Pts',(5.85563655093317,3.73611851920504,-9.67663236834336));
#41281=CARTESIAN_POINT('Ctrl Pts',(5.85625534830033,3.73650635689613,-9.67581807270749));
#41282=CARTESIAN_POINT('Ctrl Pts',(5.85687085394639,3.73689502613249,-9.675005822708));
#41283=CARTESIAN_POINT('Ctrl Pts',(5.8574830846827,3.73728448728698,-9.67419563274415));
#41284=CARTESIAN_POINT('Ctrl Pts',(5.86845368369367,3.7442632648995,-9.65967779054991));
#41285=CARTESIAN_POINT('Ctrl Pts',(5.87837190542306,3.75149250611659,-9.6458239201788));
#41286=CARTESIAN_POINT('Ctrl Pts',(5.88734074550242,3.75876990355745,-9.63270027080071));
#41287=CARTESIAN_POINT('Ctrl Pts',(5.89145114766236,3.76210512080907,-9.62668572752949));
#41288=CARTESIAN_POINT('Ctrl Pts',(5.89536229525458,3.76545109053723,-9.62082414314524));
#41289=CARTESIAN_POINT('Ctrl Pts',(5.89908473362999,3.7687912671586,-9.61511999917659));
#41290=CARTESIAN_POINT('Ctrl Pts',(5.90118652018917,3.77067721868286,-9.61189928954601));
#41291=CARTESIAN_POINT('Ctrl Pts',(5.90322815175333,3.77256135393962,-9.60872875266206));
#41292=CARTESIAN_POINT('Ctrl Pts',(5.90521156720407,3.77444091972493,-9.60560905069248));
#41293=CARTESIAN_POINT('Ctrl Pts',(5.90881698138608,3.77785755799699,-9.59993811688959));
#41294=CARTESIAN_POINT('Ctrl Pts',(5.91223005913712,3.78125896334876,-9.59443521989477));
#41295=CARTESIAN_POINT('Ctrl Pts',(5.91546371809077,3.78462845364829,-9.58910380772825));
#41296=CARTESIAN_POINT('Ctrl Pts',(5.91797000004203,3.78724001313668,-9.58497163971697));
#41297=CARTESIAN_POINT('Ctrl Pts',(5.92036843045022,3.78983237029622,-9.58094254052739));
#41298=CARTESIAN_POINT('Ctrl Pts',(5.92266498720102,3.79239866553362,-9.57701761862196));
#41299=CARTESIAN_POINT('Ctrl Pts',(5.92381326557642,3.79368181315232,-9.57505515766924));
#41300=CARTESIAN_POINT('Ctrl Pts',(5.92493606868236,3.79495845008678,-9.57311874029835));
#41301=CARTESIAN_POINT('Ctrl Pts',(5.92603412320337,3.79622776990128,-9.57120848851216));
#41302=CARTESIAN_POINT('Ctrl Pts',(5.92680721247964,3.79712143912988,-9.5698635687995));
#41303=CARTESIAN_POINT('Ctrl Pts',(5.9272598572055,3.79764976715791,-9.5690714496196));
#41304=CARTESIAN_POINT('Ctrl Pts',(5.92804436577352,3.79857558745796,-9.56769193863759));
#41305=CARTESIAN_POINT('Ctrl Pts',(5.92837413107571,3.79896475262896,-9.56711206625073));
#41306=CARTESIAN_POINT('Ctrl Pts',(5.92876221561471,3.79942440361365,-9.56642841113834));
#41307=CARTESIAN_POINT('Ctrl Pts',(5.92925474945964,3.80001299631371,-9.56555634204678));
#41308=CARTESIAN_POINT('Ctrl Pts',(5.93919911428426,3.81189681019301,-9.5479490785299));
#41309=CARTESIAN_POINT('Ctrl Pts',(5.94793617624666,3.82418303306961,-9.53098761711083));
#41310=CARTESIAN_POINT('Ctrl Pts',(5.95554257333252,3.8366698253501,-9.51474872794075));
#41311=CARTESIAN_POINT('Ctrl Pts',(5.95842928936594,3.84140870803993,-9.50858588090515));
#41312=CARTESIAN_POINT('Ctrl Pts',(5.96115320676407,3.84617694320634,-9.50252680046662));
#41313=CARTESIAN_POINT('Ctrl Pts',(5.96371874238293,3.85096506477631,-9.49657462218512));
#41314=CARTESIAN_POINT('Ctrl Pts',(5.97059811524388,3.86380420578894,-9.48061411341949));
#41315=CARTESIAN_POINT('Ctrl Pts',(5.97633958264131,3.87678283276641,-9.46542399863919));
#41316=CARTESIAN_POINT('Ctrl Pts',(5.98107332916792,3.88971313303436,-9.45104725786613));
#41317=CARTESIAN_POINT('Ctrl Pts',(5.98611100902723,3.90347363179968,-9.43574744892454));
#41318=CARTESIAN_POINT('Ctrl Pts',(5.99000695882383,3.91717969774421,-9.42136878702499));
#41319=CARTESIAN_POINT('Ctrl Pts',(5.99291129001556,3.93065595429813,-9.40793516398228));
#41320=CARTESIAN_POINT('Ctrl Pts',(5.9936189823796,3.93393968581135,-9.40466182088841));
#41321=CARTESIAN_POINT('Ctrl Pts',(5.99426778641181,3.93720998520123,-9.40144446713658));
#41322=CARTESIAN_POINT('Ctrl Pts',(5.99485986278615,3.94046470722935,-9.39828322180869));
#41323=CARTESIAN_POINT('Ctrl Pts',(5.99739682065465,3.95441069970065,-9.38473776288417));
#41324=CARTESIAN_POINT('Ctrl Pts',(5.99889426464765,3.9680669647464,-9.37222378271122));
#41325=CARTESIAN_POINT('Ctrl Pts',(5.99956526189633,3.98128094884042,-9.36072483287852));
#41326=CARTESIAN_POINT('Ctrl Pts',(5.99985052308264,3.9868986123791,-9.35583628217733));
#41327=CARTESIAN_POINT('Ctrl Pts',(5.99998613323582,3.99243691442869,-9.35113096953797));
#41328=CARTESIAN_POINT('Ctrl Pts',(5.9999873957484,3.99788653423051,-9.34660672477246));
#41329=CARTESIAN_POINT('Ctrl Pts',(5.99970218889552,4.00041486715457,-9.24574070815));
#41330=CARTESIAN_POINT('Ctrl Pts',(5.99970218889552,4.05365232671755,-9.67397475390689));
#41331=CARTESIAN_POINT('Ctrl Pts',(5.99970218889552,4.23216237618003,-10.6067286561567));
#41332=CARTESIAN_POINT('Ctrl Pts',(5.99970218889552,4.71033964600048,-11.9928024105301));
#41333=CARTESIAN_POINT('Ctrl Pts',(5.99970218889552,5.43783896865657,-13.3613500312052));
#41334=CARTESIAN_POINT('Ctrl Pts',(5.99970218889552,6.36842720326896,-14.5997817842042));
#41335=CARTESIAN_POINT('Ctrl Pts',(5.99970218889552,7.4806322410857,-15.6796607105075));
#41336=CARTESIAN_POINT('Ctrl Pts',(5.99970218889552,8.6355046825311,-16.4940256800099));
#41337=CARTESIAN_POINT('Ctrl Pts',(5.99970218889552,9.43064114619334,-16.9071647489066));
#41338=CARTESIAN_POINT('Ctrl Pts',(5.99970218889552,9.77579624644421,-17.0620851371039));
#41339=CARTESIAN_POINT('Ctrl Pts',(6.00690077768462,3.81539387032592,-9.26873651609987));
#41340=CARTESIAN_POINT('Ctrl Pts',(6.00690077768462,3.86963575160847,-9.70506457286073));
#41341=CARTESIAN_POINT('Ctrl Pts',(6.00690077768462,4.05148520857158,-10.6552730337179));
#41342=CARTESIAN_POINT('Ctrl Pts',(6.00690077768462,4.53871003918023,-12.0675567208086));
#41343=CARTESIAN_POINT('Ctrl Pts',(6.00690077768462,5.27984031821352,-13.4617523186532));
#41344=CARTESIAN_POINT('Ctrl Pts',(6.00690077768462,6.22801756506338,-14.7235948399977));
#41345=CARTESIAN_POINT('Ctrl Pts',(6.00690077768462,7.36107910569074,-15.823715865998));
#41346=CARTESIAN_POINT('Ctrl Pts',(6.00690077768462,8.53776162516752,-16.653466849808));
#41347=CARTESIAN_POINT('Ctrl Pts',(6.00690077768462,9.34778507995447,-17.0743424403229));
#41348=CARTESIAN_POINT('Ctrl Pts',(6.00690077768462,9.69945326722534,-17.2321839331678));
#41349=CARTESIAN_POINT('Ctrl Pts',(5.89988018238953,3.66357392134844,-9.28760584687473));
#41350=CARTESIAN_POINT('Ctrl Pts',(5.89988018238953,3.71863998614226,-9.73057548680401));
#41351=CARTESIAN_POINT('Ctrl Pts',(5.89988018238953,3.90322961143632,-10.6951063772361));
#41352=CARTESIAN_POINT('Ctrl Pts',(5.89988018238953,4.39787846548393,-12.12889676203));
#41353=CARTESIAN_POINT('Ctrl Pts',(5.89988018238953,5.15019369723824,-13.5441379420103));
#41354=CARTESIAN_POINT('Ctrl Pts',(5.89988018238953,6.11280370029348,-14.8251902920569));
#41355=CARTESIAN_POINT('Ctrl Pts',(5.89988018238953,7.2629791536517,-15.9419210790931));
#41356=CARTESIAN_POINT('Ctrl Pts',(5.89988018238953,8.45755804700211,-16.7842971376075));
#41357=CARTESIAN_POINT('Ctrl Pts',(5.89988018238953,9.27979710040495,-17.2115209714956));
#41358=CARTESIAN_POINT('Ctrl Pts',(5.89988018238953,9.63680963537774,-17.3717593920753));
#41359=CARTESIAN_POINT('Ctrl Pts',(5.72194802639809,3.60705103823582,-9.29463093801039));
#41360=CARTESIAN_POINT('Ctrl Pts',(5.72194802639809,3.6624239482688,-9.74007325318647));
#41361=CARTESIAN_POINT('Ctrl Pts',(5.72194802639809,3.84803374393823,-10.7099364139704));
#41362=CARTESIAN_POINT('Ctrl Pts',(5.72194802639809,4.34544657736628,-12.1517337870921));
#41363=CARTESIAN_POINT('Ctrl Pts',(5.72194802639809,5.10192599030869,-13.5748102811249));
#41364=CARTESIAN_POINT('Ctrl Pts',(5.72194802639809,6.06990933854909,-14.8630144903926));
#41365=CARTESIAN_POINT('Ctrl Pts',(5.72194802639809,7.22645633724943,-15.9859291260432));
#41366=CARTESIAN_POINT('Ctrl Pts',(5.72194802639809,8.42769808785784,-16.8330055261617));
#41367=CARTESIAN_POINT('Ctrl Pts',(5.72194802639809,9.25448503406041,-17.2625928242768));
#41368=CARTESIAN_POINT('Ctrl Pts',(5.72194802639809,9.61348728080861,-17.42372362604));
#41369=CARTESIAN_POINT('Ctrl Pts',(5.7327834389226,3.6890722712595,-9.81543931491054));
#41370=CARTESIAN_POINT('Ctrl Pts',(5.73338951170027,3.73677170904278,-10.084157914535));
#41371=CARTESIAN_POINT('Ctrl Pts',(5.73395354707033,3.79517197547473,-10.3512385133618));
#41372=CARTESIAN_POINT('Ctrl Pts',(5.7344755542285,3.86412906900604,-10.6157496455956));
#41373=CARTESIAN_POINT('Ctrl Pts',(5.73532470372123,3.97630163230417,-11.046030131679));
#41374=CARTESIAN_POINT('Ctrl Pts',(5.73606263992312,4.11640986609988,-11.4695137403519));
#41375=CARTESIAN_POINT('Ctrl Pts',(5.73668942140747,4.28354912573053,-11.8826273916816));
#41376=CARTESIAN_POINT('Ctrl Pts',(5.73681690169486,4.31754336675963,-11.9666500507909));
#41377=CARTESIAN_POINT('Ctrl Pts',(5.73693978387871,4.35265576367259,-12.050243567833));
#41378=CARTESIAN_POINT('Ctrl Pts',(5.73705806847412,4.38887864994803,-12.1333776205571));
#41379=CARTESIAN_POINT('Ctrl Pts',(5.737074784282,4.39399761582651,-12.1451260046035));
#41380=CARTESIAN_POINT('Ctrl Pts',(5.73709140827173,4.39913875918398,-12.156865212573));
#41381=CARTESIAN_POINT('Ctrl Pts',(5.73710794044476,4.4043020414885,-12.1685951647897));
#41382=CARTESIAN_POINT('Ctrl Pts',(5.73767502817134,4.58141330323435,-12.5709567857097));
#41383=CARTESIAN_POINT('Ctrl Pts',(5.73813408881124,4.78457573118237,-12.9624318471077));
#41384=CARTESIAN_POINT('Ctrl Pts',(5.73848518367753,5.01222354854569,-13.3397802562608));
#41385=CARTESIAN_POINT('Ctrl Pts',(5.73855071710513,5.05471503215729,-13.4102140250933));
#41386=CARTESIAN_POINT('Ctrl Pts',(5.7386124889663,5.0980595256941,-13.4801554890252));
#41387=CARTESIAN_POINT('Ctrl Pts',(5.73867049957996,5.14224676627578,-13.5495833927193));
#41388=CARTESIAN_POINT('Ctrl Pts',(5.73897977937872,5.37782815409092,-13.9197337277492));
#41389=CARTESIAN_POINT('Ctrl Pts',(5.73918215116736,5.63736614834506,-14.2752900546389));
#41390=CARTESIAN_POINT('Ctrl Pts',(5.73927764632016,5.91884386064799,-14.6132513264352));
#41391=CARTESIAN_POINT('Ctrl Pts',(5.73929840882404,5.98004259088702,-14.6867306812824));
#41392=CARTESIAN_POINT('Ctrl Pts',(5.73931411902131,6.04227833582952,-14.7593781301047));
#41393=CARTESIAN_POINT('Ctrl Pts',(5.73932477703137,6.10553019429181,-14.8311625497617));
#41394=CARTESIAN_POINT('Ctrl Pts',(5.73937358627051,6.39519731501835,-15.1599052406577));
#41395=CARTESIAN_POINT('Ctrl Pts',(5.73931644079047,6.7061775767551,-15.4705511644378));
#41396=CARTESIAN_POINT('Ctrl Pts',(5.73915333151696,7.03610866911516,-15.7604158973285));
#41397=CARTESIAN_POINT('Ctrl Pts',(5.73911747414971,7.10863955650045,-15.8241387375975));
#41398=CARTESIAN_POINT('Ctrl Pts',(5.73907649562849,7.18208617501254,-15.8868571080663));
#41399=CARTESIAN_POINT('Ctrl Pts',(5.7390303956456,7.25642321283939,-15.9485422260026));
#41400=CARTESIAN_POINT('Ctrl Pts',(5.73900084443127,7.30407506865231,-15.9880838923325));
#41401=CARTESIAN_POINT('Ctrl Pts',(5.73896918874389,7.35209280736278,-16.0272009802856));
#41402=CARTESIAN_POINT('Ctrl Pts',(5.73893542848712,7.40046852655848,-16.0658876523886));
#41403=CARTESIAN_POINT('Ctrl Pts',(5.73869640194024,7.74297424835245,-16.3397937931704));
#41404=CARTESIAN_POINT('Ctrl Pts',(5.7383518708658,8.10342832194923,-16.5921267927799));
#41405=CARTESIAN_POINT('Ctrl Pts',(5.7379017997706,8.47900281544137,-16.8207962970312));
#41406=CARTESIAN_POINT('Ctrl Pts',(5.73786596841235,8.5089033008736,-16.8390012851205));
#41407=CARTESIAN_POINT('Ctrl Pts',(5.7378294681113,8.53889960067031,-16.8570562728187));
#41408=CARTESIAN_POINT('Ctrl Pts',(5.73779229884403,8.56899027663243,-16.8749601964822));
#41409=CARTESIAN_POINT('Ctrl Pts',(5.7374116956997,8.87711057941036,-17.0582914844555));
#41410=CARTESIAN_POINT('Ctrl Pts',(5.73696095042956,9.19512814699331,-17.2257845440857));
#41411=CARTESIAN_POINT('Ctrl Pts',(5.73644003522278,9.52122270927801,-17.3763183336487));
#41412=CARTESIAN_POINT('Ctrl Pts',(5.99999999930592,3.99788653280082,-9.34660672570642));
#41413=CARTESIAN_POINT('Ctrl Pts',(5.99999999931562,4.01825013013249,-9.49792584808906));
#41414=CARTESIAN_POINT('Ctrl Pts',(5.99999999835918,4.04202369835754,-9.64825763309733));
#41415=CARTESIAN_POINT('Ctrl Pts',(5.99999999609537,4.06917084562767,-9.79770306355383));
#41416=CARTESIAN_POINT('Ctrl Pts',(5.99999999382034,4.09645246929592,-9.94788878848784));
#41417=CARTESIAN_POINT('Ctrl Pts',(5.99999999024012,4.12714128448646,-10.0971798054401));
#41418=CARTESIAN_POINT('Ctrl Pts',(5.99999999039158,4.1612523170038,-10.2456708113104));
#41419=CARTESIAN_POINT('Ctrl Pts',(5.9999999904855,4.18240376014979,-10.3377465661783));
#41420=CARTESIAN_POINT('Ctrl Pts',(5.99999999231395,4.20487204400595,-10.4295145418709));
#41421=CARTESIAN_POINT('Ctrl Pts',(5.99999999505291,4.22867045872271,-10.5209946588892));
#41422=CARTESIAN_POINT('Ctrl Pts',(5.99999999721692,4.24747323717649,-10.5932717577503));
#41423=CARTESIAN_POINT('Ctrl Pts',(5.99999999999964,4.26710647649524,-10.6653691270461));
#41424=CARTESIAN_POINT('Ctrl Pts',(5.99999999999964,4.28757893858364,-10.7372995788032));
#41425=CARTESIAN_POINT('Ctrl Pts',(5.99999999999964,4.33786650361673,-10.9139860591577));
#41426=CARTESIAN_POINT('Ctrl Pts',(5.99999998462025,4.39314036643884,-11.0896695597218));
#41427=CARTESIAN_POINT('Ctrl Pts',(5.99999998025196,4.45330086234597,-11.2638532657156));
#41428=CARTESIAN_POINT('Ctrl Pts',(5.99999997588671,4.51341961085679,-11.4379160997636));
#41429=CARTESIAN_POINT('Ctrl Pts',(5.99999998175306,4.57841809273495,-11.6104807782189));
#41430=CARTESIAN_POINT('Ctrl Pts',(5.99999999007196,4.6481466218464,-11.7810648390995));
#41431=CARTESIAN_POINT('Ctrl Pts',(5.99999999337622,4.67584266136247,-11.8488205045518));
#41432=CARTESIAN_POINT('Ctrl Pts',(5.99999999675167,4.70428439666252,-11.9162638791355));
#41433=CARTESIAN_POINT('Ctrl Pts',(5.99999999861009,4.73346031539168,-11.9833655503387));
#41434=CARTESIAN_POINT('Ctrl Pts',(5.99999999947165,4.74698625511949,-12.0144738478616));
#41435=CARTESIAN_POINT('Ctrl Pts',(5.99999999999964,4.76066997194886,-12.0455087123589));
#41436=CARTESIAN_POINT('Ctrl Pts',(5.99999999999964,4.77450985443936,-12.0764672813386));
#41437=CARTESIAN_POINT('Ctrl Pts',(5.99999999999964,4.86135087722856,-12.270722817549));
#41438=CARTESIAN_POINT('Ctrl Pts',(5.99999998564323,4.95440536705064,-12.4619541304201));
#41439=CARTESIAN_POINT('Ctrl Pts',(5.9999999850471,5.05350689336951,-12.6499608882332));
#41440=CARTESIAN_POINT('Ctrl Pts',(5.99999998445025,5.15272837313359,-12.8381952112428));
#41441=CARTESIAN_POINT('Ctrl Pts',(5.99999999412997,5.25801178107184,-13.0231976929862));
#41442=CARTESIAN_POINT('Ctrl Pts',(5.99999999838051,5.36923781847837,-13.2047465952675));
#41443=CARTESIAN_POINT('Ctrl Pts',(5.99999999937177,5.3951765530956,-13.2470851421233));
#41444=CARTESIAN_POINT('Ctrl Pts',(5.99999999999964,5.42143867719124,-13.2892357558119));
#41445=CARTESIAN_POINT('Ctrl Pts',(5.99999999999964,5.44802302870523,-13.3311954148891));
#41446=CARTESIAN_POINT('Ctrl Pts',(5.99999999999964,5.45163175457307,-13.3368912810094));
#41447=CARTESIAN_POINT('Ctrl Pts',(5.9999999999881,5.45524638131076,-13.3425836503172));
#41448=CARTESIAN_POINT('Ctrl Pts',(5.99999999996605,5.45886690005094,-13.3482725046921));
#41449=CARTESIAN_POINT('Ctrl Pts',(5.99999999925239,5.57604743761589,-13.5323961238789));
#41450=CARTESIAN_POINT('Ctrl Pts',(5.9999999904792,5.6994038552837,-13.7128355868706));
#41451=CARTESIAN_POINT('Ctrl Pts',(5.99999999007258,5.82856569873213,-13.8890427222146));
#41452=CARTESIAN_POINT('Ctrl Pts',(5.99999998966571,5.95780733724832,-14.0653587168001));
#41453=CARTESIAN_POINT('Ctrl Pts',(5.99999999693157,6.09286125024825,-14.2374366970401));
#41454=CARTESIAN_POINT('Ctrl Pts',(5.99999999941398,6.23331363007942,-14.4047572445278));
#41455=CARTESIAN_POINT('Ctrl Pts',(5.9999999997784,6.25393228767317,-14.4293201966202));
#41456=CARTESIAN_POINT('Ctrl Pts',(5.99999999999964,6.27466721652169,-14.4537806817704));
#41457=CARTESIAN_POINT('Ctrl Pts',(5.99999999999964,6.2955170368321,-14.4781371198393));
#41458=CARTESIAN_POINT('Ctrl Pts',(5.99999999999964,6.32570182820854,-14.5133985269324));
#41459=CARTESIAN_POINT('Ctrl Pts',(5.99999999953038,6.35612835002207,-14.5484407605217));
#41460=CARTESIAN_POINT('Ctrl Pts',(5.9999999987273,6.38679509714238,-14.5832618902974));
#41461=CARTESIAN_POINT('Ctrl Pts',(5.99999999501563,6.5285310601452,-14.7441986320471));
#41462=CARTESIAN_POINT('Ctrl Pts',(5.99999998445148,6.67539562223214,-14.9004153354487));
#41463=CARTESIAN_POINT('Ctrl Pts',(5.99999998419194,6.82720685789883,-15.0517239487321));
#41464=CARTESIAN_POINT('Ctrl Pts',(5.99999998393239,6.97901809356552,-15.2030325620155));
#41465=CARTESIAN_POINT('Ctrl Pts',(5.99999999999964,7.13577644841082,-15.3494334645929));
#41466=CARTESIAN_POINT('Ctrl Pts',(5.99999999999964,7.29733248735904,-15.4906976622844));
#41467=CARTESIAN_POINT('Ctrl Pts',(5.99999999999964,7.36277783087636,-15.5479229074984));
#41468=CARTESIAN_POINT('Ctrl Pts',(5.99999999597129,7.4290034226837,-15.6043166838342));
#41469=CARTESIAN_POINT('Ctrl Pts',(5.99999999157416,7.49596991329926,-15.6598390584008));
#41470=CARTESIAN_POINT('Ctrl Pts',(5.99999998233606,7.63666220114164,-15.776487994793));
#41471=CARTESIAN_POINT('Ctrl Pts',(5.99999997355904,7.78062676030411,-15.8892879071132));
#41472=CARTESIAN_POINT('Ctrl Pts',(5.99999997660567,7.92745072947075,-15.9979560613712));
#41473=CARTESIAN_POINT('Ctrl Pts',(5.99999997965611,8.07445806097555,-16.1067599267598));
#41474=CARTESIAN_POINT('Ctrl Pts',(5.99999999487372,8.22433156184451,-16.211421464211));
#41475=CARTESIAN_POINT('Ctrl Pts',(5.99999999914232,8.37662831455504,-16.3117005488194));
#41476=CARTESIAN_POINT('Ctrl Pts',(5.9999999996836,8.39594054927499,-16.3244165994573));
#41477=CARTESIAN_POINT('Ctrl Pts',(5.99999999999964,8.41529171670325,-16.3370622409303));
#41478=CARTESIAN_POINT('Ctrl Pts',(5.99999999999964,8.43468088597692,-16.349637036712));
#41479=CARTESIAN_POINT('Ctrl Pts',(5.99999999999964,8.5422003635077,-16.419368516871));
#41480=CARTESIAN_POINT('Ctrl Pts',(5.99999999306094,8.65090074866789,-16.4868827931156));
#41481=CARTESIAN_POINT('Ctrl Pts',(5.99999999145038,8.76083030931053,-16.5522396053082));
#41482=CARTESIAN_POINT('Ctrl Pts',(5.99999998952809,8.89203703813673,-16.630246407884));
#41483=CARTESIAN_POINT('Ctrl Pts',(5.9999999927489,9.02499432575621,-16.7051809905324));
#41484=CARTESIAN_POINT('Ctrl Pts',(5.99999999547941,9.15977750377954,-16.7771012992923));
#41485=CARTESIAN_POINT('Ctrl Pts',(5.99999999819766,9.2939557808812,-16.8486988328981));
#41486=CARTESIAN_POINT('Ctrl Pts',(5.99999999961509,9.42994399508163,-16.917309315494));
#41487=CARTESIAN_POINT('Ctrl Pts',(5.99999999985075,9.56784100775507,-16.9829446186675));
#41488=CARTESIAN_POINT('Ctrl Pts',(5.99999999991364,9.60463633082665,-17.0004582118799));
#41489=CARTESIAN_POINT('Ctrl Pts',(5.99999999993319,9.64156767640953,-17.0177597130991));
#41490=CARTESIAN_POINT('Ctrl Pts',(5.99999999993288,9.67863716454227,-17.0348487658772));
#41491=CARTESIAN_POINT('Ctrl Pts',(-5.843530343918,3.68097998125157,-9.5215919621966));
#41492=CARTESIAN_POINT('Ctrl Pts',(-3.895686895945,3.12097286918903,-10.4634459889947));
#41493=CARTESIAN_POINT('Ctrl Pts',(0.0001666015266437,2.56014793946572,
-11.405543724591));
#41494=CARTESIAN_POINT('Ctrl Pts',(3.896020098999,3.1210208372572,-10.4633654101759));
#41495=CARTESIAN_POINT('Ctrl Pts',(5.844030148498,3.68112368174947,-9.52135027794804));
#41496=CARTESIAN_POINT('Ctrl Pts',(-5.843530343918,3.79656867134517,-10.3003500893644));
#41497=CARTESIAN_POINT('Ctrl Pts',(-3.895686895945,3.28180629096974,-11.180108871291));
#41498=CARTESIAN_POINT('Ctrl Pts',(0.0001666015266437,2.76478792290348,
-12.0604741630417));
#41499=CARTESIAN_POINT('Ctrl Pts',(3.896020098999,3.28185051220906,-11.1800335725302));
#41500=CARTESIAN_POINT('Ctrl Pts',(5.844030148498,3.79670076181209,-10.3001243390543));
#41501=CARTESIAN_POINT('Ctrl Pts',(-5.843530343918,4.23580747360814,-11.9384157807471));
#41502=CARTESIAN_POINT('Ctrl Pts',(-3.895686895945,3.77920767318315,-12.6803385188317));
#41503=CARTESIAN_POINT('Ctrl Pts',(0.0001666015266437,3.32382461832179,
-13.4219179025983));
#41504=CARTESIAN_POINT('Ctrl Pts',(3.896020098999,3.77924662267507,-12.6802750906046));
#41505=CARTESIAN_POINT('Ctrl Pts',(5.844030148498,4.23592463931539,-11.938225399815));
#41506=CARTESIAN_POINT('Ctrl Pts',(-5.843530343918,5.5035950710752,-14.2139339843063));
#41507=CARTESIAN_POINT('Ctrl Pts',(-3.895686895945,5.02273055892627,-14.7660279845512));
#41508=CARTESIAN_POINT('Ctrl Pts',(0.0001666015266437,4.54131537343804,
-15.3185232177601));
#41509=CARTESIAN_POINT('Ctrl Pts',(3.896020098999,5.02277173497978,-14.7659807289319));
#41510=CARTESIAN_POINT('Ctrl Pts',(5.844030148498,5.50371846320554,-14.2137923143453));
#41511=CARTESIAN_POINT('Ctrl Pts',(-5.843530343918,7.3885050858399,-16.156062941913));
#41512=CARTESIAN_POINT('Ctrl Pts',(-3.895686895945,6.77499147815254,-16.5818456382825));
#41513=CARTESIAN_POINT('Ctrl Pts',(0.0001666015266437,6.16225586059323,
-17.0065483907037));
#41514=CARTESIAN_POINT('Ctrl Pts',(3.896020098999,6.7750438862104,-16.5818093129175));
#41515=CARTESIAN_POINT('Ctrl Pts',(5.844030148498,7.38866251637734,-16.1559536840225));
#41516=CARTESIAN_POINT('Ctrl Pts',(-5.843530343918,8.93341756257242,-17.0810053340763));
#41517=CARTESIAN_POINT('Ctrl Pts',(-3.895686895945,8.18554666399747,-17.491591968287));
#41518=CARTESIAN_POINT('Ctrl Pts',(0.0001666015266437,7.43613425203332,
-17.9044829814061));
#41519=CARTESIAN_POINT('Ctrl Pts',(3.896020098999,8.18561076219368,-17.4915566531935));
#41520=CARTESIAN_POINT('Ctrl Pts',(5.844030148498,8.93360946981109,-17.0808999756088));
#41521=CARTESIAN_POINT('Ctrl Pts',(-5.843530343918,9.74782183257114,-17.434906675706));
#41522=CARTESIAN_POINT('Ctrl Pts',(-3.895686895945,8.92798459116701,-17.8601636149315));
#41523=CARTESIAN_POINT('Ctrl Pts',(0.0001666015266437,8.1080647953231,-18.2855106697697));
#41524=CARTESIAN_POINT('Ctrl Pts',(3.896020098999,8.92805471995194,-17.86012723446));
#41525=CARTESIAN_POINT('Ctrl Pts',(5.844030148498,9.74803220673196,-17.4347975527403));
#41526=CARTESIAN_POINT('Ctrl Pts',(-5.73278975501784,3.68906394501494,-9.81543852467968));
#41527=CARTESIAN_POINT('Ctrl Pts',(-5.37901312686398,3.59283532062234,-9.98633382004624));
#41528=CARTESIAN_POINT('Ctrl Pts',(-5.01621706148927,3.50244639616453,-10.1410528069802));
#41529=CARTESIAN_POINT('Ctrl Pts',(-4.64601453417756,3.41960856061868,-10.2790753857095));
#41530=CARTESIAN_POINT('Ctrl Pts',(-4.37165623574712,3.35821717096216,-10.3813643682297));
#41531=CARTESIAN_POINT('Ctrl Pts',(-4.09323005633235,3.30097639447212,-10.4744809579979));
#41532=CARTESIAN_POINT('Ctrl Pts',(-3.81139253999388,3.24858254091202,-10.5582409695191));
#41533=CARTESIAN_POINT('Ctrl Pts',(-3.57235399153529,3.20414505485315,-10.629281446433));
#41534=CARTESIAN_POINT('Ctrl Pts',(-3.33086150898132,3.16319478165567,-10.6935907748667));
#41535=CARTESIAN_POINT('Ctrl Pts',(-3.08731565576137,3.12613831654997,-10.7510928452597));
#41536=CARTESIAN_POINT('Ctrl Pts',(-3.04370967163684,3.11950349354746,-10.7613883782591));
#41537=CARTESIAN_POINT('Ctrl Pts',(-3.00003786142227,3.11299343151016,-10.7714658046476));
#41538=CARTESIAN_POINT('Ctrl Pts',(-2.95630252426794,3.10661037140673,-10.7813248529935));
#41539=CARTESIAN_POINT('Ctrl Pts',(-2.75784317738745,3.07764573956327,-10.8260625964956));
#41540=CARTESIAN_POINT('Ctrl Pts',(-2.55807094835414,3.05131357907767,-10.866364096742));
#41541=CARTESIAN_POINT('Ctrl Pts',(-2.35725261120207,3.02779065953336,-10.9021038314712));
#41542=CARTESIAN_POINT('Ctrl Pts',(-2.16327810578139,3.00506939438713,-10.9366255662206));
#41543=CARTESIAN_POINT('Ctrl Pts',(-1.9683275793972,2.98496919543223,-10.9668911187537));
#41544=CARTESIAN_POINT('Ctrl Pts',(-1.77264145029077,2.96762488254539,-10.9928288224598));
#41545=CARTESIAN_POINT('Ctrl Pts',(-1.58004668869298,2.95055456784925,-11.0183567731862));
#41546=CARTESIAN_POINT('Ctrl Pts',(-1.38673938228074,2.93615384392036,-11.0396923982212));
#41547=CARTESIAN_POINT('Ctrl Pts',(-1.19294873426629,2.92452605748633,-11.0568097509667));
#41548=CARTESIAN_POINT('Ctrl Pts',(-0.99481114965818,2.91263744706069,-11.0743110646918));
#41549=CARTESIAN_POINT('Ctrl Pts',(-0.796168296488997,2.9036478299414,-11.0874023173225));
#41550=CARTESIAN_POINT('Ctrl Pts',(-0.597265150369091,2.89763823993256,
-11.0961050744984));
#41551=CARTESIAN_POINT('Ctrl Pts',(-0.408473574731138,2.89193415737359,
-11.1043654126162));
#41552=CARTESIAN_POINT('Ctrl Pts',(-0.219447498295875,2.88891469255251,
-11.1086723131217));
#41553=CARTESIAN_POINT('Ctrl Pts',(-0.030396402586863,2.88862252261748,
-11.1090887091539));
#41554=CARTESIAN_POINT('Ctrl Pts',(-0.0202709323560394,2.88860687416028,
-11.1091110110909));
#41555=CARTESIAN_POINT('Ctrl Pts',(-0.010145390354594,2.88859904285181,
-11.1091221633804));
#41556=CARTESIAN_POINT('Ctrl Pts',(-1.98087675444825E-5,2.88859903306065,
-11.1091221793492));
#41557=CARTESIAN_POINT('Ctrl Pts',(-1.32058452790807E-5,2.88859903305426,
-11.1091221793596));
#41558=CARTESIAN_POINT('Ctrl Pts',(-6.60292303140436E-6,2.88859903305121,
-11.1091221793653));
#41559=CARTESIAN_POINT('Ctrl Pts',(-7.99360577730113E-13,2.88859903305147,
-11.1091221793662));
#41560=CARTESIAN_POINT('Ctrl Pts',(0.189405503646998,2.88859904071486,-11.1091222063918));
#41561=CARTESIAN_POINT('Ctrl Pts',(0.378797279580155,2.8913380614621,-11.1052218521454));
#41562=CARTESIAN_POINT('Ctrl Pts',(0.567964667945599,2.89677460616661,-11.097355447509));
#41563=CARTESIAN_POINT('Ctrl Pts',(0.769363593162857,2.90256267709069,-11.0889804022499));
#41564=CARTESIAN_POINT('Ctrl Pts',(0.970508174933544,2.91140858960037,-11.0761095047332));
#41565=CARTESIAN_POINT('Ctrl Pts',(1.171144190504,2.92322964262542,-11.0587180531935));
#41566=CARTESIAN_POINT('Ctrl Pts',(1.36695866628512,2.93476662064355,-11.0417445404538));
#41567=CARTESIAN_POINT('Ctrl Pts',(1.56228872515895,2.94913719244932,-11.0204655771592));
#41568=CARTESIAN_POINT('Ctrl Pts',(1.75689803534998,2.96623568336572,-10.9949064346219));
#41569=CARTESIAN_POINT('Ctrl Pts',(1.95869514303697,2.9839656984886,-10.9684032779439));
#41570=CARTESIAN_POINT('Ctrl Pts',(2.15971727784271,3.00462885550607,-10.9372979254205));
#41571=CARTESIAN_POINT('Ctrl Pts',(2.35970094251548,3.0280777242204,-10.9016683699337));
#41572=CARTESIAN_POINT('Ctrl Pts',(2.55968460718826,3.05152659293472,-10.8660388144469));
#41573=CARTESIAN_POINT('Ctrl Pts',(2.75862980172807,3.07776097135519,-10.825885376108));
#41574=CARTESIAN_POINT('Ctrl Pts',(2.95627302888323,3.10660622105748,-10.7813321095109));
#41575=CARTESIAN_POINT('Ctrl Pts',(3.19877084584174,3.14199782128135,-10.7266676009231));
#41576=CARTESIAN_POINT('Ctrl Pts',(3.43931583985532,3.18129608636574,-10.6652855428938));
#41577=CARTESIAN_POINT('Ctrl Pts',(3.67751607631245,3.2241077234401,-10.5972522151377));
#41578=CARTESIAN_POINT('Ctrl Pts',(3.96233417229581,3.27529797051463,-10.51590417299));
#41579=CARTESIAN_POINT('Ctrl Pts',(4.2437999231366,3.33151069708892,-10.4250471694021));
#41580=CARTESIAN_POINT('Ctrl Pts',(4.52124330571427,3.39203867129015,-10.3248614333745));
#41581=CARTESIAN_POINT('Ctrl Pts',(4.88827658264392,3.47211187581421,-10.192324486001));
#41582=CARTESIAN_POINT('Ctrl Pts',(5.24827032461013,3.55973199273167,-10.0434649111247));
#41583=CARTESIAN_POINT('Ctrl Pts',(5.59967327730505,3.6532475106715,-9.8787802312009));
#41584=CARTESIAN_POINT('Ctrl Pts',(5.6441832833375,3.66509253427107,-9.85792065662804));
#41585=CARTESIAN_POINT('Ctrl Pts',(5.6885554613365,3.6770322090519,-9.83680721171413));
#41586=CARTESIAN_POINT('Ctrl Pts',(5.7327866589135,3.68906325963484,-9.81544090738039));
#41587=CARTESIAN_POINT('Ctrl Pts',(-5.84422094409324,3.72283000523856,-9.78167408162266));
#41588=CARTESIAN_POINT('Ctrl Pts',(-5.38507933576137,3.59683815761584,-10.0152843826947));
#41589=CARTESIAN_POINT('Ctrl Pts',(-4.35131200003916,3.34345413932339,-10.4619161435517));
#41590=CARTESIAN_POINT('Ctrl Pts',(-2.68512122938073,3.05355923238929,-10.9303254787283));
#41591=CARTESIAN_POINT('Ctrl Pts',(-0.894430115197969,2.89419166045093,
-11.1728831745123));
#41592=CARTESIAN_POINT('Ctrl Pts',(0.897577000464036,2.89433296944046,-11.1726725040321));
#41593=CARTESIAN_POINT('Ctrl Pts',(2.68825409632356,3.05397482372149,-10.9296798875333));
#41594=CARTESIAN_POINT('Ctrl Pts',(4.35334874826658,3.34391794571683,-10.4611286604278));
#41595=CARTESIAN_POINT('Ctrl Pts',(5.38611390228171,3.59711968962454,-10.014763833926));
#41596=CARTESIAN_POINT('Ctrl Pts',(5.84433011088186,3.72285991154443,-9.78161853339931));
#41597=CARTESIAN_POINT('Ctrl Pts',(-5.7253823284647,3.64455025382003,-9.50229674233198));
#41598=CARTESIAN_POINT('Ctrl Pts',(-5.27548411908097,3.52282891856501,-9.73077840355672));
#41599=CARTESIAN_POINT('Ctrl Pts',(-4.26255740633406,3.27781652768212,-10.1677131448542));
#41600=CARTESIAN_POINT('Ctrl Pts',(-2.63017516266764,2.99718831488208,-10.6260529752425));
#41601=CARTESIAN_POINT('Ctrl Pts',(-0.876088458604595,2.84283318581267,
-10.8634076236384));
#41602=CARTESIAN_POINT('Ctrl Pts',(0.879170849863336,2.8429700697441,-10.8632014724712));
#41603=CARTESIAN_POINT('Ctrl Pts',(2.63324420333494,2.99759077241429,-10.6254212356259));
#41604=CARTESIAN_POINT('Ctrl Pts',(4.26455304776783,3.27826526122104,-10.1669426530745));
#41605=CARTESIAN_POINT('Ctrl Pts',(5.27649785620924,3.52310092714498,-9.73026926825663));
#41606=CARTESIAN_POINT('Ctrl Pts',(5.72548929810404,3.6445791484027,-9.5022424109029));
#41607=CARTESIAN_POINT('Ctrl Pts',(-5.71943584543031,3.37475341540664,-9.34268206148292));
#41608=CARTESIAN_POINT('Ctrl Pts',(-5.27084297399291,3.25437642499162,-9.56884092463208));
#41609=CARTESIAN_POINT('Ctrl Pts',(-4.26059460930962,3.01185372124479,-10.0016516746214));
#41610=CARTESIAN_POINT('Ctrl Pts',(-2.6305607665523,2.73346781021963,-10.4564761199075));
#41611=CARTESIAN_POINT('Ctrl Pts',(-0.876566641464214,2.58004209268039,
-10.6924012836617));
#41612=CARTESIAN_POINT('Ctrl Pts',(0.879650375344035,2.58017826058766,-10.6921962381974));
#41613=CARTESIAN_POINT('Ctrl Pts',(2.63362771378936,2.73386754327752,-10.4558485735717));
#41614=CARTESIAN_POINT('Ctrl Pts',(4.26258539034863,3.01229823853514,-10.0008879757299));
#41615=CARTESIAN_POINT('Ctrl Pts',(5.27185378417918,3.25464542811177,-9.56833693988253));
#41616=CARTESIAN_POINT('Ctrl Pts',(5.71954249942017,3.37478198354303,-9.34262828327426));
#41617=CARTESIAN_POINT('Ctrl Pts',(-5.83023996337941,3.08845069594387,-9.4063707542719));
#41618=CARTESIAN_POINT('Ctrl Pts',(-5.37416754064385,2.96561979924004,-9.63451945103832));
#41619=CARTESIAN_POINT('Ctrl Pts',(-4.34669767293009,2.71808976474014,-10.0714544604592));
#41620=CARTESIAN_POINT('Ctrl Pts',(-2.68602843357863,2.4334671496755,-10.5315980787564));
#41621=CARTESIAN_POINT('Ctrl Pts',(-0.895554653482513,2.27628487850067,
-10.7707946411655));
#41622=CARTESIAN_POINT('Ctrl Pts',(0.898704696302249,2.27642450392807,-10.7705865705077));
#41623=CARTESIAN_POINT('Ctrl Pts',(2.68915637879637,2.43387633501067,-10.5309623471982));
#41624=CARTESIAN_POINT('Ctrl Pts',(4.3487229931822,2.71854365750337,-10.0706829494537));
#41625=CARTESIAN_POINT('Ctrl Pts',(5.37519522517315,2.96589426453183,-9.63401101278662));
#41626=CARTESIAN_POINT('Ctrl Pts',(5.83034838799569,3.08847983468315,-9.40631650684342));
#41627=CARTESIAN_POINT('Ctrl Pts',(-5.72001753233616,3.07996681168233,-9.45352318625267));
#41628=CARTESIAN_POINT('Ctrl Pts',(-5.54305534100265,3.03310276487157,-9.54003493482035));
#41629=CARTESIAN_POINT('Ctrl Pts',(-5.3615059653871,2.98701684693875,-9.62354209665977));
#41630=CARTESIAN_POINT('Ctrl Pts',(-5.1753597899198,2.94208361578591,-9.70365867399441));
#41631=CARTESIAN_POINT('Ctrl Pts',(-4.99261523307681,2.89797149049547,-9.78231120813346));
#41632=CARTESIAN_POINT('Ctrl Pts',(-4.80544024685734,2.85497027317297,-9.85769593441277));
#41633=CARTESIAN_POINT('Ctrl Pts',(-4.6138516950545,2.81347141986786,-9.9294257276793));
#41634=CARTESIAN_POINT('Ctrl Pts',(-4.54633624105595,2.79884730013341,-9.95470317516789));
#41635=CARTESIAN_POINT('Ctrl Pts',(-4.47827293657318,2.78441009408221,-9.97952653607247));
#41636=CARTESIAN_POINT('Ctrl Pts',(-4.40966334609503,2.77017807323515,-10.0038782076587));
#41637=CARTESIAN_POINT('Ctrl Pts',(-4.40581152306788,2.76937907086188,-10.0052453391152));
#41638=CARTESIAN_POINT('Ctrl Pts',(-4.40195797835678,2.76858071535721,-10.0066109837952));
#41639=CARTESIAN_POINT('Ctrl Pts',(-4.39810271264232,2.76778301002835,-10.0079751385947));
#41640=CARTESIAN_POINT('Ctrl Pts',(-4.20696612240203,2.72823432833767,-10.0756072854423));
#41641=CARTESIAN_POINT('Ctrl Pts',(-4.01159851371404,2.69026623838527,-10.1395832951787));
#41642=CARTESIAN_POINT('Ctrl Pts',(-3.81207290579326,2.65420530166328,-10.1995431025816));
#41643=CARTESIAN_POINT('Ctrl Pts',(-3.76843043495447,2.64631765057073,-10.2126581817604));
#41644=CARTESIAN_POINT('Ctrl Pts',(-3.72458910374073,2.63852139568591,-10.2255810089721));
#41645=CARTESIAN_POINT('Ctrl Pts',(-3.6805497995005,2.63082021387585,-10.2383076400666));
#41646=CARTESIAN_POINT('Ctrl Pts',(-3.55786021758428,2.60936540679298,-10.2737629015682));
#41647=CARTESIAN_POINT('Ctrl Pts',(-3.43363449003342,2.5886457533485,-10.3076961673479));
#41648=CARTESIAN_POINT('Ctrl Pts',(-3.30789770372184,2.56872932468178,-10.340022384266));
#41649=CARTESIAN_POINT('Ctrl Pts',(-3.24502931056605,2.55877111034841,-10.356185492725));
#41650=CARTESIAN_POINT('Ctrl Pts',(-3.18178314679223,2.54901369546737,-10.3719468108874));
#41651=CARTESIAN_POINT('Ctrl Pts',(-3.11816301394347,2.53946498461077,-10.3872955340494));
#41652=CARTESIAN_POINT('Ctrl Pts',(-3.08635294751909,2.53469062918247,-10.3949698956304));
#41653=CARTESIAN_POINT('Ctrl Pts',(-3.05444938858022,2.52996844940208,-10.4025411068631));
#41654=CARTESIAN_POINT('Ctrl Pts',(-3.02245283213984,2.52529941032688,-10.4100078084096));
#41655=CARTESIAN_POINT('Ctrl Pts',(-3.00645455391965,2.52296489078928,-10.4137411591829));
#41656=CARTESIAN_POINT('Ctrl Pts',(-2.99043302631282,2.52064365640634,-10.4174483824348));
#41657=CARTESIAN_POINT('Ctrl Pts',(-2.97438831367734,2.51833582545579,-10.4211293077042));
#41658=CARTESIAN_POINT('Ctrl Pts',(-2.95955595302759,2.51620237615352,-10.4245320991634));
#41659=CARTESIAN_POINT('Ctrl Pts',(-2.94352577511445,2.5139130275725,-10.4281786877099));
#41660=CARTESIAN_POINT('Ctrl Pts',(-2.92956478792253,2.51193203497011,-10.4313304172836));
#41661=CARTESIAN_POINT('Ctrl Pts',(-2.92842365934937,2.51177011466815,-10.4315880300599));
#41662=CARTESIAN_POINT('Ctrl Pts',(-2.9272963626467,2.51161024093396,-10.4318423609015));
#41663=CARTESIAN_POINT('Ctrl Pts',(-2.92618468578872,2.51145266038476,-10.4320930187536));
#41664=CARTESIAN_POINT('Ctrl Pts',(-2.83482829520798,2.49850286288042,-10.4526918074003));
#41665=CARTESIAN_POINT('Ctrl Pts',(-2.74308865013777,2.48609382009464,-10.4723429839348));
#41666=CARTESIAN_POINT('Ctrl Pts',(-2.65097987157538,2.47424830538277,-10.491036159891));
#41667=CARTESIAN_POINT('Ctrl Pts',(-2.40077663237707,2.44207128385301,-10.541814090596));
#41668=CARTESIAN_POINT('Ctrl Pts',(-2.14784930868952,2.41405016388818,-10.585526059997));
#41669=CARTESIAN_POINT('Ctrl Pts',(-1.89260573277423,2.39051010363169,-10.6219891796602));
#41670=CARTESIAN_POINT('Ctrl Pts',(-1.64481354069086,2.36765725371446,-10.6573878231682));
#41671=CARTESIAN_POINT('Ctrl Pts',(-1.3948379837133,2.34902750915391,-10.6859546344191));
#41672=CARTESIAN_POINT('Ctrl Pts',(-1.14305895590474,2.33494920718288,-10.7074846403153));
#41673=CARTESIAN_POINT('Ctrl Pts',(-1.05633093452868,2.33009978312676,-10.7149008847415));
#41674=CARTESIAN_POINT('Ctrl Pts',(-0.969389011244006,2.32579068746956,
-10.7214818557861));
#41675=CARTESIAN_POINT('Ctrl Pts',(-0.882249031691758,2.32203627246146,
-10.727218107575));
#41676=CARTESIAN_POINT('Ctrl Pts',(-0.625764048147959,2.31098564935461,
-10.7441020046476));
#41677=CARTESIAN_POINT('Ctrl Pts',(-0.367561507220804,2.30473871258826,
-10.7536705579575));
#41678=CARTESIAN_POINT('Ctrl Pts',(-0.108124721210384,2.30337804384068,
-10.7557538378253));
#41679=CARTESIAN_POINT('Ctrl Pts',(-0.0721012726907265,2.30318911157192,
-10.7560431064607));
#41680=CARTESIAN_POINT('Ctrl Pts',(-0.0360540656339076,2.30309442682546,
-10.7561879977457));
#41681=CARTESIAN_POINT('Ctrl Pts',(1.55675634620075E-5,2.30309424985344,
-10.7561879973148));
#41682=CARTESIAN_POINT('Ctrl Pts',(0.258123167549015,2.3030929834745,-10.7561879942312));
#41683=CARTESIAN_POINT('Ctrl Pts',(0.515061792059015,2.3078718503129,-10.7487843545561));
#41684=CARTESIAN_POINT('Ctrl Pts',(0.77037644122687,2.31739613540424,-10.7341395381072));
#41685=CARTESIAN_POINT('Ctrl Pts',(0.808742208416225,2.31882733610365,-10.7319388824838));
#41686=CARTESIAN_POINT('Ctrl Pts',(0.84707132814878,2.32036574238111,-10.7295746387273));
#41687=CARTESIAN_POINT('Ctrl Pts',(0.885362278207682,2.32201128975929,-10.7270472762613));
#41688=CARTESIAN_POINT('Ctrl Pts',(1.08656404905455,2.33065790328005,-10.7137671199067));
#41689=CARTESIAN_POINT('Ctrl Pts',(1.2867118663148,2.34226152640888,-10.6959845869193));
#41690=CARTESIAN_POINT('Ctrl Pts',(1.48561773745142,2.35667529156902,-10.6738045705339));
#41691=CARTESIAN_POINT('Ctrl Pts',(1.72995221186358,2.3743810521611,-10.6465588054139));
#41692=CARTESIAN_POINT('Ctrl Pts',(1.97240063589042,2.39636085514469,-10.6126717426014));
#41693=CARTESIAN_POINT('Ctrl Pts',(2.21261554862799,2.42228886661666,-10.5723239222172));
#41694=CARTESIAN_POINT('Ctrl Pts',(2.33272300499677,2.43525287235264,-10.5521500120251));
#41695=CARTESIAN_POINT('Ctrl Pts',(2.45227253079915,2.44920181630043,-10.5303609011959));
#41696=CARTESIAN_POINT('Ctrl Pts',(2.57122332400129,2.46408272756912,-10.5069791448595));
#41697=CARTESIAN_POINT('Ctrl Pts',(2.59887870385466,2.46754245442442,-10.5015430200913));
#41698=CARTESIAN_POINT('Ctrl Pts',(2.62650176530099,2.47105249563266,-10.4960208074496));
#41699=CARTESIAN_POINT('Ctrl Pts',(2.65409192553637,2.47461221620557,-10.4904127836425));
#41700=CARTESIAN_POINT('Ctrl Pts',(2.68583690121256,2.47870799680405,-10.4839602448451));
#41701=CARTESIAN_POINT('Ctrl Pts',(2.71753832026729,2.48286954562529,-10.4773941044017));
#41702=CARTESIAN_POINT('Ctrl Pts',(2.74919555557085,2.48709559038792,-10.4707148841878));
#41703=CARTESIAN_POINT('Ctrl Pts',(2.77878112492963,2.49104508058311,-10.4644727556189));
#41704=CARTESIAN_POINT('Ctrl Pts',(2.80832805715831,2.49505096219467,-10.4581318569174));
#41705=CARTESIAN_POINT('Ctrl Pts',(2.83783575611512,2.49911229294227,-10.4516926038457));
#41706=CARTESIAN_POINT('Ctrl Pts',(2.85258960559352,2.50114295831608,-10.4484729773099));
#41707=CARTESIAN_POINT('Ctrl Pts',(2.86733364675631,2.50318748596766,-10.4452287621483));
#41708=CARTESIAN_POINT('Ctrl Pts',(2.88206780592029,2.50524575524457,-10.441960010658));
#41709=CARTESIAN_POINT('Ctrl Pts',(2.89584461574247,2.50717028884539,-10.4389036457079));
#41710=CARTESIAN_POINT('Ctrl Pts',(2.90840992863005,2.5089366641677,-10.436096477744));
#41711=CARTESIAN_POINT('Ctrl Pts',(2.923137806357,2.51102209973565,-10.4327794102906));
#41712=CARTESIAN_POINT('Ctrl Pts',(2.92416124532654,2.51116701647575,-10.4325489075556));
#41713=CARTESIAN_POINT('Ctrl Pts',(2.92519512135964,2.51131348378967,-10.4323159249662));
#41714=CARTESIAN_POINT('Ctrl Pts',(2.92624056398715,2.51146166644494,-10.4320801995225));
#41715=CARTESIAN_POINT('Ctrl Pts',(3.13297121031788,2.54076398805763,-10.3854667632059));
#41716=CARTESIAN_POINT('Ctrl Pts',(3.33587866711728,2.57241886503027,-10.3344575226723));
#41717=CARTESIAN_POINT('Ctrl Pts',(3.53485207388181,2.60603621417604,-10.2794357398157));
#41718=CARTESIAN_POINT('Ctrl Pts',(3.73806256971372,2.64036943638673,-10.2232422818173));
#41719=CARTESIAN_POINT('Ctrl Pts',(3.93716971927397,2.67674968545062,-10.1628635658874));
#41720=CARTESIAN_POINT('Ctrl Pts',(4.13208039840941,2.71480311244308,-10.098683050252));
#41721=CARTESIAN_POINT('Ctrl Pts',(4.22656654105684,2.73325013416083,-10.0675704945808));
#41722=CARTESIAN_POINT('Ctrl Pts',(4.32006688591088,2.75209095923471,-10.0355641548993));
#41723=CARTESIAN_POINT('Ctrl Pts',(4.41257282447384,2.77128632053656,-10.0027056903117));
#41724=CARTESIAN_POINT('Ctrl Pts',(4.61058268702672,2.81237417837655,-9.93237182680255));
#41725=CARTESIAN_POINT('Ctrl Pts',(4.804035331853,2.85508378576198,-9.85813547086469));
#41726=CARTESIAN_POINT('Ctrl Pts',(4.9929108501,2.8990635906378,-9.78039118652011));
#41727=CARTESIAN_POINT('Ctrl Pts',(5.1857817011965,2.94397371173864,-9.70100235715463));
#41728=CARTESIAN_POINT('Ctrl Pts',(5.37387978343848,2.99020842254106,-9.61795560508356));
#41729=CARTESIAN_POINT('Ctrl Pts',(5.55720283873327,3.03743585162211,-9.53164303677593));
#41730=CARTESIAN_POINT('Ctrl Pts',(5.61189830411155,3.05152642090732,-9.50589119621235));
#41731=CARTESIAN_POINT('Ctrl Pts',(5.66616883817662,3.06570563505726,-9.47984846050826));
#41732=CARTESIAN_POINT('Ctrl Pts',(5.72001468712874,3.0799653729863,-9.45352477868309));
#41733=CARTESIAN_POINT('Ctrl Pts',(6.05078165618827,-4.09458887238873,-9.54443970746419));
#41734=CARTESIAN_POINT('Ctrl Pts',(6.0514309326576,-4.06997623068921,-9.55470507407486));
#41735=CARTESIAN_POINT('Ctrl Pts',(6.04719970398084,-4.00805739104224,-9.58290432047297));
#41736=CARTESIAN_POINT('Ctrl Pts',(6.01579032749343,-3.90976504771429,-9.63742351885017));
#41737=CARTESIAN_POINT('Ctrl Pts',(5.94768463712015,-3.81080368340423,-9.70642972249064));
#41738=CARTESIAN_POINT('Ctrl Pts',(5.84925760035456,-3.7329089217144,-9.77799616062866));
#41739=CARTESIAN_POINT('Ctrl Pts',(5.76422183048588,-3.69954275308194,-9.82519790048264));
#41740=CARTESIAN_POINT('Ctrl Pts',(5.71689747708232,-3.6892852770504,-9.84791207876869));
#41741=CARTESIAN_POINT('Ctrl Pts',(5.71188842785141,-3.68828725659104,-9.85027878928298));
#41742=CARTESIAN_POINT('Ctrl Pts',(5.9119338424872,-3.98202445464115,-9.28409234374272));
#41743=CARTESIAN_POINT('Ctrl Pts',(5.91252983174185,-3.959875089295,-9.29332121776031));
#41744=CARTESIAN_POINT('Ctrl Pts',(5.90864954675052,-3.90395398774346,-9.31884235613713));
#41745=CARTESIAN_POINT('Ctrl Pts',(5.87953897617286,-3.81456732430523,-9.36882529662082));
#41746=CARTESIAN_POINT('Ctrl Pts',(5.81605214418774,-3.72418838849228,-9.43267821318822));
#41747=CARTESIAN_POINT('Ctrl Pts',(5.72407864663328,-3.652997061284,-9.49923100425177));
#41748=CARTESIAN_POINT('Ctrl Pts',(5.64462215644559,-3.6226165199218,-9.54320383514445));
#41749=CARTESIAN_POINT('Ctrl Pts',(5.60046280975658,-3.61333517226186,-9.56435438307519));
#41750=CARTESIAN_POINT('Ctrl Pts',(5.59578948546033,-3.61243316965986,-9.5665580338794));
#41751=CARTESIAN_POINT('Ctrl Pts',(6.02851721676376,-3.8715554395682,-9.01218059937768));
#41752=CARTESIAN_POINT('Ctrl Pts',(6.02945192459048,-3.83742568340882,-9.02642167041017));
#41753=CARTESIAN_POINT('Ctrl Pts',(6.02333299803029,-3.7529376633562,-9.06490257042747));
#41754=CARTESIAN_POINT('Ctrl Pts',(5.98020755072705,-3.62309265216294,-9.13676063368903));
#41755=CARTESIAN_POINT('Ctrl Pts',(5.88943948424395,-3.4952859482716,-9.22561325181903));
#41756=CARTESIAN_POINT('Ctrl Pts',(5.75992263904637,-3.39562764242272,-9.31708718700472));
#41757=CARTESIAN_POINT('Ctrl Pts',(5.64799870728207,-3.35285012688804,-9.37787341286657));
#41758=CARTESIAN_POINT('Ctrl Pts',(5.58526054501384,-3.33966614696647,-9.40748009093418));
#41759=CARTESIAN_POINT('Ctrl Pts',(5.57861458744835,-3.33838322120361,-9.41056941987632));
#41760=CARTESIAN_POINT('Ctrl Pts',(6.32410045353725,-3.83560443861232,-8.90696767285684));
#41761=CARTESIAN_POINT('Ctrl Pts',(6.32554382421795,-3.78290488455112,-8.92898366934629));
#41762=CARTESIAN_POINT('Ctrl Pts',(6.31606430844593,-3.65401356063343,-8.98756587194144));
#41763=CARTESIAN_POINT('Ctrl Pts',(6.25179835610878,-3.46087038311676,-9.09336926176179));
#41764=CARTESIAN_POINT('Ctrl Pts',(6.11973434725635,-3.27416309711438,-9.22098494131091));
#41765=CARTESIAN_POINT('Ctrl Pts',(5.93329042167987,-3.1295301513967,-9.35097668483132));
#41766=CARTESIAN_POINT('Ctrl Pts',(5.77213775295316,-3.0671004297697,-9.4375958660983));
#41767=CARTESIAN_POINT('Ctrl Pts',(5.68125709334696,-3.0476935953827,-9.48013465539532));
#41768=CARTESIAN_POINT('Ctrl Pts',(5.67162338877499,-3.04580253600233,-9.48457775597017));
#41769=CARTESIAN_POINT('',(5.73278595301787,-3.68906554369663,-9.815438227342));
#41770=CARTESIAN_POINT('',(5.7200159288464,-3.07996626094983,-9.45352720243893));
#41771=CARTESIAN_POINT('Origin',(5.89875613670428,-3.22462513219392,-9.8974987073781));
#41772=CARTESIAN_POINT('',(5.99999998876135,-3.2142420670336,-9.29218347180064));
#41773=CARTESIAN_POINT('Ctrl Pts',(6.00000005573716,-3.21424213478534,-9.29218366766699));
#41774=CARTESIAN_POINT('Ctrl Pts',(5.95912832913167,-3.18371657550664,-9.32023732779621));
#41775=CARTESIAN_POINT('Ctrl Pts',(5.91539006756828,-3.15723896628417,-9.34768031862321));
#41776=CARTESIAN_POINT('Ctrl Pts',(5.86875892973,-3.13478493225045,-9.37457511033737));
#41777=CARTESIAN_POINT('Ctrl Pts',(5.82212779189173,-3.11233089821673,-9.40146990205153));
#41778=CARTESIAN_POINT('Ctrl Pts',(5.77260355260912,-3.09390025876082,-9.42781596698812));
#41779=CARTESIAN_POINT('Ctrl Pts',(5.72001606108407,-3.07996636795448,-9.45352753089058));
#41780=CARTESIAN_POINT('',(5.99998733812332,-3.99788407449396,-9.34660788725514));
#41781=CARTESIAN_POINT('Ctrl Pts',(5.99998733812332,-3.99788407449396,-9.34660788725514));
#41782=CARTESIAN_POINT('Ctrl Pts',(5.99998488596604,-3.97180407808845,-9.3357140563781));
#41783=CARTESIAN_POINT('Ctrl Pts',(5.9999858305139,-3.94582833044417,-9.3256565521199));
#41784=CARTESIAN_POINT('Ctrl Pts',(5.99998224149706,-3.91995848301427,-9.31646864591698));
#41785=CARTESIAN_POINT('Ctrl Pts',(5.99998112254582,-3.91189301572182,-9.3136041235356));
#41786=CARTESIAN_POINT('Ctrl Pts',(5.99997934669105,-3.90383796951955,-9.310823799426));
#41787=CARTESIAN_POINT('Ctrl Pts',(5.99997632633964,-3.89579365835037,-9.30812785308905));
#41788=CARTESIAN_POINT('Ctrl Pts',(5.99996219472167,-3.85815594109312,-9.29551406132529));
#41789=CARTESIAN_POINT('Ctrl Pts',(5.99992491129164,-3.82075549376394,-9.28475071122847));
#41790=CARTESIAN_POINT('Ctrl Pts',(5.99991412123476,-3.78357059890767,-9.27578193406091));
#41791=CARTESIAN_POINT('Ctrl Pts',(5.99990486207759,-3.75166151908597,-9.26808565234089));
#41792=CARTESIAN_POINT('Ctrl Pts',(5.99990277981739,-3.71991114528791,-9.26173564795763));
#41793=CARTESIAN_POINT('Ctrl Pts',(5.99990414412111,-3.68833374065537,-9.25673100183795));
#41794=CARTESIAN_POINT('Ctrl Pts',(5.99990504451532,-3.6674937238673,-9.25342810502404));
#41795=CARTESIAN_POINT('Ctrl Pts',(5.99990781486193,-3.64672846175442,-9.250710922078));
#41796=CARTESIAN_POINT('Ctrl Pts',(5.99991537550728,-3.6260312685207,-9.24858454831112));
#41797=CARTESIAN_POINT('Ctrl Pts',(5.99991828174551,-3.61807546957057,-9.24776719100131));
#41798=CARTESIAN_POINT('Ctrl Pts',(5.99992634338063,-3.60986023920379,-9.24700690180229));
#41799=CARTESIAN_POINT('Ctrl Pts',(5.99993169908744,-3.60175447189294,-9.2463532514576));
#41800=CARTESIAN_POINT('Ctrl Pts',(5.99993712301145,-3.59354545904762,-9.24569127537686));
#41801=CARTESIAN_POINT('Ctrl Pts',(5.99993949878579,-3.58544904623269,-9.24513871128581));
#41802=CARTESIAN_POINT('Ctrl Pts',(5.99994451384018,-3.57786438072415,-9.24469668443833));
#41803=CARTESIAN_POINT('Ctrl Pts',(5.99994534777804,-3.57660315019569,-9.24462318116336));
#41804=CARTESIAN_POINT('Ctrl Pts',(5.99994628951504,-3.57535609798006,-9.24455262588208));
#41805=CARTESIAN_POINT('Ctrl Pts',(5.99994740674549,-3.57412508935423,-9.24448489874969));
#41806=CARTESIAN_POINT('Ctrl Pts',(5.9999742135278,-3.54458831805716,-9.24285985666782));
#41807=CARTESIAN_POINT('Ctrl Pts',(5.99996031027524,-3.51545847374159,-9.24253337306945));
#41808=CARTESIAN_POINT('Ctrl Pts',(5.99993575361401,-3.48674310711012,-9.24342493463139));
#41809=CARTESIAN_POINT('Ctrl Pts',(5.99991415256481,-3.46148388960773,-9.24420918884966));
#41810=CARTESIAN_POINT('Ctrl Pts',(5.99988537901417,-3.43654429589967,-9.24593621729577));
#41811=CARTESIAN_POINT('Ctrl Pts',(5.99986870330864,-3.41191858348489,-9.2485831616114));
#41812=CARTESIAN_POINT('Ctrl Pts',(5.99985078225209,-3.38545380908684,-9.25142778120972));
#41813=CARTESIAN_POINT('Ctrl Pts',(5.99984832471424,-3.35935020724328,-9.25533463258301));
#41814=CARTESIAN_POINT('Ctrl Pts',(5.99986773243008,-3.33359881707214,-9.26031735681989));
#41815=CARTESIAN_POINT('Ctrl Pts',(5.99988654285589,-3.30863994925345,-9.26514673320612));
#41816=CARTESIAN_POINT('Ctrl Pts',(5.99992646290735,-3.28401122807348,-9.2709876518158));
#41817=CARTESIAN_POINT('Ctrl Pts',(5.99996032824771,-3.25972320748426,-9.27788278843555));
#41818=CARTESIAN_POINT('Ctrl Pts',(5.99998165966428,-3.24442444245233,-9.28222596142575));
#41819=CARTESIAN_POINT('Ctrl Pts',(5.99999988603535,-3.22926128485911,-9.28698799135304));
#41820=CARTESIAN_POINT('Ctrl Pts',(5.99999989033238,-3.21424200111748,-9.29218328124107));
#41821=CARTESIAN_POINT('Ctrl Pts',(5.99998733812332,-3.99788407449396,-9.34660788725514));
#41822=CARTESIAN_POINT('Ctrl Pts',(5.99998442648227,-3.98506455951682,-9.35725069887637));
#41823=CARTESIAN_POINT('Ctrl Pts',(5.99923934431779,-3.97175114978455,-9.36889665012024));
#41824=CARTESIAN_POINT('Ctrl Pts',(5.99754757095219,-3.9580775449888,-9.38156938257316));
#41825=CARTESIAN_POINT('Ctrl Pts',(5.99683713707804,-3.95233552763226,-9.38689109917871));
#41826=CARTESIAN_POINT('Ctrl Pts',(5.99595953918619,-3.94653051018614,-9.392393686159));
#41827=CARTESIAN_POINT('Ctrl Pts',(5.99489848361549,-3.94067479526504,-9.39807799691719));
#41828=CARTESIAN_POINT('Ctrl Pts',(5.99250382409841,-3.92745923535258,-9.41090672071916));
#41829=CARTESIAN_POINT('Ctrl Pts',(5.98917443765327,-3.91398268590984,-9.42466279085472));
#41830=CARTESIAN_POINT('Ctrl Pts',(5.98476532291861,-3.90040413868406,-9.4393294105634));
#41831=CARTESIAN_POINT('Ctrl Pts',(5.98056462641809,-3.88746744747819,-9.45330274121877));
#41832=CARTESIAN_POINT('Ctrl Pts',(5.97538423138413,-3.87443775181405,-9.46810266737493));
#41833=CARTESIAN_POINT('Ctrl Pts',(5.96909466645958,-3.86149238497048,-9.48369242079305));
#41834=CARTESIAN_POINT('Ctrl Pts',(5.96741551873607,-3.85803631391848,-9.48785447322056));
#41835=CARTESIAN_POINT('Ctrl Pts',(5.96565727348637,-3.85458649918978,-9.49207268886684));
#41836=CARTESIAN_POINT('Ctrl Pts',(5.96381735718526,-3.85114688309128,-9.49634606941855));
#41837=CARTESIAN_POINT('Ctrl Pts',(5.96351328401592,-3.850578436055,-9.49705230826613));
#41838=CARTESIAN_POINT('Ctrl Pts',(5.96320698007237,-3.85001026815408,-9.49776005350371));
#41839=CARTESIAN_POINT('Ctrl Pts',(5.96289843783564,-3.84944239465364,-9.49846930029565));
#41840=CARTESIAN_POINT('Ctrl Pts',(5.95831416539658,-3.84100501873863,-9.50900717853002));
#41841=CARTESIAN_POINT('Ctrl Pts',(5.95323565980044,-3.83263199254864,-9.51987698043347));
#41842=CARTESIAN_POINT('Ctrl Pts',(5.94763907818266,-3.82437747432279,-9.53105996212404));
#41843=CARTESIAN_POINT('Ctrl Pts',(5.94484078737377,-3.82025021520986,-9.53665145296933));
#41844=CARTESIAN_POINT('Ctrl Pts',(5.94191293623144,-3.81615260702795,-9.5423212351393));
#41845=CARTESIAN_POINT('Ctrl Pts',(5.93885272790819,-3.81209232950736,-9.54806633546841));
#41846=CARTESIAN_POINT('Ctrl Pts',(5.93732262374657,-3.81006219074706,-9.55093888563297));
#41847=CARTESIAN_POINT('Ctrl Pts',(5.93575942704362,-3.8080413864398,-9.55383026506808));
#41848=CARTESIAN_POINT('Ctrl Pts',(5.93416278454396,-3.80603091718481,-9.55674007844489));
#41849=CARTESIAN_POINT('Ctrl Pts',(5.9330991746773,-3.8046916349493,-9.55867846240898));
#41850=CARTESIAN_POINT('Ctrl Pts',(5.93175171859144,-3.80302652765125,-9.56110924344933));
#41851=CARTESIAN_POINT('Ctrl Pts',(5.93065599743354,-3.80169767257101,-9.56306466655013));
#41852=CARTESIAN_POINT('Ctrl Pts',(5.93010687208962,-3.80103171116496,-9.56404463519907));
#41853=CARTESIAN_POINT('Ctrl Pts',(5.92962186463968,-3.80044952661347,-9.56490518456632));
#41854=CARTESIAN_POINT('Ctrl Pts',(5.92927215875649,-3.80003154015743,-9.56552441212107));
#41855=CARTESIAN_POINT('Ctrl Pts',(5.92326911397194,-3.79285639231029,-9.57615406098208));
#41856=CARTESIAN_POINT('Ctrl Pts',(5.91647655577503,-3.78540876595849,-9.58765163498892));
#41857=CARTESIAN_POINT('Ctrl Pts',(5.90875553078948,-3.77785188769607,-9.59998916486729));
#41858=CARTESIAN_POINT('Ctrl Pts',(5.90763524385544,-3.77675541773316,-9.60177928645697));
#41859=CARTESIAN_POINT('Ctrl Pts',(5.9064953972911,-3.77565672763503,-9.60358705241849));
#41860=CARTESIAN_POINT('Ctrl Pts',(5.90533555419657,-3.77455640091975,-9.60541233540429));
#41861=CARTESIAN_POINT('Ctrl Pts',(5.89751903312143,-3.76714097809225,-9.61771345009286));
#41862=CARTESIAN_POINT('Ctrl Pts',(5.88879369601463,-3.75964795878791,-9.63081225330071));
#41863=CARTESIAN_POINT('Ctrl Pts',(5.87904237408387,-3.75226213629508,-9.64465846120265));
#41864=CARTESIAN_POINT('Ctrl Pts',(5.87007096184807,-3.74546703110276,-9.65739725086347));
#41865=CARTESIAN_POINT('Ctrl Pts',(5.86023095512446,-3.73876252446447,-9.67076877328719));
#41866=CARTESIAN_POINT('Ctrl Pts',(5.8494388689441,-3.73232780646497,-9.68471105146388));
#41867=CARTESIAN_POINT('Ctrl Pts',(5.84101794142072,-3.72730687788807,-9.6955900337176));
#41868=CARTESIAN_POINT('Ctrl Pts',(5.83201744822162,-3.72245074407605,-9.70681616103984));
#41869=CARTESIAN_POINT('Ctrl Pts',(5.82240240038839,-3.71786284377927,-9.71834822089586));
#41870=CARTESIAN_POINT('Ctrl Pts',(5.8105783876476,-3.71222091744633,-9.73252966076286));
#41871=CARTESIAN_POINT('Ctrl Pts',(5.79782361947076,-3.70698410220008,-9.74717460361531));
#41872=CARTESIAN_POINT('Ctrl Pts',(5.78410757713597,-3.70234957630206,-9.76218794847119));
#41873=CARTESIAN_POINT('Ctrl Pts',(5.77126455919935,-3.69801003740423,-9.77624569578389));
#41874=CARTESIAN_POINT('Ctrl Pts',(5.75757862353476,-3.69419833069783,-9.79062652340357));
#41875=CARTESIAN_POINT('Ctrl Pts',(5.74304692965124,-3.69110834401341,-9.80522706601143));
#41876=CARTESIAN_POINT('Ctrl Pts',(5.73967098514949,-3.69039049077199,-9.80861900517109));
#41877=CARTESIAN_POINT('Ctrl Pts',(5.73624949911788,-3.6897117421629,-9.81202268530853));
#41878=CARTESIAN_POINT('Ctrl Pts',(5.73278263502695,-3.68907482142868,-9.81543658880499));
#41879=CARTESIAN_POINT('Ctrl Pts',(5.99928507671105,-9.77920217853695,-17.0543525004093));
#41880=CARTESIAN_POINT('Ctrl Pts',(5.99928507671105,-9.74894839965409,-17.0407709830188));
#41881=CARTESIAN_POINT('Ctrl Pts',(5.99928507671105,-9.27203920734991,-16.8237867818301));
#41882=CARTESIAN_POINT('Ctrl Pts',(5.99928507671105,-8.38193522942945,-16.3303542912131));
#41883=CARTESIAN_POINT('Ctrl Pts',(5.99928507671105,-7.21246426312353,-15.4323267873847));
#41884=CARTESIAN_POINT('Ctrl Pts',(5.99928507671105,-6.18849730658614,-14.3709116157454));
#41885=CARTESIAN_POINT('Ctrl Pts',(5.99928507671105,-5.33271053138996,-13.1688951809494));
#41886=CARTESIAN_POINT('Ctrl Pts',(5.99928507671105,-4.66383020185381,-11.8527237226987));
#41887=CARTESIAN_POINT('Ctrl Pts',(5.99928507671105,-4.22479091101948,-10.5321726316834));
#41888=CARTESIAN_POINT('Ctrl Pts',(5.99928507671105,-4.05899861709883,-9.64833292798501));
#41889=CARTESIAN_POINT('Ctrl Pts',(5.99928507671105,-4.00882230477428,-9.24471639752991));
#41890=CARTESIAN_POINT('Ctrl Pts',(6.01063076682066,-9.70160365670749,-17.2272481798314));
#41891=CARTESIAN_POINT('Ctrl Pts',(6.01063076682066,-9.67076859172804,-17.2134055071903));
#41892=CARTESIAN_POINT('Ctrl Pts',(6.01063076682066,-9.18470271755529,-16.9922531320754));
#41893=CARTESIAN_POINT('Ctrl Pts',(6.01063076682066,-8.27768704363521,-16.4894545190853));
#41894=CARTESIAN_POINT('Ctrl Pts',(6.01063076682066,-7.08568152473405,-15.5741206058228));
#41895=CARTESIAN_POINT('Ctrl Pts',(6.01063076682066,-6.04222139176158,-14.4924942432127));
#41896=CARTESIAN_POINT('Ctrl Pts',(6.01063076682066,-5.16996888347368,-13.2673642990713));
#41897=CARTESIAN_POINT('Ctrl Pts',(6.01063076682066,-4.48832934805044,-11.9260686457922));
#41898=CARTESIAN_POINT('Ctrl Pts',(6.01063076682066,-4.04084801205732,-10.5801430309673));
#41899=CARTESIAN_POINT('Ctrl Pts',(6.01063076682066,-3.87189820410474,-9.67946904936188));
#41900=CARTESIAN_POINT('Ctrl Pts',(6.01063076682066,-3.82075861600654,-9.26809120543838));
#41901=CARTESIAN_POINT('Ctrl Pts',(5.90351705923382,-9.63722444731814,-17.3706901795732));
#41902=CARTESIAN_POINT('Ctrl Pts',(5.90351705923382,-9.60590712136365,-17.3566308408348));
#41903=CARTESIAN_POINT('Ctrl Pts',(5.90351705923382,-9.11224445377126,-17.1320203619313));
#41904=CARTESIAN_POINT('Ctrl Pts',(5.90351705923382,-8.19119807937274,-16.6214511943171));
#41905=CARTESIAN_POINT('Ctrl Pts',(5.90351705923382,-6.98049688630115,-15.6917591086185));
#41906=CARTESIAN_POINT('Ctrl Pts',(5.90351705923382,-5.92086434104531,-14.5933646367085));
#41907=CARTESIAN_POINT('Ctrl Pts',(5.90351705923382,-5.03495112308005,-13.3490586899501));
#41908=CARTESIAN_POINT('Ctrl Pts',(5.90351705923382,-4.34272597895849,-11.9869188791486));
#41909=CARTESIAN_POINT('Ctrl Pts',(5.90351705923382,-3.88824074417813,-10.6199414228328));
#41910=CARTESIAN_POINT('Ctrl Pts',(5.90351705923382,-3.71667132115728,-9.70530097025956));
#41911=CARTESIAN_POINT('Ctrl Pts',(5.90351705923382,-3.66473255633256,-9.28748399304876));
#41912=CARTESIAN_POINT('Ctrl Pts',(5.7219541158257,-9.61342486666327,-17.4237175384707));
#41913=CARTESIAN_POINT('Ctrl Pts',(5.7219541158257,-9.58192925940845,-17.4095781030297));
#41914=CARTESIAN_POINT('Ctrl Pts',(5.7219541158257,-9.08545822403752,-17.1836892390603));
#41915=CARTESIAN_POINT('Ctrl Pts',(5.7219541158257,-8.1592250076253,-16.670247467953));
#41916=CARTESIAN_POINT('Ctrl Pts',(5.7219541158257,-6.94161243417266,-15.7352474810556));
#41917=CARTESIAN_POINT('Ctrl Pts',(5.7219541158257,-5.87600130305989,-14.6306542071787));
#41918=CARTESIAN_POINT('Ctrl Pts',(5.7219541158257,-4.98503802057335,-13.3792593131512));
#41919=CARTESIAN_POINT('Ctrl Pts',(5.7219541158257,-4.28889960925415,-12.0094138748187));
#41920=CARTESIAN_POINT('Ctrl Pts',(5.7219541158257,-3.83182518682086,-10.6346540147708));
#41921=CARTESIAN_POINT('Ctrl Pts',(5.7219541158257,-3.6592873496071,-9.71485046443014));
#41922=CARTESIAN_POINT('Ctrl Pts',(5.7219541158257,-3.60705314668704,-9.29465308097585));
#41923=CARTESIAN_POINT('',(6.,-9.67863108609234,-17.0348569101268));
#41924=CARTESIAN_POINT('Ctrl Pts',(5.99999999999975,-9.67863108609234,-17.0348569101268));
#41925=CARTESIAN_POINT('Ctrl Pts',(5.99999999999975,-9.53996482698304,-16.9709229523293));
#41926=CARTESIAN_POINT('Ctrl Pts',(6.00000000003748,-9.40322990798227,-16.9040238345894));
#41927=CARTESIAN_POINT('Ctrl Pts',(5.99999999795225,-9.26832001841028,-16.8341585314232));
#41928=CARTESIAN_POINT('Ctrl Pts',(5.9999999958601,-9.13296247356695,-16.7640614026188));
#41929=CARTESIAN_POINT('Ctrl Pts',(5.99999999148619,-8.99944169515712,-16.6909781287944));
#41930=CARTESIAN_POINT('Ctrl Pts',(5.9999999908736,-8.86767321980464,-16.6148604837069));
#41931=CARTESIAN_POINT('Ctrl Pts',(5.999999990262,-8.73611954092696,-16.5388669183872));
#41932=CARTESIAN_POINT('Ctrl Pts',(5.99999999695627,-8.60631206866638,-16.4598486138675));
#41933=CARTESIAN_POINT('Ctrl Pts',(5.99999999953315,-8.47819538354683,-16.3777143843573));
#41934=CARTESIAN_POINT('Ctrl Pts',(5.99999999982105,-8.46388161375179,-16.368537980422));
#41935=CARTESIAN_POINT('Ctrl Pts',(5.99999999999975,-8.44958898201702,-16.3593226402141));
#41936=CARTESIAN_POINT('Ctrl Pts',(5.99999999999975,-8.43531743665977,-16.3500682051006));
#41937=CARTESIAN_POINT('Ctrl Pts',(5.99999999999975,-8.41951507644074,-16.3398211075631));
#41938=CARTESIAN_POINT('Ctrl Pts',(5.99999999977976,-8.40373799579059,-16.3295268932043));
#41939=CARTESIAN_POINT('Ctrl Pts',(5.99999999940213,-8.38798676299647,-16.3191857879626));
#41940=CARTESIAN_POINT('Ctrl Pts',(5.99999999572735,-8.23470703684241,-16.218553551725));
#41941=CARTESIAN_POINT('Ctrl Pts',(5.99999998184258,-8.08387696921227,-16.1134769902152));
#41942=CARTESIAN_POINT('Ctrl Pts',(5.99999998033336,-7.93593246474559,-16.0042029928214));
#41943=CARTESIAN_POINT('Ctrl Pts',(5.99999997882273,-7.78785045817077,-15.8948274343386));
#41944=CARTESIAN_POINT('Ctrl Pts',(5.99999998731005,-7.64265976297581,-15.7812468735922));
#41945=CARTESIAN_POINT('Ctrl Pts',(5.99999999411987,-7.50077077039805,-15.6637536647744));
#41946=CARTESIAN_POINT('Ctrl Pts',(5.99999999739303,-7.43257160183055,-15.6072803682337));
#41947=CARTESIAN_POINT('Ctrl Pts',(5.99999999999975,-7.36513478079692,-15.5499037886234));
#41948=CARTESIAN_POINT('Ctrl Pts',(5.99999999999975,-7.2985032883994,-15.4916598064485));
#41949=CARTESIAN_POINT('Ctrl Pts',(5.99999999999975,-7.27238327152466,-15.4688277529776));
#41950=CARTESIAN_POINT('Ctrl Pts',(5.99999999960415,-7.24638785264023,-15.4458614503158));
#41951=CARTESIAN_POINT('Ctrl Pts',(5.99999999898866,-7.22051776537586,-15.4227616312456));
#41952=CARTESIAN_POINT('Ctrl Pts',(5.99999999507861,-7.05617055376858,-15.2760133495707));
#41953=CARTESIAN_POINT('Ctrl Pts',(5.99999998615656,-6.89687872218188,-15.1238800776715));
#41954=CARTESIAN_POINT('Ctrl Pts',(5.99999998771985,-6.74283048209707,-14.9666009211883));
#41955=CARTESIAN_POINT('Ctrl Pts',(5.99999998928315,-6.58878224201225,-14.8093217647052));
#41956=CARTESIAN_POINT('Ctrl Pts',(5.99999999999975,-6.43997714680681,-14.6468962856083));
#41957=CARTESIAN_POINT('Ctrl Pts',(5.99999999999975,-6.29664110038409,-14.4795249794017));
#41958=CARTESIAN_POINT('Ctrl Pts',(5.99999999999975,-6.26385436913173,-14.4412404154493));
#41959=CARTESIAN_POINT('Ctrl Pts',(5.9999999993467,-6.23135170199723,-14.4026986427207));
#41960=CARTESIAN_POINT('Ctrl Pts',(5.99999999845574,-6.19913907434213,-14.3639052805569));
#41961=CARTESIAN_POINT('Ctrl Pts',(5.99999999449763,-6.05603309707375,-14.1915641085351));
#41962=CARTESIAN_POINT('Ctrl Pts',(5.99999998895133,-5.91865446098742,-14.0142547234861));
#41963=CARTESIAN_POINT('Ctrl Pts',(5.99999999115154,-5.78742187725139,-13.8325315580029));
#41964=CARTESIAN_POINT('Ctrl Pts',(5.99999999312721,-5.6695821336787,-13.6693540100791));
#41965=CARTESIAN_POINT('Ctrl Pts',(5.99999999999975,-5.55669768554855,-13.5026183338488));
#41966=CARTESIAN_POINT('Ctrl Pts',(5.99999999999975,-5.44904317682204,-13.3327476292645));
#41967=CARTESIAN_POINT('Ctrl Pts',(5.99999999999975,-5.41325256682299,-13.2762727429828));
#41968=CARTESIAN_POINT('Ctrl Pts',(5.99999999913628,-5.3780422672377,-13.219450528623));
#41969=CARTESIAN_POINT('Ctrl Pts',(5.99999999780775,-5.34341678808511,-13.1622879102247));
#41970=CARTESIAN_POINT('Ctrl Pts',(5.99999999336883,-5.22772507034453,-12.9712944084768));
#41971=CARTESIAN_POINT('Ctrl Pts',(5.99999998477715,-5.11855861803619,-12.7765024093267));
#41972=CARTESIAN_POINT('Ctrl Pts',(5.99999998688354,-5.01608477796987,-12.5781968539945));
#41973=CARTESIAN_POINT('Ctrl Pts',(5.99999998863009,-4.93111681469402,-12.4137683605179));
#41974=CARTESIAN_POINT('Ctrl Pts',(5.99999999999975,-4.85075089132226,-12.2469236105177));
#41975=CARTESIAN_POINT('Ctrl Pts',(5.99999999999975,-4.77510784589638,-12.0778154581411));
#41976=CARTESIAN_POINT('Ctrl Pts',(5.99999999999975,-4.74092204835261,-12.001389436058));
#41977=CARTESIAN_POINT('Ctrl Pts',(5.99999999683355,-4.70768988233596,-11.9245038096418));
#41978=CARTESIAN_POINT('Ctrl Pts',(5.99999999319076,-4.67543337998466,-11.8471991538661));
#41979=CARTESIAN_POINT('Ctrl Pts',(5.99999998466668,-4.59995360841341,-11.6663073232581));
#41980=CARTESIAN_POINT('Ctrl Pts',(5.99999997595979,-4.52981981238297,-11.483119818371));
#41981=CARTESIAN_POINT('Ctrl Pts',(5.99999997954455,-4.46519569756246,-11.298180586888));
#41982=CARTESIAN_POINT('Ctrl Pts',(5.9999999831293,-4.40057158274195,-11.1132413554049));
#41983=CARTESIAN_POINT('Ctrl Pts',(5.99999999999975,-4.34145727180482,-10.9265509189464));
#41984=CARTESIAN_POINT('Ctrl Pts',(5.99999999999975,-4.28796151252698,-10.7386680750688));
#41985=CARTESIAN_POINT('Ctrl Pts',(5.99999999999975,-4.26062856773402,-10.6426718415621));
#41986=CARTESIAN_POINT('Ctrl Pts',(5.99999999545169,-4.23478514967344,-10.5463642320482));
#41987=CARTESIAN_POINT('Ctrl Pts',(5.99999999307294,-4.21041230415808,-10.4497165385558));
#41988=CARTESIAN_POINT('Ctrl Pts',(5.9999999894094,-4.17287556932914,-10.3008689680017));
#41989=CARTESIAN_POINT('Ctrl Pts',(5.99999999031163,-4.13882446525617,-10.1512153093438));
#41990=CARTESIAN_POINT('Ctrl Pts',(5.99999999276244,-4.10822755624092,-10.0006714392445));
#41991=CARTESIAN_POINT('Ctrl Pts',(5.99999999520029,-4.07779233417733,-9.85092310634911));
#41992=CARTESIAN_POINT('Ctrl Pts',(5.99999999786784,-4.05077479923683,-9.70029349478971));
#41993=CARTESIAN_POINT('Ctrl Pts',(5.99999999875695,-4.02719432983824,-9.54868945835378));
#41994=CARTESIAN_POINT('Ctrl Pts',(5.99999999915085,-4.01674728362348,-9.48152309502914));
#41995=CARTESIAN_POINT('Ctrl Pts',(5.99999999931877,-4.00697554670158,-9.41416537293925));
#41996=CARTESIAN_POINT('Ctrl Pts',(5.99999999931449,-3.99788407308631,-9.34660788817994));
#41997=CARTESIAN_POINT('',(5.73644276520394,-9.5212169767595,-17.3763304373435));
#41998=CARTESIAN_POINT('Origin',(5.6,-9.67863108603356,-17.0348569100686));
#41999=CARTESIAN_POINT('Ctrl Pts',(5.73644276397727,-9.52121697613054,-17.3763304378314));
#42000=CARTESIAN_POINT('Ctrl Pts',(5.7370879225765,-9.11866915060707,-17.190470746701));
#42001=CARTESIAN_POINT('Ctrl Pts',(5.73762563119994,-8.7282103260932,-16.9787094510485));
#42002=CARTESIAN_POINT('Ctrl Pts',(5.73805595553824,-8.35333654529934,-16.7430677114181));
#42003=CARTESIAN_POINT('Ctrl Pts',(5.73812189681658,-8.29589230121891,-16.7069588601183));
#42004=CARTESIAN_POINT('Ctrl Pts',(5.73818531654628,-8.23881393095504,-16.6702892103096));
#42005=CARTESIAN_POINT('Ctrl Pts',(5.73824621493434,-8.18211392296719,-16.6330659762319));
#42006=CARTESIAN_POINT('Ctrl Pts',(5.73865147315426,-7.80479450550312,-16.3853579159207));
#42007=CARTESIAN_POINT('Ctrl Pts',(5.73894507726364,-7.44423378224291,-16.1131375843732));
#42008=CARTESIAN_POINT('Ctrl Pts',(5.73912707307373,-7.10336499304846,-15.8189084157108));
#42009=CARTESIAN_POINT('Ctrl Pts',(5.73915087281185,-7.05878930797042,-15.7804318312336));
#42010=CARTESIAN_POINT('Ctrl Pts',(5.7391727638931,-7.01455032175002,-15.7415788234522));
#42011=CARTESIAN_POINT('Ctrl Pts',(5.73919274637924,-6.97065454662951,-15.7023549458821));
#42012=CARTESIAN_POINT('Ctrl Pts',(5.73934700322017,-6.631796631049,-15.3995622202062));
#42013=CARTESIAN_POINT('Ctrl Pts',(5.73938752573454,-6.31339406649295,-15.0746719077206));
#42014=CARTESIAN_POINT('Ctrl Pts',(5.73931432084042,-6.01802942968551,-14.730631055353));
#42015=CARTESIAN_POINT('Ctrl Pts',(5.73930537005946,-5.98191512067613,-14.688565093129));
#42016=CARTESIAN_POINT('Ctrl Pts',(5.7392947190043,-5.94614518966932,-14.6462127796561));
#42017=CARTESIAN_POINT('Ctrl Pts',(5.73928236764773,-5.91072432463659,-14.6035794599369));
#42018=CARTESIAN_POINT('Ctrl Pts',(5.73918135756739,-5.62105052227199,-14.2549218023928));
#42019=CARTESIAN_POINT('Ctrl Pts',(5.73896663323084,-5.35472450905668,-13.887474076343));
#42020=CARTESIAN_POINT('Ctrl Pts',(5.73863815928527,-5.11384103203013,-13.5046257092083));
#42021=CARTESIAN_POINT('Ctrl Pts',(5.73859603612378,-5.08295038228288,-13.4555296277275));
#42022=CARTESIAN_POINT('Ctrl Pts',(5.73855204227779,-5.05247810754861,-13.4061802174161));
#42023=CARTESIAN_POINT('Ctrl Pts',(5.73850617763449,-5.02242859617607,-13.3565845722254));
#42024=CARTESIAN_POINT('Ctrl Pts',(5.73815298350166,-4.79102352361814,-12.9746587654586));
#42025=CARTESIAN_POINT('Ctrl Pts',(5.73768884852362,-4.58469079413331,-12.5781343505374));
#42026=CARTESIAN_POINT('Ctrl Pts',(5.73711370889819,-4.40507707959883,-12.170380536125));
#42027=CARTESIAN_POINT('Ctrl Pts',(5.7370302059657,-4.37899946085101,-12.1111798868718));
#42028=CARTESIAN_POINT('Ctrl Pts',(5.73694436290758,-4.35348502742357,-12.0517424499186));
#42029=CARTESIAN_POINT('Ctrl Pts',(5.73685617955183,-4.32853878640423,-11.992078459459));
#42030=CARTESIAN_POINT('Ctrl Pts',(5.73622835025684,-4.15093179040852,-11.5672953385699));
#42031=CARTESIAN_POINT('Ctrl Pts',(5.73548189400739,-4.0021263642364,-11.1310327750241));
#42032=CARTESIAN_POINT('Ctrl Pts',(5.73461675057501,-3.8830427836656,-10.6872506417479));
#42033=CARTESIAN_POINT('Ctrl Pts',(5.73452239358223,-3.87005491583734,-10.6388494796069));
#42034=CARTESIAN_POINT('Ctrl Pts',(5.73442662479487,-3.85742058667043,-10.5903588204422));
#42035=CARTESIAN_POINT('Ctrl Pts',(5.73432944414849,-3.84514098364243,-10.5417837649701));
#42036=CARTESIAN_POINT('Ctrl Pts',(5.73384873086919,-3.78439876325035,-10.3015026485271));
#42037=CARTESIAN_POINT('Ctrl Pts',(5.73333347080855,-3.73233631768364,-10.0591568647339));
#42038=CARTESIAN_POINT('Ctrl Pts',(5.73278365810998,-3.68907196542854,-9.81543709296658));
#42039=CARTESIAN_POINT('Ctrl Pts',(5.99999999997498,-9.91330135657868,-16.8993650110575));
#42040=CARTESIAN_POINT('Ctrl Pts',(5.99999999997498,-9.8352288888744,-16.9447895967214));
#42041=CARTESIAN_POINT('Ctrl Pts',(5.99999999997498,-9.75700380943188,-16.9899528783353));
#42042=CARTESIAN_POINT('Ctrl Pts',(5.99999999997498,-9.67862816205492,-17.0348534691251));
#42043=CARTESIAN_POINT('Ctrl Pts',(6.00000263486244,-10.0326958051699,-17.1045706743814));
#42044=CARTESIAN_POINT('Ctrl Pts',(6.00000263486244,-9.95416474484388,-17.150262077563));
#42045=CARTESIAN_POINT('Ctrl Pts',(6.00000263486244,-9.87548026973954,-17.195690591635));
#42046=CARTESIAN_POINT('Ctrl Pts',(6.00000263486244,-9.79664425061344,-17.2408549245712));
#42047=CARTESIAN_POINT('Ctrl Pts',(5.83074066841652,-10.116417534179,-17.2484649101534));
#42048=CARTESIAN_POINT('Ctrl Pts',(5.83074066841652,-10.0375648997125,-17.2943434110118));
#42049=CARTESIAN_POINT('Ctrl Pts',(5.83074066841652,-9.95855828736023,-17.3399579112862));
#42050=CARTESIAN_POINT('Ctrl Pts',(5.83074066841652,-9.87939944653079,-17.3853071853881));
#42051=CARTESIAN_POINT('Ctrl Pts',(5.59336110044025,-10.1144359114731,-17.2450590549679));
#42052=CARTESIAN_POINT('Ctrl Pts',(5.59336110044025,-10.0355908883964,-17.2909331273821));
#42053=CARTESIAN_POINT('Ctrl Pts',(5.59336110044025,-9.95659190076218,-17.3365432255193));
#42054=CARTESIAN_POINT('Ctrl Pts',(5.59336110044025,-9.87744070085091,-17.381888122219));
#42055=CARTESIAN_POINT('',(5.99999999995606,-9.91329603789449,-16.8993703023574));
#42056=CARTESIAN_POINT('',(5.59336167790258,-10.1144355809267,-17.2450590897518));
#42057=CARTESIAN_POINT('Origin',(5.6,-9.91330329119712,-16.8993688492374));
#42058=CARTESIAN_POINT('',(5.5933616956255,-9.87744142956214,-17.381887715675));
#42059=CARTESIAN_POINT('Origin',(5.59336169592161,-7.49315402656696,-13.0994163770562));
#42060=CARTESIAN_POINT('Origin',(5.6,-9.67863108611231,-17.0348569102122));
#42061=CARTESIAN_POINT('Ctrl Pts',(5.99999999999155,-9.91329301289976,-16.8993720623907));
#42062=CARTESIAN_POINT('Ctrl Pts',(5.9999999999916,-9.88722393977981,-16.9145397247211));
#42063=CARTESIAN_POINT('Ctrl Pts',(5.99999999999962,-9.86114407693648,-16.9296767195906));
#42064=CARTESIAN_POINT('Ctrl Pts',(5.99999999999962,-9.83508082013908,-16.9447638792498));
#42065=CARTESIAN_POINT('Ctrl Pts',(5.99999999999962,-9.80901756334168,-16.959851038909));
#42066=CARTESIAN_POINT('Ctrl Pts',(5.99999999999962,-9.78297091259021,-16.974888363358));
#42067=CARTESIAN_POINT('Ctrl Pts',(5.99999999999962,-9.75690044718562,-16.9899010654911));
#42068=CARTESIAN_POINT('Ctrl Pts',(5.99999999999962,-9.73082998178102,-17.0049137676242));
#42069=CARTESIAN_POINT('Ctrl Pts',(5.99999999999962,-9.7047357017233,-17.0199018474415));
#42070=CARTESIAN_POINT('Ctrl Pts',(5.99999999999962,-9.67863108609234,-17.0348569101268));
#42071=CARTESIAN_POINT('Origin',(5.6,-9.67863108603356,-17.0348569100686));
#42072=CARTESIAN_POINT('Origin',(5.600000004205,-9.67863108710757,-17.0348569087084));
#42073=CARTESIAN_POINT('Ctrl Pts',(-5.69266360645557,-9.93047718662622,
-17.3532040955763));
#42074=CARTESIAN_POINT('Ctrl Pts',(-5.65789955297649,-9.91591746177382,
-17.3608556206644));
#42075=CARTESIAN_POINT('Ctrl Pts',(-5.54372467191845,-9.86855446001491,
-17.3857806485202));
#42076=CARTESIAN_POINT('Ctrl Pts',(-5.34116840845335,-9.78714565169692,
-17.4287927186182));
#42077=CARTESIAN_POINT('Ctrl Pts',(-5.07576710977349,-9.68537184202562,
-17.4827626121575));
#42078=CARTESIAN_POINT('Ctrl Pts',(-4.78281267363776,-9.57897699504215,
-17.5393275023324));
#42079=CARTESIAN_POINT('Ctrl Pts',(-4.45929925449841,-9.46872737380591,
-17.5980532014339));
#42080=CARTESIAN_POINT('Ctrl Pts',(-4.10061014601583,-9.35538870497184,
-17.6585174226153));
#42081=CARTESIAN_POINT('Ctrl Pts',(-3.70134367778252,-9.24025425662571,
-17.7200257080785));
#42082=CARTESIAN_POINT('Ctrl Pts',(-3.2566726167652,-9.12574041664841,-17.7812901303106));
#42083=CARTESIAN_POINT('Ctrl Pts',(-2.76260093164982,-9.01549190881541,
-17.8403691196296));
#42084=CARTESIAN_POINT('Ctrl Pts',(-2.21454168295961,-8.91411127568825,
-17.8948066609545));
#42085=CARTESIAN_POINT('Ctrl Pts',(-1.60546929120789,-8.82723526419404,
-17.9415848779543));
#42086=CARTESIAN_POINT('Ctrl Pts',(-0.938933076209208,-8.76363029294198,
-17.9759675605449));
#42087=CARTESIAN_POINT('Ctrl Pts',(-0.236645353180689,-8.73273868672654,
-17.9927933052039));
#42088=CARTESIAN_POINT('Ctrl Pts',(0.464246679174975,-8.7390529531475,-17.989337089631));
#42089=CARTESIAN_POINT('Ctrl Pts',(1.1288813795409,-8.77907936488918,-17.9676027521604));
#42090=CARTESIAN_POINT('Ctrl Pts',(1.73416986111007,-8.84413326189491,-17.9324777156547));
#42091=CARTESIAN_POINT('Ctrl Pts',(2.2738216203696,-8.92486775034786,-17.8890293563113));
#42092=CARTESIAN_POINT('Ctrl Pts',(2.75209716612224,-9.01417698631136,-17.8410792541175));
#42093=CARTESIAN_POINT('Ctrl Pts',(3.17956622796434,-9.10813982684136,-17.7907195797015));
#42094=CARTESIAN_POINT('Ctrl Pts',(3.56235593967422,-9.20363013326605,-17.7396142074167));
#42095=CARTESIAN_POINT('Ctrl Pts',(3.90389825968162,-9.29788912705087,-17.6892297131137));
#42096=CARTESIAN_POINT('Ctrl Pts',(4.20699235675401,-9.388673083866,-17.6407574720575));
#42097=CARTESIAN_POINT('Ctrl Pts',(4.47553242575446,-9.47469414069719,-17.5948792514844));
#42098=CARTESIAN_POINT('Ctrl Pts',(4.71438132197511,-9.55560416869257,-17.5517772747069));
#42099=CARTESIAN_POINT('Ctrl Pts',(4.9283498408451,-9.63159810677658,-17.5113467756739));
#42100=CARTESIAN_POINT('Ctrl Pts',(5.12118003505284,-9.70292908305465,-17.4734546182196));
#42101=CARTESIAN_POINT('Ctrl Pts',(5.29544654742088,-9.76971701115713,-17.4380406162804));
#42102=CARTESIAN_POINT('Ctrl Pts',(5.45302073831863,-9.83201159502866,-17.4050827994527));
#42103=CARTESIAN_POINT('Ctrl Pts',(5.58355273454169,-9.88505636891086,-17.3770948527372));
#42104=CARTESIAN_POINT('Ctrl Pts',(5.66171486335273,-9.91751652281573,-17.3600153922565));
#42105=CARTESIAN_POINT('Ctrl Pts',(5.69263724707086,-9.93047273566079,-17.3532067220467));
#42106=CARTESIAN_POINT('Ctrl Pts',(-5.75649789768048,-9.81445032353156,
-17.4266145045828));
#42107=CARTESIAN_POINT('Ctrl Pts',(-5.72140176441163,-9.79971069472685,
-17.434270380524));
#42108=CARTESIAN_POINT('Ctrl Pts',(-5.60613635739674,-9.75175915352497,
-17.4592038938664));
#42109=CARTESIAN_POINT('Ctrl Pts',(-5.40164108893205,-9.66931698875883,
-17.5021963817961));
#42110=CARTESIAN_POINT('Ctrl Pts',(-5.13366937863353,-9.5661987286677,-17.5560725731441));
#42111=CARTESIAN_POINT('Ctrl Pts',(-4.83782308793672,-9.45834379568037,
-17.6124815425991));
#42112=CARTESIAN_POINT('Ctrl Pts',(-4.51104023762664,-9.34652661601802,
-17.6709975695962));
#42113=CARTESIAN_POINT('Ctrl Pts',(-4.14862925029359,-9.231521531333,-17.7312048309269));
#42114=CARTESIAN_POINT('Ctrl Pts',(-3.74510102845225,-9.11463774454148,
-17.7924129625212));
#42115=CARTESIAN_POINT('Ctrl Pts',(-3.29554242556852,-8.9983253434469,-17.8533379230091));
#42116=CARTESIAN_POINT('Ctrl Pts',(-2.79587913883895,-8.8862850261194,-17.9120433222388));
#42117=CARTESIAN_POINT('Ctrl Pts',(-2.24144276794023,-8.78319658437654,
-17.9660813301617));
#42118=CARTESIAN_POINT('Ctrl Pts',(-1.62510688401195,-8.69479920344606,
-18.0124491340476));
#42119=CARTESIAN_POINT('Ctrl Pts',(-0.950466599383164,-8.63003115288642,
-18.0464583229771));
#42120=CARTESIAN_POINT('Ctrl Pts',(-0.239549742883197,-8.59853868486254,
-18.0630341805028));
#42121=CARTESIAN_POINT('Ctrl Pts',(0.469949066202627,-8.60498016144591,
-18.0596381272223));
#42122=CARTESIAN_POINT('Ctrl Pts',(1.14273524876982,-8.64576713166439,-18.0381916489064));
#42123=CARTESIAN_POINT('Ctrl Pts',(1.75535098855907,-8.71199656223821,-18.0034263284059));
#42124=CARTESIAN_POINT('Ctrl Pts',(2.30141447271848,-8.79413512241296,-17.9603471611883));
#42125=CARTESIAN_POINT('Ctrl Pts',(2.7852478206494,-8.88494571507752,-17.9127462179189));
#42126=CARTESIAN_POINT('Ctrl Pts',(3.21756682194094,-8.98043993881617,-17.8627088342849));
#42127=CARTESIAN_POINT('Ctrl Pts',(3.60459389084317,-9.07744184548594,-17.8118953887759));
#42128=CARTESIAN_POINT('Ctrl Pts',(3.94982589630254,-9.17315216444604,-17.7617698453573));
#42129=CARTESIAN_POINT('Ctrl Pts',(4.25611894261082,-9.26529734916467,-17.7135218257619));
#42130=CARTESIAN_POINT('Ctrl Pts',(4.52743270504629,-9.35257560708462,-17.6678330416736));
#42131=CARTESIAN_POINT('Ctrl Pts',(4.76870079198005,-9.43463882557911,-17.6248868897531));
#42132=CARTESIAN_POINT('Ctrl Pts',(4.98479925044384,-9.51168909397294,-17.5845799209091));
#42133=CARTESIAN_POINT('Ctrl Pts',(5.17952065868517,-9.58398673758781,-17.546779662838));
#42134=CARTESIAN_POINT('Ctrl Pts',(5.35547601555703,-9.65165676751619,-17.5114262531364));
#42135=CARTESIAN_POINT('Ctrl Pts',(5.51456435186126,-9.71475354863065,-17.4784990017821));
#42136=CARTESIAN_POINT('Ctrl Pts',(5.64634486800574,-9.76846611527046,-17.4505151131804));
#42137=CARTESIAN_POINT('Ctrl Pts',(5.72525346100058,-9.80132967332423,-17.4334299861987));
#42138=CARTESIAN_POINT('Ctrl Pts',(5.75647083561349,-9.81444682222214,-17.4266191679546));
#42139=CARTESIAN_POINT('Ctrl Pts',(-5.81361929048237,-9.67439453857855,
-17.423197744291));
#42140=CARTESIAN_POINT('Ctrl Pts',(-5.77819666227631,-9.6595220433756,-17.4308427766472));
#42141=CARTESIAN_POINT('Ctrl Pts',(-5.66186327707103,-9.61114035601224,
-17.4557334262191));
#42142=CARTESIAN_POINT('Ctrl Pts',(-5.45549017818957,-9.52796766887907,
-17.4986076291796));
#42143=CARTESIAN_POINT('Ctrl Pts',(-5.18505475617177,-9.42393970967208,
-17.5522493851993));
#42144=CARTESIAN_POINT('Ctrl Pts',(-4.88646290757818,-9.31512956626903,
-17.6083407394487));
#42145=CARTESIAN_POINT('Ctrl Pts',(-4.55660702638627,-9.2023142636938,-17.6664668945342));
#42146=CARTESIAN_POINT('Ctrl Pts',(-4.1907357518231,-9.08627253772922,-17.7262204199607));
#42147=CARTESIAN_POINT('Ctrl Pts',(-3.78329193485985,-8.96832424820001,
-17.7869172956422));
#42148=CARTESIAN_POINT('Ctrl Pts',(-3.32929912805831,-8.85094208595135,
-17.8472814113126));
#42149=CARTESIAN_POINT('Ctrl Pts',(-2.82462928256113,-8.73786294953229,
-17.9053881650923));
#42150=CARTESIAN_POINT('Ctrl Pts',(-2.2645589068602,-8.63381421728722,-17.9588072543659));
#42151=CARTESIAN_POINT('Ctrl Pts',(-1.64189026832239,-8.54459435107722,
-18.0045638218666));
#42152=CARTESIAN_POINT('Ctrl Pts',(-0.96027229994903,-8.47922974920371,
-18.0380406721874));
#42153=CARTESIAN_POINT('Ctrl Pts',(-0.2420055177134,-8.44745609604986,-18.0542798623764));
#42154=CARTESIAN_POINT('Ctrl Pts',(0.474779168863501,-8.45395382657934,
-18.0509629399101));
#42155=CARTESIAN_POINT('Ctrl Pts',(1.15453262834516,-8.49510983520315,-18.0299118250766));
#42156=CARTESIAN_POINT('Ctrl Pts',(1.77347554169151,-8.56195149369413,-17.9956652267154));
#42157=CARTESIAN_POINT('Ctrl Pts',(2.32514101750424,-8.64485473380872,-17.9531396728781));
#42158=CARTESIAN_POINT('Ctrl Pts',(2.81388750093076,-8.73651098679611,-17.9060805154817));
#42159=CARTESIAN_POINT('Ctrl Pts',(3.25054379785076,-8.832890960607,-17.8565581084493));
#42160=CARTESIAN_POINT('Ctrl Pts',(3.64140302964256,-8.93078680616275,-17.8062235176184));
#42161=CARTESIAN_POINT('Ctrl Pts',(3.99000761178859,-9.02737231548921,-17.7565334831738));
#42162=CARTESIAN_POINT('Ctrl Pts',(4.29925370227988,-9.12035320253652,-17.7086725687123));
#42163=CARTESIAN_POINT('Ctrl Pts',(4.57315108197472,-9.20841675799382,-17.6633210002052));
#42164=CARTESIAN_POINT('Ctrl Pts',(4.81669094399185,-9.29121306576743,-17.6206634780497));
#42165=CARTESIAN_POINT('Ctrl Pts',(5.03480427213376,-9.36894754326617,-17.5805987012757));
#42166=CARTESIAN_POINT('Ctrl Pts',(5.23132679673705,-9.44188448240512,-17.5429955607112));
#42167=CARTESIAN_POINT('Ctrl Pts',(5.40890088264024,-9.51015186167537,-17.5077948859787));
#42168=CARTESIAN_POINT('Ctrl Pts',(5.56945003289077,-9.57380659447015,-17.4749776200002));
#42169=CARTESIAN_POINT('Ctrl Pts',(5.70244415125805,-9.62799710805693,-17.447059588863));
#42170=CARTESIAN_POINT('Ctrl Pts',(5.78208417666968,-9.6611555957235,-17.4300039376));
#42171=CARTESIAN_POINT('Ctrl Pts',(5.81359177729411,-9.67439082761106,-17.4232047915309));
#42172=CARTESIAN_POINT('Ctrl Pts',(-5.84786851508959,-9.55010334349577,
-17.3442496989582));
#42173=CARTESIAN_POINT('Ctrl Pts',(-5.812217479884,-9.5351824724971,-17.3518718310924));
#42174=CARTESIAN_POINT('Ctrl Pts',(-5.69514122735358,-9.4866502579589,-17.3766806339459));
#42175=CARTESIAN_POINT('Ctrl Pts',(-5.48748337876904,-9.4032556173417,-17.4193717913408));
#42176=CARTESIAN_POINT('Ctrl Pts',(-5.21538869253598,-9.29900866034276,
-17.4727054166742));
#42177=CARTESIAN_POINT('Ctrl Pts',(-4.9149750351536,-9.1900167307662,-17.5284081611456));
#42178=CARTESIAN_POINT('Ctrl Pts',(-4.5831125662408,-9.0770531753415,-17.5860755004643));
#42179=CARTESIAN_POINT('Ctrl Pts',(-4.21502210731758,-8.9608956758337,-17.6453079392981));
#42180=CARTESIAN_POINT('Ctrl Pts',(-3.80511703616835,-8.8428664734407,-17.7054282443237));
#42181=CARTESIAN_POINT('Ctrl Pts',(-3.34839805975775,-8.72544340689495,
-17.765170016477));
#42182=CARTESIAN_POINT('Ctrl Pts',(-2.8407230353756,-8.61236962673605,-17.8226236819756));
#42183=CARTESIAN_POINT('Ctrl Pts',(-2.27735525009385,-8.50837707579534,
-17.8753808010097));
#42184=CARTESIAN_POINT('Ctrl Pts',(-1.65107529422485,-8.41926371628257,
-17.9204993862399));
#42185=CARTESIAN_POINT('Ctrl Pts',(-0.965578662885549,-8.3540357348161,
-17.9534365922209));
#42186=CARTESIAN_POINT('Ctrl Pts',(-0.243318637273114,-8.3223788964438,
-17.9693481145899));
#42187=CARTESIAN_POINT('Ctrl Pts',(0.47737188163246,-8.32884628519568,-17.966106785336));
#42188=CARTESIAN_POINT('Ctrl Pts',(1.16093897363205,-8.3698768981194,-17.945446036046));
#42189=CARTESIAN_POINT('Ctrl Pts',(1.78342015349724,-8.43659637874813,-17.9117294849112));
#42190=CARTESIAN_POINT('Ctrl Pts',(2.33829376630727,-8.51941092724095,-17.869784288292));
#42191=CARTESIAN_POINT('Ctrl Pts',(2.82991911139756,-8.61102028452467,-17.8233051831625));
#42192=CARTESIAN_POINT('Ctrl Pts',(3.26917307993139,-8.70739211148768,-17.7743436753537));
#42193=CARTESIAN_POINT('Ctrl Pts',(3.66237499383399,-8.80531353084573,-17.724538365214));
#42194=CARTESIAN_POINT('Ctrl Pts',(4.01308062607134,-8.90195252815353,-17.6753362240971));
#42195=CARTESIAN_POINT('Ctrl Pts',(4.32419802749158,-8.99500899930038,-17.6279149003961));
#42196=CARTESIAN_POINT('Ctrl Pts',(4.59975757560383,-9.08316541187363,-17.5829521313571));
#42197=CARTESIAN_POINT('Ctrl Pts',(4.84477861688869,-9.16606874549135,-17.5406336814741));
#42198=CARTESIAN_POINT('Ctrl Pts',(5.06422123228634,-9.24392299646874,-17.5008606167677));
#42199=CARTESIAN_POINT('Ctrl Pts',(5.26194473312297,-9.31699208235458,-17.4635035011414));
#42200=CARTESIAN_POINT('Ctrl Pts',(5.44060899250946,-9.38540398708525,-17.4285040269477));
#42201=CARTESIAN_POINT('Ctrl Pts',(5.6021518658813,-9.44921534699241,-17.3958446583246));
#42202=CARTESIAN_POINT('Ctrl Pts',(5.73598088935879,-9.50355932364197,-17.3680353568609));
#42203=CARTESIAN_POINT('Ctrl Pts',(5.8161300955248,-9.53682114745297,-17.3510358204143));
#42204=CARTESIAN_POINT('Ctrl Pts',(5.84784092911347,-9.55009832792046,-17.344258799978));
#42205=CARTESIAN_POINT('',(-5.593361696257,-9.87744143006053,-17.3818877156668));
#42206=CARTESIAN_POINT('Ctrl Pts',(-5.593361696257,-9.87744143006053,-17.3818877156668));
#42207=CARTESIAN_POINT('Ctrl Pts',(-5.53987020059952,-9.85545802832816,
-17.3934585468391));
#42208=CARTESIAN_POINT('Ctrl Pts',(-5.4793497262585,-9.83099911672932,-17.4063497946954));
#42209=CARTESIAN_POINT('Ctrl Pts',(-5.37802554672181,-9.79072213244693,
-17.4276237192178));
#42210=CARTESIAN_POINT('Ctrl Pts',(-5.34249357553872,-9.77670562256007,
-17.4350336172399));
#42211=CARTESIAN_POINT('Ctrl Pts',(-5.28655975175779,-9.75487376400626,
-17.4465840985766));
#42212=CARTESIAN_POINT('Ctrl Pts',(-5.25793387311575,-9.74375670971193,
-17.4524678767338));
#42213=CARTESIAN_POINT('Ctrl Pts',(-5.22831954434635,-9.73235856535911,
-17.4585032833399));
#42214=CARTESIAN_POINT('Ctrl Pts',(-5.20835700291623,-9.72470001466014,
-17.4625591244086));
#42215=CARTESIAN_POINT('Ctrl Pts',(-5.19631311250797,-9.72009659507744,
-17.4649974123646));
#42216=CARTESIAN_POINT('Ctrl Pts',(-5.1220799029291,-9.69180540538195,-17.4799839844333));
#42217=CARTESIAN_POINT('Ctrl Pts',(-5.04939710272276,-9.66462085844997,
-17.4943969591114));
#42218=CARTESIAN_POINT('Ctrl Pts',(-4.93032631487558,-9.62113982432037,
-17.5174745985252));
#42219=CARTESIAN_POINT('Ctrl Pts',(-4.86827927406758,-9.59872847149976,
-17.5293749740773));
#42220=CARTESIAN_POINT('Ctrl Pts',(-4.79149567774383,-9.57153828977163,
-17.5438220492272));
#42221=CARTESIAN_POINT('Ctrl Pts',(-4.75200503407002,-9.55770243449621,
-17.5511756151097));
#42222=CARTESIAN_POINT('Ctrl Pts',(-4.73484500560012,-9.55172343097645,
-17.5543538058097));
#42223=CARTESIAN_POINT('Ctrl Pts',(-4.72335266064343,-9.54772672077564,
-17.556478385714));
#42224=CARTESIAN_POINT('Ctrl Pts',(-4.71643686245652,-9.54532685037244,
-17.5577541794684));
#42225=CARTESIAN_POINT('Ctrl Pts',(-4.56282068320413,-9.49210542227198,
-17.5860482166363));
#42226=CARTESIAN_POINT('Ctrl Pts',(-4.386889093463,-9.43374884345433,-17.6171019560031));
#42227=CARTESIAN_POINT('Ctrl Pts',(-4.08253603951581,-9.34005104916093,
-17.6670294778133));
#42228=CARTESIAN_POINT('Ctrl Pts',(-3.97434240997751,-9.30782386068614,
-17.6842115349644));
#42229=CARTESIAN_POINT('Ctrl Pts',(-3.80193804833617,-9.25876183240516,
-17.7103833193709));
#42230=CARTESIAN_POINT('Ctrl Pts',(-3.71320738818203,-9.23405323476083,
-17.7235674303112));
#42231=CARTESIAN_POINT('Ctrl Pts',(-3.6052634458353,-9.20511170082965,-17.7390166073284));
#42232=CARTESIAN_POINT('Ctrl Pts',(-3.55018526495355,-9.1906386182531,-17.7467441290376));
#42233=CARTESIAN_POINT('Ctrl Pts',(-3.52634328535243,-9.18443823905463,
-17.7500550341078));
#42234=CARTESIAN_POINT('Ctrl Pts',(-3.51039595563223,-9.18030550310546,
-17.7522619351916));
#42235=CARTESIAN_POINT('Ctrl Pts',(-3.50119799341605,-9.17793129863342,
-17.7535298272406));
#42236=CARTESIAN_POINT('Ctrl Pts',(-3.27586137147083,-9.11994720365643,
-17.7844960252267));
#42237=CARTESIAN_POINT('Ctrl Pts',(-3.02941181880873,-9.06174272207816,
-17.8156123473834));
#42238=CARTESIAN_POINT('Ctrl Pts',(-2.61782552001545,-8.97815820474398,
-17.860360920498));
#42239=CARTESIAN_POINT('Ctrl Pts',(-2.47364475878434,-8.95093882646814,
-17.8749443867086));
#42240=CARTESIAN_POINT('Ctrl Pts',(-2.24689562448764,-8.91208544364912,
-17.8957798174269));
#42241=CARTESIAN_POINT('Ctrl Pts',(-2.16956624764707,-8.89946471526788,
-17.9025510545595));
#42242=CARTESIAN_POINT('Ctrl Pts',(-2.01141482981592,-8.87506515653167,
-17.915648697891));
#42243=CARTESIAN_POINT('Ctrl Pts',(-1.93261264225071,-8.86356189842033,
-17.9218270113));
#42244=CARTESIAN_POINT('Ctrl Pts',(-1.50967150979595,-8.80586566263095,
-17.9528342587281));
#42245=CARTESIAN_POINT('Ctrl Pts',(-1.1550619741231,-8.76998362984971,-17.9721822696362));
#42246=CARTESIAN_POINT('Ctrl Pts',(-0.598762726050275,-8.73779219664723,
-17.9896029650133));
#42247=CARTESIAN_POINT('Ctrl Pts',(-0.409265485932076,-8.73066302435934,
-17.9934771411258));
#42248=CARTESIAN_POINT('Ctrl Pts',(-0.118923389613889,-8.72608300745925,
-17.9959714712881));
#42249=CARTESIAN_POINT('Ctrl Pts',(-0.0211266514843454,-8.72557448984061,
-17.9962498255603));
#42250=CARTESIAN_POINT('Ctrl Pts',(0.127092514745191,-8.72642220893752,
-17.9957877679624));
#42251=CARTESIAN_POINT('Ctrl Pts',(0.201583112618764,-8.72724880515296,
-17.9953371969745));
#42252=CARTESIAN_POINT('Ctrl Pts',(0.276645232630548,-8.72869526217384,
-17.9945496438171));
#42253=CARTESIAN_POINT('Ctrl Pts',(0.326813650891338,-8.72979901612804,
-17.9939488896616));
#42254=CARTESIAN_POINT('Ctrl Pts',(0.353716444626081,-8.73046880560203,
-17.9935844415831));
#42255=CARTESIAN_POINT('Ctrl Pts',(0.752470687018729,-8.74141659322514,
-17.9876293438515));
#42256=CARTESIAN_POINT('Ctrl Pts',(1.10888528675477,-8.76680638628075,-17.9738803725204));
#42257=CARTESIAN_POINT('Ctrl Pts',(1.61518192023207,-8.82097298245935,-17.9447112956001));
#42258=CARTESIAN_POINT('Ctrl Pts',(1.86124892043903,-8.85206972094614,-17.9279894068043));
#42259=CARTESIAN_POINT('Ctrl Pts',(2.13593478341671,-8.89391687546287,-17.9055257982567));
#42260=CARTESIAN_POINT('Ctrl Pts',(2.25100180242205,-8.91289053503451,-17.8953477722513));
#42261=CARTESIAN_POINT('Ctrl Pts',(2.32712303871463,-8.92575366186556,-17.8884490984369));
#42262=CARTESIAN_POINT('Ctrl Pts',(2.36664298290315,-8.93260298069073,-17.8847765119233));
#42263=CARTESIAN_POINT('Ctrl Pts',(2.68808813074154,-8.98954074940645,-17.8542525016971));
#42264=CARTESIAN_POINT('Ctrl Pts',(2.94934760460972,-9.04481782758675,-17.8246684230021));
#42265=CARTESIAN_POINT('Ctrl Pts',(3.30453249576307,-9.12819298700539,-17.7800978521836));
#42266=CARTESIAN_POINT('Ctrl Pts',(3.4168100728727,-9.15607565928406,-17.76520089681));
#42267=CARTESIAN_POINT('Ctrl Pts',(3.57605035862492,-9.19736314467759,-17.743153243358));
#42268=CARTESIAN_POINT('Ctrl Pts',(3.65337648152297,-9.21787438116161,-17.7322029881789));
#42269=CARTESIAN_POINT('Ctrl Pts',(3.7395757566091,-9.2414428236852,-17.7196251323142));
#42270=CARTESIAN_POINT('Ctrl Pts',(3.77565804558281,-9.25145346321499,-17.7142836508181));
#42271=CARTESIAN_POINT('Ctrl Pts',(3.79952173656711,-9.25810581892405,-17.7107342865122));
#42272=CARTESIAN_POINT('Ctrl Pts',(3.80961452997646,-9.26093063959662,-17.7092271754704));
#42273=CARTESIAN_POINT('Ctrl Pts',(4.03884499629718,-9.32544138467622,-17.6748113705168));
#42274=CARTESIAN_POINT('Ctrl Pts',(4.2328456349755,-9.38529250399132,-17.6429130577065));
#42275=CARTESIAN_POINT('Ctrl Pts',(4.49122806914593,-9.46901622821037,-17.5983382779601));
#42276=CARTESIAN_POINT('Ctrl Pts',(4.57191912656156,-9.4959353918958,-17.5840150142378));
#42277=CARTESIAN_POINT('Ctrl Pts',(4.68480108172324,-9.53443167111024,-17.5635439200051));
#42278=CARTESIAN_POINT('Ctrl Pts',(4.73920340156364,-9.55321133941474,-17.553560636219));
#42279=CARTESIAN_POINT('Ctrl Pts',(4.799105123665,-9.5742369214802,-17.5423882028615));
#42280=CARTESIAN_POINT('Ctrl Pts',(4.82401279362721,-9.58305308212916,-17.5377044547403));
#42281=CARTESIAN_POINT('Ctrl Pts',(4.8404480187903,-9.58888667848674,-17.5346054413657));
#42282=CARTESIAN_POINT('Ctrl Pts',(4.84692845456482,-9.59119177450282,-17.5333809517617));
#42283=CARTESIAN_POINT('Ctrl Pts',(4.93422806910404,-9.62235399167718,-17.5168284776004));
#42284=CARTESIAN_POINT('Ctrl Pts',(5.00665608387182,-9.64889059416907,-17.5027432111989));
#42285=CARTESIAN_POINT('Ctrl Pts',(5.10754064212285,-9.68649972701724,-17.4827987196256));
#42286=CARTESIAN_POINT('Ctrl Pts',(5.15604355527322,-9.70475862742077,-17.4731205210468));
#42287=CARTESIAN_POINT('Ctrl Pts',(5.20923639682545,-9.72504279169127,-17.4623766520456));
#42288=CARTESIAN_POINT('Ctrl Pts',(5.23130606667859,-9.73351349340259,-17.4578915977158));
#42289=CARTESIAN_POINT('Ctrl Pts',(5.24585756608274,-9.73911075894413,-17.4549283108024));
#42290=CARTESIAN_POINT('Ctrl Pts',(5.25198965447703,-9.74147381272326,-17.4536773941826));
#42291=CARTESIAN_POINT('Ctrl Pts',(5.39099848894759,-9.79518047740564,-17.4252507494902));
#42292=CARTESIAN_POINT('Ctrl Pts',(5.50206350613277,-9.83992060849029,-17.4016365743076));
#42293=CARTESIAN_POINT('Ctrl Pts',(5.593361696298,-9.877441429835,-17.3818877156174));
#42294=CARTESIAN_POINT('',(-5.73644346265596,-9.5212176560943,-17.3763289909634));
#42295=CARTESIAN_POINT('Origin',(-5.599999999997,-9.6786310860259,-17.0348569100619));
#42296=CARTESIAN_POINT('Ctrl Pts',(-5.73644387762363,-9.52121721553821,
-17.3763301032151));
#42297=CARTESIAN_POINT('Ctrl Pts',(-5.73644352459376,-9.52121707146375,
-17.3763301778592));
#42298=CARTESIAN_POINT('Ctrl Pts',(-5.73644317156365,-9.5212169273892,-17.3763302525035));
#42299=CARTESIAN_POINT('Ctrl Pts',(-5.73644281853329,-9.52121678331457,
-17.3763303271477));
#42300=CARTESIAN_POINT('Ctrl Pts',(-5.67992322178403,-9.49815066425739,
-17.3882807538312));
#42301=CARTESIAN_POINT('Ctrl Pts',(-5.61717095064414,-9.47290942008161,
-17.4013891368914));
#42302=CARTESIAN_POINT('Ctrl Pts',(-5.54808342727774,-9.44569918314702,
-17.4155436022901));
#42303=CARTESIAN_POINT('Ctrl Pts',(-5.52951990676316,-9.43838790946215,
-17.4193468462913));
#42304=CARTESIAN_POINT('Ctrl Pts',(-5.51049890446277,-9.43093469419091,
-17.4232254429296));
#42305=CARTESIAN_POINT('Ctrl Pts',(-5.49101823035263,-9.42334400648704,
-17.4271768288267));
#42306=CARTESIAN_POINT('Ctrl Pts',(-5.42195695327852,-9.39643412730443,
-17.4411849557898));
#42307=CARTESIAN_POINT('Ctrl Pts',(-5.34711974638812,-9.36779313739751,
-17.4561096755892));
#42308=CARTESIAN_POINT('Ctrl Pts',(-5.26639706158773,-9.33765672401009,
-17.4718271439572));
#42309=CARTESIAN_POINT('Ctrl Pts',(-5.2508485049638,-9.33185194024757,-17.4748545946361));
#42310=CARTESIAN_POINT('Ctrl Pts',(-5.2350815454412,-9.32599180437578,-17.4779113854455));
#42311=CARTESIAN_POINT('Ctrl Pts',(-5.21909533755791,-9.32007818972099,
-17.4809965265211));
#42312=CARTESIAN_POINT('Ctrl Pts',(-5.19132317678243,-9.30980471785349,
-17.4863562112312));
#42313=CARTESIAN_POINT('Ctrl Pts',(-5.16288931838467,-9.29936980768925,
-17.4918014763877));
#42314=CARTESIAN_POINT('Ctrl Pts',(-5.1337892851941,-9.2887838855698,-17.4973269203456));
#42315=CARTESIAN_POINT('Ctrl Pts',(-5.06602551715808,-9.26413298684911,
-17.5101937408131));
#42316=CARTESIAN_POINT('Ctrl Pts',(-4.99464963484642,-9.2386618869589,-17.5234960128167));
#42317=CARTESIAN_POINT('Ctrl Pts',(-4.91960196681596,-9.21251576379739,
-17.5371586424099));
#42318=CARTESIAN_POINT('Ctrl Pts',(-4.82891093158763,-9.18091959247115,
-17.5536691890301));
#42319=CARTESIAN_POINT('Ctrl Pts',(-4.73285787026604,-9.14833624523932,
-17.5707066532315));
#42320=CARTESIAN_POINT('Ctrl Pts',(-4.63133262667696,-9.11506274518776,
-17.588118684881));
#42321=CARTESIAN_POINT('Ctrl Pts',(-4.61738479820793,-9.11049153654174,
-17.5905107996119));
#42322=CARTESIAN_POINT('Ctrl Pts',(-4.6033336778579,-9.10590737359808,-17.5929099483661));
#42323=CARTESIAN_POINT('Ctrl Pts',(-4.58917897115216,-9.10131109609215,
-17.5953157015978));
#42324=CARTESIAN_POINT('Ctrl Pts',(-4.5569989063018,-9.09086167377023,-17.6007850692521));
#42325=CARTESIAN_POINT('Ctrl Pts',(-4.52428344765957,-9.08034960451572,
-17.6062885885683));
#42326=CARTESIAN_POINT('Ctrl Pts',(-4.49102921165013,-9.06978507926774,
-17.6118210417931));
#42327=CARTESIAN_POINT('Ctrl Pts',(-4.45061973879662,-9.05694740962175,
-17.6185439001483));
#42328=CARTESIAN_POINT('Ctrl Pts',(-4.40941469034533,-9.04403225153753,
-17.6253094982539));
#42329=CARTESIAN_POINT('Ctrl Pts',(-4.36740794739292,-9.03105885241992,
-17.6321080004935));
#42330=CARTESIAN_POINT('Ctrl Pts',(-4.34640457591672,-9.02457215286112,
-17.6355072516133));
#42331=CARTESIAN_POINT('Ctrl Pts',(-4.32520077691195,-9.01807089922343,
-17.6389147163269));
#42332=CARTESIAN_POINT('Ctrl Pts',(-4.30379578562449,-9.01155761129438,
-17.6423291198216));
#42333=CARTESIAN_POINT('Ctrl Pts',(-4.29309328998076,-9.00830096732986,
-17.644036321569));
#42334=CARTESIAN_POINT('Ctrl Pts',(-4.28234049601323,-9.00504131518672,
-17.6457452572156));
#42335=CARTESIAN_POINT('Ctrl Pts',(-4.2715373074274,-9.00177897451451,-17.6474557634699));
#42336=CARTESIAN_POINT('Ctrl Pts',(-4.26343491598802,-8.99933221901035,
-17.6487386431606));
#42337=CARTESIAN_POINT('Ctrl Pts',(-4.25530417755542,-8.9968839512415,-17.650022406252));
#42338=CARTESIAN_POINT('Ctrl Pts',(-4.24714505143305,-8.99443430757621,
-17.6513069830186));
#42339=CARTESIAN_POINT('Ctrl Pts',(-4.2444253427256,-8.99361775968778,-17.6517351752741));
#42340=CARTESIAN_POINT('Ctrl Pts',(-4.24040571702055,-8.99241248537787,
-17.6523672331073));
#42341=CARTESIAN_POINT('Ctrl Pts',(-4.23897646125202,-8.99198421043807,
-17.6525918284096));
#42342=CARTESIAN_POINT('Ctrl Pts',(-4.23363824301308,-8.99038461913656,
-17.6534306836833));
#42343=CARTESIAN_POINT('Ctrl Pts',(-4.22827574141105,-8.98878076076398,
-17.6542717650764));
#42344=CARTESIAN_POINT('Ctrl Pts',(-4.22288893012927,-8.98717271128015,
-17.6551150336142));
#42345=CARTESIAN_POINT('Ctrl Pts',(-4.1421074038801,-8.96305813128221,-17.6677608301641));
#42346=CARTESIAN_POINT('Ctrl Pts',(-4.05585939228501,-8.93799731004626,
-17.6809003637884));
#42347=CARTESIAN_POINT('Ctrl Pts',(-3.96405498682432,-8.91226963547649,
-17.6943903142864));
#42348=CARTESIAN_POINT('Ctrl Pts',(-3.91582486924293,-8.89875341298838,
-17.7014773586981));
#42349=CARTESIAN_POINT('Ctrl Pts',(-3.86606110337935,-8.88505388292564,
-17.7086607422642));
#42350=CARTESIAN_POINT('Ctrl Pts',(-3.81475024026647,-8.87121673240609,
-17.7159170732943));
#42351=CARTESIAN_POINT('Ctrl Pts',(-3.71991894440022,-8.84564329950596,
-17.7293280204715));
#42352=CARTESIAN_POINT('Ctrl Pts',(-3.61980302978308,-8.81959708984185,
-17.7429895018292));
#42353=CARTESIAN_POINT('Ctrl Pts',(-3.51432006484776,-8.79339955531239,
-17.7567370276897));
#42354=CARTESIAN_POINT('Ctrl Pts',(-3.46379569220283,-8.78085142493175,
-17.7633218361462));
#42355=CARTESIAN_POINT('Ctrl Pts',(-3.41204000915956,-8.76826924284194,
-17.7699260492204));
#42356=CARTESIAN_POINT('Ctrl Pts',(-3.35904414021376,-8.7556921475468,-17.7765296682036));
#42357=CARTESIAN_POINT('Ctrl Pts',(-3.24837094384221,-8.72942694301161,
-17.7903202453758));
#42358=CARTESIAN_POINT('Ctrl Pts',(-3.13228850732444,-8.70318068816256,
-17.8041098612256));
#42359=CARTESIAN_POINT('Ctrl Pts',(-3.01072520053139,-8.67734385271493,
-17.8176991668407));
#42360=CARTESIAN_POINT('Ctrl Pts',(-2.96856983178144,-8.66838423032262,
-17.8224116265818));
#42361=CARTESIAN_POINT('Ctrl Pts',(-2.92501766724462,-8.65932141386993,
-17.8271801970784));
#42362=CARTESIAN_POINT('Ctrl Pts',(-2.88136984601049,-8.65044680338113,
-17.8318519114778));
#42363=CARTESIAN_POINT('Ctrl Pts',(-2.87181233466587,-8.64850354050964,
-17.8328748712066));
#42364=CARTESIAN_POINT('Ctrl Pts',(-2.8622502854179,-8.64656913044084,-17.8338932746767));
#42365=CARTESIAN_POINT('Ctrl Pts',(-2.85269744002281,-8.64464634075612,
-17.8349056654296));
#42366=CARTESIAN_POINT('Ctrl Pts',(-2.83187074814701,-8.64045435955582,
-17.837112835063));
#42367=CARTESIAN_POINT('Ctrl Pts',(-2.81108776255884,-8.63631776879051,
-17.8392913449678));
#42368=CARTESIAN_POINT('Ctrl Pts',(-2.79049137152155,-8.63226346828058,
-17.84142701391));
#42369=CARTESIAN_POINT('Ctrl Pts',(-2.61969812019133,-8.59864363824783,
-17.8591368079095));
#42370=CARTESIAN_POINT('Ctrl Pts',(-2.45356650983542,-8.56904343577165,
-17.874747333849));
#42371=CARTESIAN_POINT('Ctrl Pts',(-2.29233862838001,-8.54299950336389,
-17.8884979961909));
#42372=CARTESIAN_POINT('Ctrl Pts',(-2.12998975602917,-8.51677449178518,
-17.9023442646225));
#42373=CARTESIAN_POINT('Ctrl Pts',(-1.97261304668375,-8.49415449375703,
-17.914305181698));
#42374=CARTESIAN_POINT('Ctrl Pts',(-1.82041653590442,-8.47465675411815,
-17.9246298556848));
#42375=CARTESIAN_POINT('Ctrl Pts',(-1.76985269925734,-8.46817907261915,
-17.9280599943012));
#42376=CARTESIAN_POINT('Ctrl Pts',(-1.71986020669752,-8.46204609989298,
-17.9313094777006));
#42377=CARTESIAN_POINT('Ctrl Pts',(-1.67044548275205,-8.45624043232021,
-17.9343872621625));
#42378=CARTESIAN_POINT('Ctrl Pts',(-1.52120350532392,-8.43870619880296,
-17.9436827636348));
#42379=CARTESIAN_POINT('Ctrl Pts',(-1.37723518824579,-8.4241556847917,-17.9514131060398));
#42380=CARTESIAN_POINT('Ctrl Pts',(-1.23869615121725,-8.4121078471322,-17.957825540084));
#42381=CARTESIAN_POINT('Ctrl Pts',(-1.14905169330374,-8.40431205253755,
-17.9619748339301));
#42382=CARTESIAN_POINT('Ctrl Pts',(-1.0616794722232,-8.39756458386839,-17.965572065017));
#42383=CARTESIAN_POINT('Ctrl Pts',(-0.976611993948442,-8.39174067995234,
-17.9686811741687));
#42384=CARTESIAN_POINT('Ctrl Pts',(-0.844717368027886,-8.38271088802736,
-17.9735017565679));
#42385=CARTESIAN_POINT('Ctrl Pts',(-0.718364973239535,-8.37589936903327,
-17.9771500149081));
#42386=CARTESIAN_POINT('Ctrl Pts',(-0.59764893798114,-8.37085523792009,
-17.9798579747241));
#42387=CARTESIAN_POINT('Ctrl Pts',(-0.480950252688124,-8.36597897216058,
-17.982475815425));
#42388=CARTESIAN_POINT('Ctrl Pts',(-0.369518419027349,-8.36275450372224,
-17.9842148255809));
#42389=CARTESIAN_POINT('Ctrl Pts',(-0.263409254252512,-8.36080591599256,
-17.9852673126018));
#42390=CARTESIAN_POINT('Ctrl Pts',(-0.255798643619334,-8.36066615480862,
-17.9853428015469));
#42391=CARTESIAN_POINT('Ctrl Pts',(-0.248215404147646,-8.36053297076181,
-17.9854147514066));
#42392=CARTESIAN_POINT('Ctrl Pts',(-0.24065955159746,-8.36040623146302,
-17.9854832297331));
#42393=CARTESIAN_POINT('Ctrl Pts',(-0.202148468472625,-8.35976025966322,
-17.9858322538181));
#42394=CARTESIAN_POINT('Ctrl Pts',(-0.164348870767216,-8.35928165386147,
-17.9860911216831));
#42395=CARTESIAN_POINT('Ctrl Pts',(-0.127262571736914,-8.3589527956832,
-17.9862686945712));
#42396=CARTESIAN_POINT('Ctrl Pts',(-0.10508126686014,-8.35875610570053,
-17.9863749008649));
#42397=CARTESIAN_POINT('Ctrl Pts',(-0.0831551306878216,-8.35861298799412,
-17.9864520145469));
#42398=CARTESIAN_POINT('Ctrl Pts',(-0.0614844712836392,-8.35851980347556,
-17.9865018816466));
#42399=CARTESIAN_POINT('Ctrl Pts',(-0.0416881557408339,-8.35843467869469,
-17.9865474356291));
#42400=CARTESIAN_POINT('Ctrl Pts',(-0.0231003214238363,-8.35839184303637,
-17.9865699936198));
#42401=CARTESIAN_POINT('Ctrl Pts',(-0.00299359736550399,-8.35838676981635,
-17.9865716737415));
#42402=CARTESIAN_POINT('Ctrl Pts',(-0.00108986357576685,-8.35838628947652,
-17.9865718328179));
#42403=CARTESIAN_POINT('Ctrl Pts',(0.000827486450446617,-8.35838618200386,
-17.9865717873868));
#42404=CARTESIAN_POINT('Ctrl Pts',(0.00276076763039516,-8.35838646560832,
-17.9865715281069));
#42405=CARTESIAN_POINT('Ctrl Pts',(0.115380446224821,-8.35840298645552,
-17.9865564242466));
#42406=CARTESIAN_POINT('Ctrl Pts',(0.233554097747699,-8.35974063747125,
-17.9858249645334));
#42407=CARTESIAN_POINT('Ctrl Pts',(0.357227596823177,-8.36282142206872,
-17.9841629399821));
#42408=CARTESIAN_POINT('Ctrl Pts',(0.400683622266197,-8.36390393897698,
-17.9835789427497));
#42409=CARTESIAN_POINT('Ctrl Pts',(0.444818436323151,-8.3652020196244,-17.9828798738739));
#42410=CARTESIAN_POINT('Ctrl Pts',(0.489628808808967,-8.36673509448657,
-17.9820558604452));
#42411=CARTESIAN_POINT('Ctrl Pts',(0.616894594461688,-8.37108917515977,
-17.9797155827246));
#42412=CARTESIAN_POINT('Ctrl Pts',(0.749612285280078,-8.37733668062018,
-17.9763686556394));
#42413=CARTESIAN_POINT('Ctrl Pts',(0.887682926937973,-8.38593002473395,
-17.9717825956685));
#42414=CARTESIAN_POINT('Ctrl Pts',(0.982201843108898,-8.39181276390401,
-17.968643120015));
#42415=CARTESIAN_POINT('Ctrl Pts',(1.0792286356825,-8.3987954762465,-17.9649225955862));
#42416=CARTESIAN_POINT('Ctrl Pts',(1.17872050964713,-8.40703101254687,-17.9605420742837));
#42417=CARTESIAN_POINT('Ctrl Pts',(1.32351032771627,-8.41901613007574,-17.9541671327216));
#42418=CARTESIAN_POINT('Ctrl Pts',(1.47352296203192,-8.43365408126441,-17.9463946600187));
#42419=CARTESIAN_POINT('Ctrl Pts',(1.62859653155586,-8.45142072464075,-17.9369799815677));
#42420=CARTESIAN_POINT('Ctrl Pts',(1.68654895885756,-8.45806028360508,-17.9334616291485));
#42421=CARTESIAN_POINT('Ctrl Pts',(1.74520772260452,-8.46513697481412,-17.9297138252413));
#42422=CARTESIAN_POINT('Ctrl Pts',(1.80456261858381,-8.47267625227983,-17.9257234471777));
#42423=CARTESIAN_POINT('Ctrl Pts',(1.96229923096924,-8.49271200615751,-17.9151189518365));
#42424=CARTESIAN_POINT('Ctrl Pts',(2.1249558097838,-8.51601437137955,-17.9028015591113));
#42425=CARTESIAN_POINT('Ctrl Pts',(2.29231728498669,-8.54305160629487,-17.8885294728786));
#42426=CARTESIAN_POINT('Ctrl Pts',(2.31269526918793,-8.54634366825407,-17.8867916993114));
#42427=CARTESIAN_POINT('Ctrl Pts',(2.33314294299478,-8.54969110847641,-17.885024941533));
#42428=CARTESIAN_POINT('Ctrl Pts',(2.35365986452972,-8.55309477709375,-17.8832287594278));
#42429=CARTESIAN_POINT('Ctrl Pts',(2.36243866304189,-8.55455114182873,-17.8824602074417));
#42430=CARTESIAN_POINT('Ctrl Pts',(2.37123013941515,-8.55601780098565,-17.8816862683799));
#42431=CARTESIAN_POINT('Ctrl Pts',(2.38003426028352,-8.5574948191759,-17.8809069088695));
#42432=CARTESIAN_POINT('Ctrl Pts',(2.44797134508464,-8.56889224448885,-17.8748929735834));
#42433=CARTESIAN_POINT('Ctrl Pts',(2.51666145215479,-8.58090650166341,-17.8685562781695));
#42434=CARTESIAN_POINT('Ctrl Pts',(2.58608847376924,-8.59356722554678,-17.8618815018982));
#42435=CARTESIAN_POINT('Ctrl Pts',(2.62080198457646,-8.59989758748846,-17.8585441137625));
#42436=CARTESIAN_POINT('Ctrl Pts',(2.6556997235816,-8.60638956729783,-17.8551222031688));
#42437=CARTESIAN_POINT('Ctrl Pts',(2.69077952127531,-8.61304685414928,-17.851613861692));
#42438=CARTESIAN_POINT('Ctrl Pts',(2.70831942012216,-8.61637549757501,-17.8498596909536));
#42439=CARTESIAN_POINT('Ctrl Pts',(2.72590483362213,-8.61974546781656,-17.8480839123907));
#42440=CARTESIAN_POINT('Ctrl Pts',(2.74353548531567,-8.62315722542768,-17.8462862873725));
#42441=CARTESIAN_POINT('Ctrl Pts',(2.75886023088542,-8.62612276057889,-17.844723773036));
#42442=CARTESIAN_POINT('Ctrl Pts',(2.77563789148753,-8.62939846974932,-17.8429979696744));
#42443=CARTESIAN_POINT('Ctrl Pts',(2.79016868445501,-8.63225838463787,-17.8414913638725));
#42444=CARTESIAN_POINT('Ctrl Pts',(2.79235512496293,-8.63268871447435,-17.8412646657176));
#42445=CARTESIAN_POINT('Ctrl Pts',(2.79449071610734,-8.63310954567438,-17.8410429737587));
#42446=CARTESIAN_POINT('Ctrl Pts',(2.79656287567783,-8.63351832069494,-17.8408276342317));
#42447=CARTESIAN_POINT('Ctrl Pts',(2.81155194711914,-8.63647521555661,-17.8392699648313));
#42448=CARTESIAN_POINT('Ctrl Pts',(2.82653495592412,-8.6394549709341,-17.8377005599592));
#42449=CARTESIAN_POINT('Ctrl Pts',(2.84151182039781,-8.64245751452065,-17.8361194547485));
#42450=CARTESIAN_POINT('Ctrl Pts',(2.98776197925397,-8.67177756861319,-17.8206798486395));
#42451=CARTESIAN_POINT('Ctrl Pts',(3.13342623719005,-8.70327062452146,-17.8041245447627));
#42452=CARTESIAN_POINT('Ctrl Pts',(3.27843755206495,-8.73686228895337,-17.7864898983305));
#42453=CARTESIAN_POINT('Ctrl Pts',(3.40982752547695,-8.76729858904749,-17.7705117263661));
#42454=CARTESIAN_POINT('Ctrl Pts',(3.54068146009692,-8.7994577580664,-17.7536474595275));
#42455=CARTESIAN_POINT('Ctrl Pts',(3.67095575806953,-8.83328068790664,-17.7359259293636));
#42456=CARTESIAN_POINT('Ctrl Pts',(3.7881302786502,-8.86370254126023,-17.7199863938356));
#42457=CARTESIAN_POINT('Ctrl Pts',(3.90483587259101,-8.89547037835598,-17.7033533317629));
#42458=CARTESIAN_POINT('Ctrl Pts',(4.02104510452003,-8.92853923906793,-17.6860484800191));
#42459=CARTESIAN_POINT('Ctrl Pts',(4.12468783508762,-8.95803213704215,-17.6706149205934));
#42460=CARTESIAN_POINT('Ctrl Pts',(4.22793574925146,-8.9885598949597,-17.6546470065895));
#42461=CARTESIAN_POINT('Ctrl Pts',(4.33077217729926,-9.0200896656201,-17.6381603930781));
#42462=CARTESIAN_POINT('Ctrl Pts',(4.42240217237626,-9.04818353065642,-17.6234703815367));
#42463=CARTESIAN_POINT('Ctrl Pts',(4.51370547671078,-9.07707292191899,-17.6083685600615));
#42464=CARTESIAN_POINT('Ctrl Pts',(4.60467210495441,-9.1067341689929,-17.5928660142161));
#42465=CARTESIAN_POINT('Ctrl Pts',(4.68609298329243,-9.13328285872658,-17.5789902564401));
#42466=CARTESIAN_POINT('Ctrl Pts',(4.76724413733699,-9.16044991128749,-17.5647934634993));
#42467=CARTESIAN_POINT('Ctrl Pts',(4.84811962989529,-9.18821823686332,-17.550283531101));
#42468=CARTESIAN_POINT('Ctrl Pts',(4.92104264857972,-9.213256107555,-17.5372003579677));
#42469=CARTESIAN_POINT('Ctrl Pts',(4.99374155163286,-9.23878281838882,-17.5238625999774));
#42470=CARTESIAN_POINT('Ctrl Pts',(5.06621286141821,-9.26478600954632,-17.510276029362));
#42471=CARTESIAN_POINT('Ctrl Pts',(5.13211260416723,-9.28843127845354,-17.497921464348));
#42472=CARTESIAN_POINT('Ctrl Pts',(5.19782415727064,-9.31247053252497,-17.4853611648872));
#42473=CARTESIAN_POINT('Ctrl Pts',(5.26334554178665,-9.33689503275619,-17.4725995993014));
#42474=CARTESIAN_POINT('Ctrl Pts',(5.32292696859615,-9.35910528645634,-17.4609949561526));
#42475=CARTESIAN_POINT('Ctrl Pts',(5.38235114343648,-9.38163410200066,-17.4492238850272));
#42476=CARTESIAN_POINT('Ctrl Pts',(5.44161694958957,-9.40447611389181,-17.4372902012635));
#42477=CARTESIAN_POINT('Ctrl Pts',(5.49538378457564,-9.42519873227531,-17.4264637830074));
#42478=CARTESIAN_POINT('Ctrl Pts',(5.54902027517795,-9.44617912364355,-17.4155035276484));
#42479=CARTESIAN_POINT('Ctrl Pts',(5.60252556054591,-9.46741559848347,-17.4044133515384));
#42480=CARTESIAN_POINT('Ctrl Pts',(5.64725681504284,-9.48516962323354,-17.3951417910453));
#42481=CARTESIAN_POINT('Ctrl Pts',(5.69189636725116,-9.50310263122264,-17.3857794246311));
#42482=CARTESIAN_POINT('Ctrl Pts',(5.736442763711,-9.52121697643775,-17.3763304371651));
#42483=CARTESIAN_POINT('Ctrl Pts',(-5.843530256076,-9.74782193877526,-17.4349067568258));
#42484=CARTESIAN_POINT('Ctrl Pts',(-3.895686837384,-8.92798470939806,-17.8601636858557));
#42485=CARTESIAN_POINT('Ctrl Pts',(0.0001633689307963,-8.10806560616921,
-18.2855103771765));
#42486=CARTESIAN_POINT('Ctrl Pts',(3.896013575246,-8.92805347740346,-17.8601280113164));
#42487=CARTESIAN_POINT('Ctrl Pts',(5.844020362869,-9.74802823084197,-17.4347997512851));
#42488=CARTESIAN_POINT('Ctrl Pts',(-5.843530256076,-8.93341761899431,-17.0810054062716));
#42489=CARTESIAN_POINT('Ctrl Pts',(-3.895686837384,-8.18554673507222,-17.4915920272974));
#42490=CARTESIAN_POINT('Ctrl Pts',(0.0001633689307963,-7.43613495951606,
-17.9044826847225));
#42491=CARTESIAN_POINT('Ctrl Pts',(3.896013575246,-8.1856095895101,-17.4915573974575));
#42492=CARTESIAN_POINT('Ctrl Pts',(5.844020362869,-8.93360580246804,-17.0809020921739));
#42493=CARTESIAN_POINT('Ctrl Pts',(-5.843530256076,-7.38850509491984,-16.1560629985976));
#42494=CARTESIAN_POINT('Ctrl Pts',(-3.895686837384,-6.77499150312524,-16.5818456797104));
#42495=CARTESIAN_POINT('Ctrl Pts',(0.0001633689307963,-6.16225640987013,
-17.0065480644992));
#42496=CARTESIAN_POINT('Ctrl Pts',(3.896013575246,-6.77504289425523,-16.5818100592022));
#42497=CARTESIAN_POINT('Ctrl Pts',(5.844020362869,-7.38865947067571,-16.1559558607449));
#42498=CARTESIAN_POINT('Ctrl Pts',(-5.843530256076,-5.5035950496103,-14.2139340091191));
#42499=CARTESIAN_POINT('Ctrl Pts',(-3.895686837384,-5.02273055192306,-14.7660279927807));
#42500=CARTESIAN_POINT('Ctrl Pts',(0.0001633689307963,-4.54131578037147,
-15.3185227509534));
#42501=CARTESIAN_POINT('Ctrl Pts',(3.896013575246,-5.02277092898996,-14.7659816541094));
#42502=CARTESIAN_POINT('Ctrl Pts',(5.844020362869,-5.50371604744393,-14.2137950881237));
#42503=CARTESIAN_POINT('Ctrl Pts',(-5.843530256076,-4.23580607983558,-11.9384133491196));
#42504=CARTESIAN_POINT('Ctrl Pts',(-3.895686837384,-3.77920631945423,-12.6803362705394));
#42505=CARTESIAN_POINT('Ctrl Pts',(0.000163368930796,-3.32382368434964,
-13.4219152215187));
#42506=CARTESIAN_POINT('Ctrl Pts',(3.896013575246,-3.77924451316813,-12.6802740730544));
#42507=CARTESIAN_POINT('Ctrl Pts',(5.844020362869,-4.23592097205499,-11.9382266622861));
#42508=CARTESIAN_POINT('Ctrl Pts',(-5.843530256076,-3.79656718977774,-10.3003446896952));
#42509=CARTESIAN_POINT('Ctrl Pts',(-3.895686837384,-3.28180463172425,-11.1801039028799));
#42510=CARTESIAN_POINT('Ctrl Pts',(0.0001633689307967,-2.7647865035497,
-12.0604688985302));
#42511=CARTESIAN_POINT('Ctrl Pts',(3.896013575246,-3.28184799491133,-11.1800300651747));
#42512=CARTESIAN_POINT('Ctrl Pts',(5.844020362869,-3.79669671721236,-10.3001233197275));
#42513=CARTESIAN_POINT('Ctrl Pts',(-5.843530256076,-3.68097872426921,-9.52158370504134));
#42514=CARTESIAN_POINT('Ctrl Pts',(-3.895686837384,-3.1209711468501,-10.4634383653078));
#42515=CARTESIAN_POINT('Ctrl Pts',(0.0001633689307967,-2.56014623248247,
-11.4055359487921));
#42516=CARTESIAN_POINT('Ctrl Pts',(3.896013575246,-3.12101818418698,-10.4633593499865));
#42517=CARTESIAN_POINT('Ctrl Pts',(5.844020362869,-3.6811196365252,-9.52134671026255));
#42518=CARTESIAN_POINT('',(-5.732788638925,-3.68906708236562,-9.81543797412044));
#42519=CARTESIAN_POINT('Ctrl Pts',(-5.73644356954166,-9.5212182362576,-17.3763277345531));
#42520=CARTESIAN_POINT('Ctrl Pts',(-5.73766037024463,-8.76684683173291,
-17.028090734259));
#42521=CARTESIAN_POINT('Ctrl Pts',(-5.73849618482518,-8.05516360140243,
-16.5887330605515));
#42522=CARTESIAN_POINT('Ctrl Pts',(-5.73940756700657,-6.75884968378645,
-15.5535369808515));
#42523=CARTESIAN_POINT('Ctrl Pts',(-5.73948313454001,-6.17416092819343,
-14.9577815504229));
#42524=CARTESIAN_POINT('Ctrl Pts',(-5.73887402245194,-5.16463991732877,
-13.6459927354831));
#42525=CARTESIAN_POINT('Ctrl Pts',(-5.73818934283044,-4.74008689118233,
-12.9297576020434));
#42526=CARTESIAN_POINT('Ctrl Pts',(-5.73605973643251,-4.07387566043888,
-11.4195453042489));
#42527=CARTESIAN_POINT('Ctrl Pts',(-5.73461480965608,-3.83284551954944,
-10.6253394036378));
#42528=CARTESIAN_POINT('Ctrl Pts',(-5.732788638925,-3.68906708236562,-9.81543797412044));
#42529=CARTESIAN_POINT('Ctrl Pts',(5.73278688036066,-3.68906294648598,-9.81543868668658));
#42530=CARTESIAN_POINT('Ctrl Pts',(5.37903378703979,-3.59284163073062,-9.98632746914467));
#42531=CARTESIAN_POINT('Ctrl Pts',(5.01625588585428,-3.50245734812832,-10.1410436198638));
#42532=CARTESIAN_POINT('Ctrl Pts',(4.64606584067004,-3.4196218239831,-10.2790646475806));
#42533=CARTESIAN_POINT('Ctrl Pts',(4.3717064383795,-3.35822983036102,-10.3813563411593));
#42534=CARTESIAN_POINT('Ctrl Pts',(4.0932757270239,-3.30098748245638,-10.4744756568886));
#42535=CARTESIAN_POINT('Ctrl Pts',(3.8114301982303,-3.24859133006159,-10.5582373815854));
#42536=CARTESIAN_POINT('Ctrl Pts',(3.57233893573706,-3.204143357871,-10.6292929579932));
#42537=CARTESIAN_POINT('Ctrl Pts',(3.33079029164474,-3.16318341588268,-10.6936140694128));
#42538=CARTESIAN_POINT('Ctrl Pts',(3.08718502825172,-3.12611849781819,-10.7511239095404));
#42539=CARTESIAN_POINT('Ctrl Pts',(3.04362356893838,-3.1194905543258,-10.7614078111522));
#42540=CARTESIAN_POINT('Ctrl Pts',(2.99999634605026,-3.11298709530054,-10.7714740291743));
#42541=CARTESIAN_POINT('Ctrl Pts',(2.95630565116257,-3.10661035551622,-10.7813222892007));
#42542=CARTESIAN_POINT('Ctrl Pts',(2.75783727944364,-3.07764352024104,-10.8260587745489));
#42543=CARTESIAN_POINT('Ctrl Pts',(2.55805789464781,-3.05130996919154,-10.8663594316571));
#42544=CARTESIAN_POINT('Ctrl Pts',(2.35723405313087,-3.02778623237469,-10.9020986226108));
#42545=CARTESIAN_POINT('Ctrl Pts',(2.16323819137806,-3.00506229899627,-10.9366226865617));
#42546=CARTESIAN_POINT('Ctrl Pts',(1.96826768825925,-2.98496040015708,-10.9668901438503));
#42547=CARTESIAN_POINT('Ctrl Pts',(1.77256282543726,-2.96761517395057,-10.9928292031195));
#42548=CARTESIAN_POINT('Ctrl Pts',(1.57994261266313,-2.95054333876805,-11.0183594175635));
#42549=CARTESIAN_POINT('Ctrl Pts',(1.38661100732697,-2.93614205053063,-11.0396964692977));
#42550=CARTESIAN_POINT('Ctrl Pts',(1.1927971074576,-2.92451449290185,-11.0568142909632));
#42551=CARTESIAN_POINT('Ctrl Pts',(0.994683243107288,-2.91262896572167,
-11.0743118894415));
#42552=CARTESIAN_POINT('Ctrl Pts',(0.796065446409081,-2.90364186949685,
-11.0874005424206));
#42553=CARTESIAN_POINT('Ctrl Pts',(0.597188404533596,-2.89763401017108,
-11.0961016630333));
#42554=CARTESIAN_POINT('Ctrl Pts',(0.408362354537037,-2.89192978038809,
-11.1043630401151));
#42555=CARTESIAN_POINT('Ctrl Pts',(0.219302601049658,-2.88891114283554,
-11.1086693634381));
#42556=CARTESIAN_POINT('Ctrl Pts',(0.0302185760373398,-2.8886206466935,
-11.1090834497124));
#42557=CARTESIAN_POINT('Ctrl Pts',(0.0201538524472,-2.88860518392041,-11.109105491045));
#42558=CARTESIAN_POINT('Ctrl Pts',(0.0100890600883165,-2.88859744448944,
-11.1091165150391));
#42559=CARTESIAN_POINT('Ctrl Pts',(2.42305459169099E-5,-2.88859743267018,
-11.1091165347574));
#42560=CARTESIAN_POINT('Ctrl Pts',(1.61536968630372E-5,-2.88859743266069,
-11.1091165347732));
#42561=CARTESIAN_POINT('Ctrl Pts',(8.07684783334205E-6,-2.88859743265618,
-11.1091165347819));
#42562=CARTESIAN_POINT('Ctrl Pts',(-1.17328610291081E-12,-2.88859743265665,
-11.1091165347836));
#42563=CARTESIAN_POINT('Ctrl Pts',(-0.189437344854955,-2.88859744363441,
-11.1091165734976));
#42564=CARTESIAN_POINT('Ctrl Pts',(-0.378861690437173,-2.89133726996081,
-11.1052144979462));
#42565=CARTESIAN_POINT('Ctrl Pts',(-0.568062428807369,-2.89677554744192,
-11.097344766198));
#42566=CARTESIAN_POINT('Ctrl Pts',(-0.769447710209329,-2.90256405043779,
-11.0889682230813));
#42567=CARTESIAN_POINT('Ctrl Pts',(-0.970579656371806,-2.91140995242851,
-11.0760962038057));
#42568=CARTESIAN_POINT('Ctrl Pts',(-1.17120429318957,-2.92323076595731,
-11.0587041736618));
#42569=CARTESIAN_POINT('Ctrl Pts',(-1.36703736658995,-2.93476926033246,
-11.0417275212937));
#42570=CARTESIAN_POINT('Ctrl Pts',(-1.56238707363891,-2.94914199135374,
-11.0204446274376));
#42571=CARTESIAN_POINT('Ctrl Pts',(-1.75701720624661,-2.96624345460967,
-10.994880896949));
#42572=CARTESIAN_POINT('Ctrl Pts',(-1.95879053438656,-2.98397256526165,
-10.9683789421321));
#42573=CARTESIAN_POINT('Ctrl Pts',(-2.15979050006648,-3.00463437240796,
-10.9372761550918));
#42574=CARTESIAN_POINT('Ctrl Pts',(-2.35975392151571,-3.02808173670664,
-10.9016506212175));
#42575=CARTESIAN_POINT('Ctrl Pts',(-2.55971734296493,-3.05152910100532,
-10.8660250873432));
#42576=CARTESIAN_POINT('Ctrl Pts',(-2.75864422018347,-3.07776182110568,
-10.825877125748));
#42577=CARTESIAN_POINT('Ctrl Pts',(-2.95627137140066,-3.10660556548852,
-10.7813308547632));
#42578=CARTESIAN_POINT('Ctrl Pts',(-3.19883119754988,-3.14200724779738,
-10.7266565062279));
#42579=CARTESIAN_POINT('Ctrl Pts',(-3.43943497053319,-3.18131687623534,
-10.665260368241));
#42580=CARTESIAN_POINT('Ctrl Pts',(-3.67769055117286,-3.22414075633116,
-10.5972094009893));
#42581=CARTESIAN_POINT('Ctrl Pts',(-3.96259738974965,-3.27534969868177,
-10.5158338214973));
#42582=CARTESIAN_POINT('Ctrl Pts',(-4.24414644049201,-3.33158317306783,
-10.4249426846565));
#42583=CARTESIAN_POINT('Ctrl Pts',(-4.52166717124462,-3.3921331042644,-10.3247174210247));
#42584=CARTESIAN_POINT('Ctrl Pts',(-4.88864236905086,-3.47220035876374,
-10.1921861112134));
#42585=CARTESIAN_POINT('Ctrl Pts',(-5.24857377478926,-3.5598100414616,-10.0433370079679));
#42586=CARTESIAN_POINT('Ctrl Pts',(-5.59991098953761,-3.65331093395734,
-9.87866971603991));
#42587=CARTESIAN_POINT('Ctrl Pts',(-5.64434240534598,-3.66513540588499,
-9.85784527555776));
#42588=CARTESIAN_POINT('Ctrl Pts',(-5.68863637360616,-3.67705416337425,
-9.8367678762802));
#42589=CARTESIAN_POINT('Ctrl Pts',(-5.73278975856799,-3.68906394712505,
-9.81543852851373));
#42590=CARTESIAN_POINT('Ctrl Pts',(5.84421883180474,-3.72282215870307,-9.78170207264411));
#42591=CARTESIAN_POINT('Ctrl Pts',(5.60210555070136,-3.65638716931675,-9.90489110085523));
#42592=CARTESIAN_POINT('Ctrl Pts',(4.82411485412597,-3.45517207621565,-10.2687173462891));
#42593=CARTESIAN_POINT('Ctrl Pts',(3.45674861901373,-3.1717867894043,-10.7434846212514));
#42594=CARTESIAN_POINT('Ctrl Pts',(1.73637252749493,-2.95116599793079,-11.0872359518019));
#42595=CARTESIAN_POINT('Ctrl Pts',(0.00178708571280825,-2.87580440265437,
-11.2002490127008));
#42596=CARTESIAN_POINT('Ctrl Pts',(-1.73280014723785,-2.95085735941276,
-11.0877033118007));
#42597=CARTESIAN_POINT('Ctrl Pts',(-3.45327880384202,-3.1711983285024,-10.7444278554086));
#42598=CARTESIAN_POINT('Ctrl Pts',(-4.82196103408831,-3.45464798710974,
-10.269637251114));
#42599=CARTESIAN_POINT('Ctrl Pts',(-5.60114390651019,-3.6561220066129,-9.90538363300166));
#42600=CARTESIAN_POINT('Ctrl Pts',(-5.8443346108831,-3.72285393964802,-9.78164313446629));
#42601=CARTESIAN_POINT('Ctrl Pts',(5.7253702758327,-3.64455037473193,-9.50230796587388));
#42602=CARTESIAN_POINT('Ctrl Pts',(5.4881314994798,-3.58036715962835,-9.62279259868668));
#42603=CARTESIAN_POINT('Ctrl Pts',(4.72581564301797,-3.38588375667695,-9.97867779049632));
#42604=CARTESIAN_POINT('Ctrl Pts',(3.38610693741535,-3.11167079843839,-10.4432062423216));
#42605=CARTESIAN_POINT('Ctrl Pts',(1.70079220243387,-2.89802964660707,-10.7795799094507));
#42606=CARTESIAN_POINT('Ctrl Pts',(0.00175042691972879,-2.82503096864176,
-10.8901685400845));
#42607=CARTESIAN_POINT('Ctrl Pts',(-1.69729287672102,-2.89773070464145,
-10.7800372441397));
#42608=CARTESIAN_POINT('Ctrl Pts',(-3.3827075656956,-3.11110109891825,-10.4441292117391));
#42609=CARTESIAN_POINT('Ctrl Pts',(-4.72370524846715,-3.38537694518877,
-9.97957774413633));
#42610=CARTESIAN_POINT('Ctrl Pts',(-5.48718921578431,-3.58011099558317,
-9.62327431064613));
#42611=CARTESIAN_POINT('Ctrl Pts',(-5.72548372426805,-3.64458107905496,
-9.50225032158714));
#42612=CARTESIAN_POINT('Ctrl Pts',(5.71942246157996,-3.37473909219602,-9.34268285703912));
#42613=CARTESIAN_POINT('Ctrl Pts',(5.48287285233699,-3.3112654349926,-9.46194227133996));
#42614=CARTESIAN_POINT('Ctrl Pts',(4.72266850715085,-3.11884881435695,-9.81433425125829));
#42615=CARTESIAN_POINT('Ctrl Pts',(3.38569730696337,-2.84709739195396,-10.2749197644463));
#42616=CARTESIAN_POINT('Ctrl Pts',(1.70145185496075,-2.63491822139972,-10.6090358172226));
#42617=CARTESIAN_POINT('Ctrl Pts',(0.00175145994779487,-2.56231815139111,
-10.7190101985091));
#42618=CARTESIAN_POINT('Ctrl Pts',(-1.69795250354239,-2.63462102463518,
-10.6094904682724));
#42619=CARTESIAN_POINT('Ctrl Pts',(-3.38230253911364,-2.84653212429915,
-10.2758358266937));
#42620=CARTESIAN_POINT('Ctrl Pts',(-4.72056368204768,-3.11834712228491,
-9.81522575608262));
#42621=CARTESIAN_POINT('Ctrl Pts',(-5.48193330987248,-3.311012103631,-9.4624190734827));
#42622=CARTESIAN_POINT('Ctrl Pts',(-5.71953557724954,-3.37476945656438,
-9.34262580081448));
#42623=CARTESIAN_POINT('Ctrl Pts',(5.83023580926565,-3.08842202064092,-9.40638358569627));
#42624=CARTESIAN_POINT('Ctrl Pts',(5.58974287210655,-3.02365536252599,-9.52669182842707));
#42625=CARTESIAN_POINT('Ctrl Pts',(4.81671666980029,-2.8272997397519,-9.88230469038235));
#42626=CARTESIAN_POINT('Ctrl Pts',(3.45578661938464,-2.54970205873507,-10.3478011867109));
#42627=CARTESIAN_POINT('Ctrl Pts',(1.73792413620994,-2.33251867796578,-10.6862443582688));
#42628=CARTESIAN_POINT('Ctrl Pts',(0.00178951524897414,-2.25809428228155,
-10.7978131876545));
#42629=CARTESIAN_POINT('Ctrl Pts',(-1.73435169431629,-2.33221414274175,
-10.6867054084471));
#42630=CARTESIAN_POINT('Ctrl Pts',(-3.45232762804018,-2.54912401807523,
-10.3487281805197));
#42631=CARTESIAN_POINT('Ctrl Pts',(-4.81457594437186,-2.82678768753553,
-9.8832047300166));
#42632=CARTESIAN_POINT('Ctrl Pts',(-5.58878767299468,-3.02339686010146,
-9.52717281640476));
#42633=CARTESIAN_POINT('Ctrl Pts',(-5.83035080595657,-3.08845300227363,
-9.4063260301971));
#42634=CARTESIAN_POINT('',(-5.7200185442403,-3.0799676360579,-9.45352569283355));
#42635=CARTESIAN_POINT('Origin',(-5.89878573791871,-3.22460261179308,-9.89753636536867));
#42636=CARTESIAN_POINT('Ctrl Pts',(5.72001578658213,-3.07996614583804,-9.45352684908776));
#42637=CARTESIAN_POINT('Ctrl Pts',(5.51356681596581,-3.02529977540968,-9.55445522100768));
#42638=CARTESIAN_POINT('Ctrl Pts',(5.30316956267147,-2.97232139279663,-9.65016641036658));
#42639=CARTESIAN_POINT('Ctrl Pts',(5.08894867055704,-2.92143297802579,-9.74045681632173));
#42640=CARTESIAN_POINT('Ctrl Pts',(4.85594668814816,-2.8660830940522,-9.8386631274448));
#42641=CARTESIAN_POINT('Ctrl Pts',(4.61842051735488,-2.81320484592507,-9.93045706148136));
#42642=CARTESIAN_POINT('Ctrl Pts',(4.3766008775274,-2.76339299495987,-10.0155394511694));
#42643=CARTESIAN_POINT('Ctrl Pts',(4.14452715583251,-2.71558868243068,-10.0971928141457));
#42644=CARTESIAN_POINT('Ctrl Pts',(3.90849626788228,-2.67057763096145,-10.1726744199736));
#42645=CARTESIAN_POINT('Ctrl Pts',(3.66875283939545,-2.62875548050569,-10.2417200197346));
#42646=CARTESIAN_POINT('Ctrl Pts',(3.58862574672169,-2.61477767370391,-10.26479645276));
#42647=CARTESIAN_POINT('Ctrl Pts',(3.50808466559867,-2.6011553063792,-10.2871537896843));
#42648=CARTESIAN_POINT('Ctrl Pts',(3.42713923261638,-2.58790184224115,-10.3087818015856));
#42649=CARTESIAN_POINT('Ctrl Pts',(3.3869886980803,-2.58132786209191,-10.3195097229371));
#42650=CARTESIAN_POINT('Ctrl Pts',(3.34673867487783,-2.57484465155967,-10.3300581989155));
#42651=CARTESIAN_POINT('Ctrl Pts',(3.30639080102876,-2.56845356021827,-10.3404260905222));
#42652=CARTESIAN_POINT('Ctrl Pts',(3.24554522478032,-2.55881563885026,-10.3560611235267));
#42653=CARTESIAN_POINT('Ctrl Pts',(3.1844766843321,-2.54938754043835,-10.3712855031509));
#42654=CARTESIAN_POINT('Ctrl Pts',(3.12319004734369,-2.54017420676512,-10.3860953093476));
#42655=CARTESIAN_POINT('Ctrl Pts',(3.08513329993774,-2.53445306542668,-10.3952916542811));
#42656=CARTESIAN_POINT('Ctrl Pts',(3.04632095066816,-2.52871572983249,-10.4044864855534));
#42657=CARTESIAN_POINT('Ctrl Pts',(3.00800426616806,-2.52314921706523,-10.4133813072128));
#42658=CARTESIAN_POINT('Ctrl Pts',(2.98461571063522,-2.51975141021738,-10.4188107182656));
#42659=CARTESIAN_POINT('Ctrl Pts',(2.96141213571219,-2.51641677170785,-10.4241292288973));
#42660=CARTESIAN_POINT('Ctrl Pts',(2.93868070631794,-2.51318337406863,-10.4292769885392));
#42661=CARTESIAN_POINT('Ctrl Pts',(2.67982640696756,-2.47636303752467,-10.4878971347796));
#42662=CARTESIAN_POINT('Ctrl Pts',(2.41895243086841,-2.44400427296749,-10.5386806582089));
#42663=CARTESIAN_POINT('Ctrl Pts',(2.15650358185332,-2.41645036367251,-10.5815940612891));
#42664=CARTESIAN_POINT('Ctrl Pts',(2.00946578054502,-2.40101319846723,-10.6056364316757));
#42665=CARTESIAN_POINT('Ctrl Pts',(1.86193310803913,-2.38708447197652,-10.6272077902081));
#42666=CARTESIAN_POINT('Ctrl Pts',(1.71398017126471,-2.37472713185341,-10.6462966328573));
#42667=CARTESIAN_POINT('Ctrl Pts',(1.4531427413368,-2.35294144169592,-10.6799497982858));
#42668=CARTESIAN_POINT('Ctrl Pts',(1.19099999568001,-2.33603818365922,-10.705889511206));
#42669=CARTESIAN_POINT('Ctrl Pts',(0.928059192655602,-2.32412814711591,
-10.7241021511244));
#42670=CARTESIAN_POINT('Ctrl Pts',(0.66629372200498,-2.31227134784639,-10.7422333814439));
#42671=CARTESIAN_POINT('Ctrl Pts',(0.40373671189424,-2.30536303813329,-10.7527065306979));
#42672=CARTESIAN_POINT('Ctrl Pts',(0.14087630804359,-2.30353950361934,-10.7554660904619));
#42673=CARTESIAN_POINT('Ctrl Pts',(0.0945133613883472,-2.3032178711781,
-10.7559528177143));
#42674=CARTESIAN_POINT('Ctrl Pts',(0.0481409586041718,-2.30305449545756,
-10.7561994721505));
#42675=CARTESIAN_POINT('Ctrl Pts',(0.00176176044996187,-2.30305021913014,
-10.7562056100611));
#42676=CARTESIAN_POINT('Ctrl Pts',(0.00117444596505243,-2.30305016497765,
-10.7562056877874));
#42677=CARTESIAN_POINT('Ctrl Pts',(0.000587130390413492,-2.30305013633867,
-10.756205726944));
#42678=CARTESIAN_POINT('Ctrl Pts',(-1.86268554556318E-7,-2.30305013321116,
-10.7562057275312));
#42679=CARTESIAN_POINT('Ctrl Pts',(-0.255000491349255,-2.30304877531682,
-10.7562059824751));
#42680=CARTESIAN_POINT('Ctrl Pts',(-0.509774434758715,-2.30783485820167,
-10.7489431787096));
#42681=CARTESIAN_POINT('Ctrl Pts',(-0.763898932404416,-2.31730701398244,
-10.7344707880309));
#42682=CARTESIAN_POINT('Ctrl Pts',(-1.00372079461643,-2.32624605787451,
-10.7208129324705));
#42683=CARTESIAN_POINT('Ctrl Pts',(-1.24296459205544,-2.33935895111826,
-10.700733749856));
#42684=CARTESIAN_POINT('Ctrl Pts',(-1.48126244510556,-2.356582676509,-10.6742439838085));
#42685=CARTESIAN_POINT('Ctrl Pts',(-1.5577578438524,-2.36211162158679,-10.665740570158));
#42686=CARTESIAN_POINT('Ctrl Pts',(-1.63415741723896,-2.36805837750173,
-10.6565774625737));
#42687=CARTESIAN_POINT('Ctrl Pts',(-1.71044775245404,-2.37442125867848,
-10.6467543951761));
#42688=CARTESIAN_POINT('Ctrl Pts',(-1.87890328193537,-2.38847103988123,
-10.6250642293781));
#42689=CARTESIAN_POINT('Ctrl Pts',(-2.04682653109725,-2.40454952041417,
-10.6001567271322));
#42690=CARTESIAN_POINT('Ctrl Pts',(-2.21410026640134,-2.42257268343704,
-10.572046645807));
#42691=CARTESIAN_POINT('Ctrl Pts',(-2.33561469550333,-2.43566544041622,
-10.5516263420574));
#42692=CARTESIAN_POINT('Ctrl Pts',(-2.45678531457589,-2.44978651145652,
-10.5295155390599));
#42693=CARTESIAN_POINT('Ctrl Pts',(-2.57756645267151,-2.46490128099779,
-10.5057186054411));
#42694=CARTESIAN_POINT('Ctrl Pts',(-2.63795702171931,-2.47245866576843,
-10.4938201386317));
#42695=CARTESIAN_POINT('Ctrl Pts',(-2.69825021746175,-2.48026446967665,
-10.4815001146347));
#42696=CARTESIAN_POINT('Ctrl Pts',(-2.75844045211332,-2.48831371733907,
-10.4687590489619));
#42697=CARTESIAN_POINT('Ctrl Pts',(-2.795972562294,-2.49333289116164,-10.4608142538731));
#42698=CARTESIAN_POINT('Ctrl Pts',(-2.83278783471037,-2.49835393714893,
-10.4528528804943));
#42699=CARTESIAN_POINT('Ctrl Pts',(-2.87015176601266,-2.50354781733663,
-10.4446022649074));
#42700=CARTESIAN_POINT('Ctrl Pts',(-2.89270836094146,-2.5066833613605,-10.4396213705737));
#42701=CARTESIAN_POINT('Ctrl Pts',(-2.9154646728921,-2.50988236193164,-10.4345342417536));
#42702=CARTESIAN_POINT('Ctrl Pts',(-2.93869667983939,-2.5131867540875,-10.4292731465582));
#42703=CARTESIAN_POINT('Ctrl Pts',(-3.10185557320944,-2.5363935725356,-10.3923243598291));
#42704=CARTESIAN_POINT('Ctrl Pts',(-3.26352239546762,-2.56118034873841,
-10.3524399770393));
#42705=CARTESIAN_POINT('Ctrl Pts',(-3.42360171637816,-2.58742510026999,
-10.309700957847));
#42706=CARTESIAN_POINT('Ctrl Pts',(-3.67169453244662,-2.62809952515793,
-10.2434635227612));
#42707=CARTESIAN_POINT('Ctrl Pts',(-3.91597451893442,-2.67227397445666,
-10.1703712528922));
#42708=CARTESIAN_POINT('Ctrl Pts',(-4.15620380046542,-2.71944877115637,
-10.0907290824044));
#42709=CARTESIAN_POINT('Ctrl Pts',(-4.40438535371314,-2.76818518765174,
-10.0084505298079));
#42710=CARTESIAN_POINT('Ctrl Pts',(-4.64824377246369,-2.8201241159297,-9.91918128445061));
#42711=CARTESIAN_POINT('Ctrl Pts',(-4.88751685622871,-2.87475428965369,
-9.82321881397021));
#42712=CARTESIAN_POINT('Ctrl Pts',(-4.95392625599963,-2.88991670152762,
-9.79658476903352));
#42713=CARTESIAN_POINT('Ctrl Pts',(-5.01998242881333,-2.90528664210822,
-9.76943490709447));
#42714=CARTESIAN_POINT('Ctrl Pts',(-5.08567973802691,-2.92085365990828,
-9.74177507982081));
#42715=CARTESIAN_POINT('Ctrl Pts',(-5.30103361184729,-2.97188189268074,
-9.65110696838838));
#42716=CARTESIAN_POINT('Ctrl Pts',(-5.5125318672241,-3.02502631681574,-9.55496102222212));
#42717=CARTESIAN_POINT('Ctrl Pts',(-5.72001839641912,-3.07996751644906,
-9.45352532568119));
#42718=CARTESIAN_POINT('Ctrl Pts',(-5.71197198844382,-3.68829479791916,
-9.8501703687033));
#42719=CARTESIAN_POINT('Ctrl Pts',(-5.71754580782435,-3.68940667657091,
-9.84753623637226));
#42720=CARTESIAN_POINT('Ctrl Pts',(-5.76536778611043,-3.69987796915319,
-9.8245378123085));
#42721=CARTESIAN_POINT('Ctrl Pts',(-5.85070495630983,-3.73375492021359,
-9.77700012003639));
#42722=CARTESIAN_POINT('Ctrl Pts',(-5.94870719254402,-3.81192663887559,
-9.70547744306355));
#42723=CARTESIAN_POINT('Ctrl Pts',(-6.01636824229405,-3.91100725665301,
-9.6365907833745));
#42724=CARTESIAN_POINT('Ctrl Pts',(-6.04738225412035,-4.00919272256942,
-9.58227189268685));
#42725=CARTESIAN_POINT('Ctrl Pts',(-6.05143261400087,-4.07095169026726,
-9.55421326848555));
#42726=CARTESIAN_POINT('Ctrl Pts',(-6.05072985177984,-4.09544619788918,
-9.5440201179351));
#42727=CARTESIAN_POINT('Ctrl Pts',(-5.59589935073135,-3.61241520274072,
-9.56651528941115));
#42728=CARTESIAN_POINT('Ctrl Pts',(-5.60110010589582,-3.61342022961924,
-9.56406241085858));
#42729=CARTESIAN_POINT('Ctrl Pts',(-5.64572896520279,-3.62289723996144,
-9.5426450484337));
#42730=CARTESIAN_POINT('Ctrl Pts',(-5.72547570812964,-3.6537490789919,-9.49835555934878));
#42731=CARTESIAN_POINT('Ctrl Pts',(-5.81705924964759,-3.72520141233989,
-9.43184052695804));
#42732=CARTESIAN_POINT('Ctrl Pts',(-5.88013461718338,-3.81569531693298,
-9.3680978453068));
#42733=CARTESIAN_POINT('Ctrl Pts',(-5.90887905532575,-3.90498789181401,
-9.31830046586544));
#42734=CARTESIAN_POINT('Ctrl Pts',(-5.91259286860787,-3.96076595326123,
-9.29290817691202));
#42735=CARTESIAN_POINT('Ctrl Pts',(-5.91194771160934,-3.98280987749108,
-9.28374470677804));
#42736=CARTESIAN_POINT('Ctrl Pts',(-5.57877004579782,-3.33842765893124,
-9.41053844742967));
#42737=CARTESIAN_POINT('Ctrl Pts',(-5.58616524518609,-3.33985698600003,
-9.40710010435303));
#42738=CARTESIAN_POINT('Ctrl Pts',(-5.6495565331106,-3.35331617480298,-9.37712813939376));
#42739=CARTESIAN_POINT('Ctrl Pts',(-5.76186844825849,-3.39674464954052,
-9.31592123793131));
#42740=CARTESIAN_POINT('Ctrl Pts',(-5.89083814572667,-3.49676380958585,
-9.22450171582332));
#42741=CARTESIAN_POINT('Ctrl Pts',(-5.98103739468164,-3.62475240735847,
-9.13578477922984));
#42742=CARTESIAN_POINT('Ctrl Pts',(-6.0236413123101,-3.75450472600272,-9.0641622319954));
#42743=CARTESIAN_POINT('Ctrl Pts',(-6.02950682140399,-3.83881283105142,
-9.02585447175553));
#42744=CARTESIAN_POINT('Ctrl Pts',(-6.02849503592009,-3.87279257907653,
-9.01170707669297));
#42745=CARTESIAN_POINT('Ctrl Pts',(-5.67181053456004,-3.04590420482865,
-9.48446714171748));
#42746=CARTESIAN_POINT('Ctrl Pts',(-5.68252944195994,-3.04801089652616,
-9.4795224919317));
#42747=CARTESIAN_POINT('Ctrl Pts',(-5.77434175986858,-3.06781879365414,
-9.43646696993557));
#42748=CARTESIAN_POINT('Ctrl Pts',(-5.93603114512472,-3.13118288995348,
-9.34926475855966));
#42749=CARTESIAN_POINT('Ctrl Pts',(-6.12168886188134,-3.27633231152322,
-9.2193510829));
#42750=CARTESIAN_POINT('Ctrl Pts',(-6.25294449101188,-3.46332288353974,
-9.09190985330162));
#42751=CARTESIAN_POINT('Ctrl Pts',(-6.31645340122605,-3.6563701535287,-8.98641973386077));
#42752=CARTESIAN_POINT('Ctrl Pts',(-6.32554862134644,-3.78502058339552,
-8.92807953097214));
#42753=CARTESIAN_POINT('Ctrl Pts',(-6.32398626296098,-3.83749979088896,
-8.90620108365363));
#42754=CARTESIAN_POINT('',(-5.99998805436274,-3.9978865442048,-9.34661202445984));
#42755=CARTESIAN_POINT('',(-5.99999999729861,-3.21424235897937,-9.29218336212829));
#42756=CARTESIAN_POINT('Ctrl Pts',(-5.99998805436274,-3.9978865442048,-9.34661202445984));
#42757=CARTESIAN_POINT('Ctrl Pts',(-5.99998615757755,-3.97569967948952,
-9.33734483768274));
#42758=CARTESIAN_POINT('Ctrl Pts',(-5.99998787688148,-3.95340882073654,
-9.32855545295178));
#42759=CARTESIAN_POINT('Ctrl Pts',(-6.00000067043316,-3.9310658935729,-9.32034755058032));
#42760=CARTESIAN_POINT('Ctrl Pts',(-6.00000703302803,-3.91995412434894,
-9.31626552872632));
#42761=CARTESIAN_POINT('Ctrl Pts',(-6.00001548520134,-3.908829972833,-9.31232702313013));
#42762=CARTESIAN_POINT('Ctrl Pts',(-6.00002414590328,-3.89770276645304,
-9.30854234483346));
#42763=CARTESIAN_POINT('Ctrl Pts',(-6.00004249128253,-3.87413275763661,
-9.30052551673));
#42764=CARTESIAN_POINT('Ctrl Pts',(-6.00006348281536,-3.85054713585633,
-9.29320139494933));
#42765=CARTESIAN_POINT('Ctrl Pts',(-6.00008478134917,-3.82704822256206,
-9.28663239331664));
#42766=CARTESIAN_POINT('Ctrl Pts',(-6.00009878952125,-3.81159284783559,
-9.28231192195949));
#42767=CARTESIAN_POINT('Ctrl Pts',(-6.00011226036874,-3.79617570477161,
-9.27831732549394));
#42768=CARTESIAN_POINT('Ctrl Pts',(-6.00012161146963,-3.78083205625065,
-9.27465621621041));
#42769=CARTESIAN_POINT('Ctrl Pts',(-6.00013617109966,-3.75694205139138,
-9.26895588239122));
#42770=CARTESIAN_POINT('Ctrl Pts',(-6.00013962298854,-3.73322992383675,
-9.26406658182334));
#42771=CARTESIAN_POINT('Ctrl Pts',(-6.00012391442244,-3.70984226421294,
-9.25997601119208));
#42772=CARTESIAN_POINT('Ctrl Pts',(-6.00011963924351,-3.70347717468189,
-9.2588627382644));
#42773=CARTESIAN_POINT('Ctrl Pts',(-6.00011403061838,-3.69713617242992,
-9.25780834367095));
#42774=CARTESIAN_POINT('Ctrl Pts',(-6.00010715608015,-3.69082229089165,
-9.25681195952613));
#42775=CARTESIAN_POINT('Ctrl Pts',(-6.00010131553909,-3.68545807832469,
-9.25596544121266));
#42776=CARTESIAN_POINT('Ctrl Pts',(-6.00009456501949,-3.68011344099444,
-9.25516079029681));
#42777=CARTESIAN_POINT('Ctrl Pts',(-6.00008712855673,-3.67479011176827,
-9.25439735758586));
#42778=CARTESIAN_POINT('Ctrl Pts',(-6.00006858490899,-3.66151579774108,
-9.25249365313454));
#42779=CARTESIAN_POINT('Ctrl Pts',(-6.00005096959346,-3.64819250826683,
-9.25081521949727));
#42780=CARTESIAN_POINT('Ctrl Pts',(-6.00003052847771,-3.63505165735234,
-9.24939564882071));
#42781=CARTESIAN_POINT('Ctrl Pts',(-6.00000990265753,-3.62179206667071,
-9.2479632510074));
#42782=CARTESIAN_POINT('Ctrl Pts',(-5.99998594742847,-3.60871873802229,
-9.24679454187284));
#42783=CARTESIAN_POINT('Ctrl Pts',(-5.99996790995349,-3.5960857271278,-9.24587435399025));
#42784=CARTESIAN_POINT('Ctrl Pts',(-5.99995721318206,-3.58859396732476,
-9.24532865458038));
#42785=CARTESIAN_POINT('Ctrl Pts',(-5.99994889418915,-3.58125733395095,
-9.24486937940367));
#42786=CARTESIAN_POINT('Ctrl Pts',(-5.99994781651967,-3.57413028014663,
-9.24448539899825));
#42787=CARTESIAN_POINT('Ctrl Pts',(-5.99994381541193,-3.54766937478428,
-9.24305977917727));
#42788=CARTESIAN_POINT('Ctrl Pts',(-5.99996581464687,-3.52111758167283,
-9.24259217744035));
#42789=CARTESIAN_POINT('Ctrl Pts',(-5.99999344291283,-3.49464197784248,
-9.2431668105431));
#42790=CARTESIAN_POINT('Ctrl Pts',(-6.00002107117879,-3.46816637401214,
-9.24374144364584));
#42791=CARTESIAN_POINT('Ctrl Pts',(-6.00005342999203,-3.4417680087858,-9.24535888815406));
#42792=CARTESIAN_POINT('Ctrl Pts',(-6.00007273963438,-3.4156408295774,-9.24804717908462));
#42793=CARTESIAN_POINT('Ctrl Pts',(-6.0000911444452,-3.39073794520572,-9.25060949925195));
#42794=CARTESIAN_POINT('Ctrl Pts',(-6.00009742310507,-3.36608229990409,
-9.25414433396963));
#42795=CARTESIAN_POINT('Ctrl Pts',(-6.00008958768821,-3.34184650386147,
-9.25862572524751));
#42796=CARTESIAN_POINT('Ctrl Pts',(-6.00008165516822,-3.31731035726507,
-9.26316265372952));
#42797=CARTESIAN_POINT('Ctrl Pts',(-6.000058850835,-3.29320556340356,-9.26866951866689));
#42798=CARTESIAN_POINT('Ctrl Pts',(-6.00003612101861,-3.26970688957186,
-9.27506846759169));
#42799=CARTESIAN_POINT('Ctrl Pts',(-6.00001783142877,-3.25079863713838,
-9.28021739397136));
#42800=CARTESIAN_POINT('Ctrl Pts',(-5.99999992125698,-3.23228289786736,
-9.28594277002995));
#42801=CARTESIAN_POINT('Ctrl Pts',(-5.99999992406984,-3.21424228989424,
-9.29218316240729));
#42802=CARTESIAN_POINT('Ctrl Pts',(-5.72001867921778,-3.07996774527742,
-9.45352602808894));
#42803=CARTESIAN_POINT('Ctrl Pts',(-5.77261523598685,-3.09390413589055,
-9.42780998495483));
#42804=CARTESIAN_POINT('Ctrl Pts',(-5.82214285829514,-3.11233855179879,
-9.40146116709804));
#42805=CARTESIAN_POINT('Ctrl Pts',(-5.86877313173194,-3.13479324096957,
-9.37456642764042));
#42806=CARTESIAN_POINT('Ctrl Pts',(-5.91540340287037,-3.15724792903357,
-9.34767168950842));
#42807=CARTESIAN_POINT('Ctrl Pts',(-5.95913655250815,-3.18372307206963,
-9.32023156202287));
#42808=CARTESIAN_POINT('Ctrl Pts',(-6.00000008491191,-3.21424242024491,
-9.29218355643704));
#42809=CARTESIAN_POINT('Ctrl Pts',(-5.73278520692685,-3.68907667907205,
-9.8154362792223));
#42810=CARTESIAN_POINT('Ctrl Pts',(-5.74762382962131,-3.69180325511032,
-9.80082774594881));
#42811=CARTESIAN_POINT('Ctrl Pts',(-5.76162171238064,-3.69529215425996,
-9.78641524403596));
#42812=CARTESIAN_POINT('Ctrl Pts',(-5.77477721800093,-3.69934156434397,
-9.77230761864449));
#42813=CARTESIAN_POINT('Ctrl Pts',(-5.78880577316832,-3.70365970873147,
-9.75726375740514));
#42814=CARTESIAN_POINT('Ctrl Pts',(-5.80187658368747,-3.70861550222048,
-9.74256647678676));
#42815=CARTESIAN_POINT('Ctrl Pts',(-5.81401568052954,-3.71400533038411,
-9.72831583026195));
#42816=CARTESIAN_POINT('Ctrl Pts',(-5.81729336960867,-3.71546064301076,
-9.7244679996455));
#42817=CARTESIAN_POINT('Ctrl Pts',(-5.8205032728521,-3.71694780460071,-9.72065256683664));
#42818=CARTESIAN_POINT('Ctrl Pts',(-5.82364619983945,-3.71846323640865,
-9.71687115362401));
#42819=CARTESIAN_POINT('Ctrl Pts',(-5.83610465210455,-3.7244703549056,-9.70188176437192));
#42820=CARTESIAN_POINT('Ctrl Pts',(-5.84750972960467,-3.73091750184809,
-9.6874295362641));
#42821=CARTESIAN_POINT('Ctrl Pts',(-5.85794382570231,-3.73757946624391,
-9.67360152486396));
#42822=CARTESIAN_POINT('Ctrl Pts',(-5.8688044299202,-3.74451374765551,-9.65920827435793));
#42823=CARTESIAN_POINT('Ctrl Pts',(-5.878613435895,-3.75168144867336,-9.64549094512086));
#42824=CARTESIAN_POINT('Ctrl Pts',(-5.88747619597288,-3.75888048322723,
-9.6325145729761));
#42825=CARTESIAN_POINT('Ctrl Pts',(-5.89165259807077,-3.76227288725818,
-9.6263997117622));
#42826=CARTESIAN_POINT('Ctrl Pts',(-5.89561902734608,-3.76567292020307,
-9.62044895431379));
#42827=CARTESIAN_POINT('Ctrl Pts',(-5.89938714503697,-3.76906266936731,
-9.61466703946109));
#42828=CARTESIAN_POINT('Ctrl Pts',(-5.90174440457449,-3.7711832290745,-9.61104998844258));
#42829=CARTESIAN_POINT('Ctrl Pts',(-5.90402406175946,-3.77329980253791,
-9.6074989896858));
#42830=CARTESIAN_POINT('Ctrl Pts',(-5.9062290268245,-3.77540836081767,-9.60401497849346));
#42831=CARTESIAN_POINT('Ctrl Pts',(-5.90952625901899,-3.77856142947814,
-9.59880510281265));
#42832=CARTESIAN_POINT('Ctrl Pts',(-5.91265649617662,-3.78169648827022,
-9.59374505629813));
#42833=CARTESIAN_POINT('Ctrl Pts',(-5.91563044428714,-3.78480001737202,
-9.58883752575352));
#42834=CARTESIAN_POINT('Ctrl Pts',(-5.91811180565001,-3.78738949671584,
-9.58474284883651));
#42835=CARTESIAN_POINT('Ctrl Pts',(-5.920484295981,-3.78995698533474,-9.58075441007369));
#42836=CARTESIAN_POINT('Ctrl Pts',(-5.92275407850264,-3.79249552701193,
-9.57687328474074));
#42837=CARTESIAN_POINT('Ctrl Pts',(-5.92388896976347,-3.79376479785053,
-9.57493272207426));
#42838=CARTESIAN_POINT('Ctrl Pts',(-5.92499817681059,-3.79502683695038,
-9.57301898699673));
#42839=CARTESIAN_POINT('Ctrl Pts',(-5.92608244824651,-3.79628082871286,
-9.571132197062));
#42840=CARTESIAN_POINT('Ctrl Pts',(-5.92684317282743,-3.79716062903442,
-9.56980842569366));
#42841=CARTESIAN_POINT('Ctrl Pts',(-5.92727871378404,-3.79766914381903,
-9.56904606582659));
#42842=CARTESIAN_POINT('Ctrl Pts',(-5.928049092874,-3.79857833855905,-9.56769139022369));
#42843=CARTESIAN_POINT('Ctrl Pts',(-5.92837674592737,-3.79896503185922,
-9.56711522765203));
#42844=CARTESIAN_POINT('Ctrl Pts',(-5.92876465306642,-3.79942445551461,
-9.56643192389701));
#42845=CARTESIAN_POINT('Ctrl Pts',(-5.92926118432832,-3.80001787185852,
-9.56555277030981));
#42846=CARTESIAN_POINT('Ctrl Pts',(-5.9392063852684,-3.81190361850559,-9.54794389096479));
#42847=CARTESIAN_POINT('Ctrl Pts',(-5.94794390660985,-3.82419219851774,
-9.5309806794631));
#42848=CARTESIAN_POINT('Ctrl Pts',(-5.95555097031253,-3.83668111574082,
-9.51474001570556));
#42849=CARTESIAN_POINT('Ctrl Pts',(-5.95867322267065,-3.84180708191834,
-9.50807417817662));
#42850=CARTESIAN_POINT('Ctrl Pts',(-5.96160508865422,-3.84696733110998,
-9.50152971460728));
#42851=CARTESIAN_POINT('Ctrl Pts',(-5.96435219187444,-3.85214989453163,
-9.49511056986388));
#42852=CARTESIAN_POINT('Ctrl Pts',(-5.97117112933457,-3.86501420031934,
-9.4791767868773));
#42853=CARTESIAN_POINT('Ctrl Pts',(-5.9768525793462,-3.87801257167857,-9.46401683414202));
#42854=CARTESIAN_POINT('Ctrl Pts',(-5.98152771173936,-3.89095751760361,
-9.44967300324281));
#42855=CARTESIAN_POINT('Ctrl Pts',(-5.98650278304255,-3.90473296257011,
-9.43440892610375));
#42856=CARTESIAN_POINT('Ctrl Pts',(-5.99033781740992,-3.91844820403234,
-9.4200690225312));
#42857=CARTESIAN_POINT('Ctrl Pts',(-5.99318392794507,-3.93192830023576,
-9.40667643182402));
#42858=CARTESIAN_POINT('Ctrl Pts',(-5.99387721931419,-3.93521195146339,
-9.40341409628478));
#42859=CARTESIAN_POINT('Ctrl Pts',(-5.99451181801508,-3.9384818624222,-9.40020785074143));
#42860=CARTESIAN_POINT('Ctrl Pts',(-5.99508989597192,-3.94173589648596,
-9.39705780395256));
#42861=CARTESIAN_POINT('Ctrl Pts',(-5.99756671015925,-3.95567802598549,
-9.38356121498038));
#42862=CARTESIAN_POINT('Ctrl Pts',(-5.99900795538788,-3.96932498629971,
-9.37109761283901));
#42863=CARTESIAN_POINT('Ctrl Pts',(-5.99962729227282,-3.98252532525775,
-9.35964972360189));
#42864=CARTESIAN_POINT('Ctrl Pts',(-5.99987086536048,-3.9877167604788,-9.35514749259242));
#42865=CARTESIAN_POINT('Ctrl Pts',(-5.99998706574566,-3.99283961991828,
-9.35080217488171));
#42866=CARTESIAN_POINT('Ctrl Pts',(-5.99998805436274,-3.99788654420479,
-9.34661202445984));
#42867=CARTESIAN_POINT('Ctrl Pts',(-5.72202476730477,-9.61344956113702,
-17.4236870238206));
#42868=CARTESIAN_POINT('Ctrl Pts',(-5.72274570226849,-9.17589143465609,
-17.2270248402683));
#42869=CARTESIAN_POINT('Ctrl Pts',(-5.72404124879816,-8.29086215801847,
-16.7525775515301));
#42870=CARTESIAN_POINT('Ctrl Pts',(-5.72530541068372,-7.06378515805125,
-15.8436322695082));
#42871=CARTESIAN_POINT('Ctrl Pts',(-5.72546532299495,-5.95933659063332,
-14.7303948480276));
#42872=CARTESIAN_POINT('Ctrl Pts',(-5.72471356214735,-5.03570890150477,
-13.4633046799478));
#42873=CARTESIAN_POINT('Ctrl Pts',(-5.72306575818266,-4.31359100517564,
-12.0712170809002));
#42874=CARTESIAN_POINT('Ctrl Pts',(-5.72038904755586,-3.83840722052135,
-10.6678390314501));
#42875=CARTESIAN_POINT('Ctrl Pts',(-5.71829743871595,-3.65952910665459,
-9.72608608764783));
#42876=CARTESIAN_POINT('Ctrl Pts',(-5.71724185222974,-3.60559726864913,
-9.29489095839975));
#42877=CARTESIAN_POINT('Ctrl Pts',(-5.90002717726106,-9.63679765643431,
-17.3716665606242));
#42878=CARTESIAN_POINT('Ctrl Pts',(-5.90064014424208,-9.20180701959731,
-17.1757873397771));
#42879=CARTESIAN_POINT('Ctrl Pts',(-5.90174038137585,-8.32197996147983,
-16.7034325008754));
#42880=CARTESIAN_POINT('Ctrl Pts',(-5.90280993369199,-7.10225209295494,
-15.7991883436704));
#42881=CARTESIAN_POINT('Ctrl Pts',(-5.90294519188033,-6.00412592355956,
-14.6922158654566));
#42882=CARTESIAN_POINT('Ctrl Pts',(-5.90230921958852,-5.08548723943647,
-13.4325714280488));
#42883=CARTESIAN_POINT('Ctrl Pts',(-5.9009135213621,-4.36673044058498,-12.048661604341));
#42884=CARTESIAN_POINT('Ctrl Pts',(-5.89863582611894,-3.89298817613705,
-10.6534829599988));
#42885=CARTESIAN_POINT('Ctrl Pts',(-5.89685148833867,-3.71409960335627,
-9.71696543058244));
#42886=CARTESIAN_POINT('Ctrl Pts',(-5.89594501973261,-3.65996390017634,
-9.2881333735693));
#42887=CARTESIAN_POINT('Ctrl Pts',(-6.00727960514337,-9.69953310260925,
-17.2318896281666));
#42888=CARTESIAN_POINT('Ctrl Pts',(-6.00760257008453,-9.27115360051871,
-17.0387552962051));
#42889=CARTESIAN_POINT('Ctrl Pts',(-6.00818063783358,-8.40460281232898,
-16.573090076404));
#42890=CARTESIAN_POINT('Ctrl Pts',(-6.00873745913476,-7.20353593893208,
-15.6822226095155));
#42891=CARTESIAN_POINT('Ctrl Pts',(-6.00880782934474,-6.12189755288578,
-14.5918038255627));
#42892=CARTESIAN_POINT('Ctrl Pts',(-6.00847681114424,-5.2169700002139,-13.3513285148959));
#42893=CARTESIAN_POINT('Ctrl Pts',(-6.00774820020079,-4.50853269808651,
-11.9883509755523));
#42894=CARTESIAN_POINT('Ctrl Pts',(-6.00654575904665,-4.04115736338279,
-10.6143706750423));
#42895=CARTESIAN_POINT('Ctrl Pts',(-6.00559803258962,-3.86430082012095,
-9.691815921938));
#42896=CARTESIAN_POINT('Ctrl Pts',(-6.00510903930179,-3.81065842092309,
-9.26940249172137));
#42897=CARTESIAN_POINT('Ctrl Pts',(-5.99966802959142,-9.77609339016483,
-17.0613104586777));
#42898=CARTESIAN_POINT('Ctrl Pts',(-5.99963712428367,-9.35567454107366,
-16.8717652077172));
#42899=CARTESIAN_POINT('Ctrl Pts',(-5.99957893141052,-8.50506367644026,
-16.4146621757356));
#42900=CARTESIAN_POINT('Ctrl Pts',(-5.99951383159447,-7.3263647493401,-15.5403972571897));
#42901=CARTESIAN_POINT('Ctrl Pts',(-5.99950552107023,-6.2646607784291,-14.4700755533922));
#42902=CARTESIAN_POINT('Ctrl Pts',(-5.9995443574713,-5.37658001505559,-13.2526810833737));
#42903=CARTESIAN_POINT('Ctrl Pts',(-5.99962598905998,-4.68121720532413,
-11.9148600033795));
#42904=CARTESIAN_POINT('Ctrl Pts',(-5.99973691556681,-4.22254267934907,
-10.5664384725443));
#42905=CARTESIAN_POINT('Ctrl Pts',(-5.99981426292777,-4.04893496254998,
-9.66088439635348));
#42906=CARTESIAN_POINT('Ctrl Pts',(-5.99984101441889,-3.9962831894273,-9.24632985745589));
#42907=CARTESIAN_POINT('',(-5.99999988467789,-9.67863428828651,-17.0348543136794));
#42908=CARTESIAN_POINT('Origin',(-5.59998164336546,-9.67863961984266,-17.0348438488183));
#42909=CARTESIAN_POINT('Ctrl Pts',(-6.,-9.67863396518321,-17.0348526023082));
#42910=CARTESIAN_POINT('Ctrl Pts',(-6.,-9.24640194919319,-16.8355809092864));
#42911=CARTESIAN_POINT('Ctrl Pts',(-6.,-8.83275508583899,-16.6077872915085));
#42912=CARTESIAN_POINT('Ctrl Pts',(-6.,-8.43516132001025,-16.3499544374811));
#42913=CARTESIAN_POINT('Ctrl Pts',(-6.,-8.03756727297484,-16.092121401096));
#42914=CARTESIAN_POINT('Ctrl Pts',(-6.,-7.65602634617269,-15.8042490859695));
#42915=CARTESIAN_POINT('Ctrl Pts',(-6.,-7.29796322174819,-15.4912222292012));
#42916=CARTESIAN_POINT('Ctrl Pts',(-6.,-6.93990009732394,-15.1781953724331));
#42917=CARTESIAN_POINT('Ctrl Pts',(-6.,-6.6053147752773,-14.8400139740232));
#42918=CARTESIAN_POINT('Ctrl Pts',(-6.,-6.29607548316964,-14.4788351250848));
#42919=CARTESIAN_POINT('Ctrl Pts',(-6.,-5.98683619106177,-14.1176562761461));
#42920=CARTESIAN_POINT('Ctrl Pts',(-6.,-5.70294292889293,-13.733479976679));
#42921=CARTESIAN_POINT('Ctrl Pts',(-6.,-5.44842667128605,-13.331796225766));
#42922=CARTESIAN_POINT('Ctrl Pts',(-6.,-5.19391041367936,-12.9301124748532));
#42923=CARTESIAN_POINT('Ctrl Pts',(-6.,-4.9687711606346,-12.5109212724947));
#42924=CARTESIAN_POINT('Ctrl Pts',(-6.,-4.77466771540665,-12.0768285359646));
#42925=CARTESIAN_POINT('Ctrl Pts',(-6.,-4.58056427017856,-11.6427357994341));
#42926=CARTESIAN_POINT('Ctrl Pts',(-6.,-4.41749663276733,-11.1937415287322));
#42927=CARTESIAN_POINT('Ctrl Pts',(-6.,-4.28772377567829,-10.7378297759092));
#42928=CARTESIAN_POINT('Ctrl Pts',(-6.,-4.15795091858935,-10.2819180230865));
#42929=CARTESIAN_POINT('Ctrl Pts',(-6.,-4.06147284182256,-9.8190887881429));
#42930=CARTESIAN_POINT('Ctrl Pts',(-6.,-3.99788654320472,-9.34661202518238));
#42931=CARTESIAN_POINT('Origin',(-5.599999999997,-9.6786310860259,-17.0348569100619));
#42932=CARTESIAN_POINT('Origin',(-5.6,-9.67863108604804,-17.0348569101035));
#42933=CARTESIAN_POINT('Ctrl Pts',(-6.05070079238961,-6.2176939973095,-8.31864695491407));
#42934=CARTESIAN_POINT('Ctrl Pts',(-6.05139768547269,-6.23880305073253,
-8.30250772584274));
#42935=CARTESIAN_POINT('Ctrl Pts',(-6.04731850243085,-6.29402509020919,
-8.26303317773159));
#42936=CARTESIAN_POINT('Ctrl Pts',(-6.01624003938889,-6.39018722730729,
-8.20516961886834));
#42937=CARTESIAN_POINT('Ctrl Pts',(-5.94855011433123,-6.49933487298712,
-8.15385676121418));
#42938=CARTESIAN_POINT('Ctrl Pts',(-5.85055911347944,-6.60029897666562,
-8.12196082013419));
#42939=CARTESIAN_POINT('Ctrl Pts',(-5.76530777443809,-6.65832830405139,
-8.11641163255942));
#42940=CARTESIAN_POINT('Ctrl Pts',(-5.71755809134908,-6.68344389358587,
-8.11883822207412));
#42941=CARTESIAN_POINT('Ctrl Pts',(-5.71204816250035,-6.68624967619076,
-8.11918746206646));
#42942=CARTESIAN_POINT('Ctrl Pts',(-5.91199124611904,-6.04862265685342,
-8.09100626630052));
#42943=CARTESIAN_POINT('Ctrl Pts',(-5.91263110712145,-6.06761428475678,
-8.07647455597469));
#42944=CARTESIAN_POINT('Ctrl Pts',(-5.90889016285839,-6.11754050550086,
-8.04084303944076));
#42945=CARTESIAN_POINT('Ctrl Pts',(-5.8800819863844,-6.20535025391518,-7.98841262080049));
#42946=CARTESIAN_POINT('Ctrl Pts',(-5.81697232658341,-6.30576567345289,
-7.9419541048996));
#42947=CARTESIAN_POINT('Ctrl Pts',(-5.72538958464469,-6.39904806928683,
-7.91336636114985));
#42948=CARTESIAN_POINT('Ctrl Pts',(-5.64571477447322,-6.45276327292691,
-7.90880982817913));
#42949=CARTESIAN_POINT('Ctrl Pts',(-5.60114858206858,-6.47601774174994,
-7.91130704060933));
#42950=CARTESIAN_POINT('Ctrl Pts',(-5.59600687463879,-6.47861573314325,
-7.91165826841064));
#42951=CARTESIAN_POINT('Ctrl Pts',(-6.02851383329436,-5.86812573387379,
-7.8597274090204));
#42952=CARTESIAN_POINT('Ctrl Pts',(-6.02951717986534,-5.89741436718577,
-7.83734246590686));
#42953=CARTESIAN_POINT('Ctrl Pts',(-6.02361102927941,-5.97279895728111,
-7.78345987269494));
#42954=CARTESIAN_POINT('Ctrl Pts',(-5.98092154264836,-6.0997335165731,-7.70691568628475));
#42955=CARTESIAN_POINT('Ctrl Pts',(-5.89068578849719,-6.24049313343636,
-7.64049778117552));
#42956=CARTESIAN_POINT('Ctrl Pts',(-5.7617298699184,-6.36959713087669,-7.59964063210728));
#42957=CARTESIAN_POINT('Ctrl Pts',(-5.64952879318203,-6.44421982544224,
-7.5926595670497));
#42958=CARTESIAN_POINT('Ctrl Pts',(-5.58623246546378,-6.47685794718921,
-7.59598379230037));
#42959=CARTESIAN_POINT('Ctrl Pts',(-5.57892201417051,-6.48050945436716,
-7.596458488021));
#42960=CARTESIAN_POINT('Ctrl Pts',(-6.32392448294239,-5.79446202133885,
-7.77634070202551));
#42961=CARTESIAN_POINT('Ctrl Pts',(-6.32547368216801,-5.83971563927917,
-7.74178710117615));
#42962=CARTESIAN_POINT('Ctrl Pts',(-6.31631749247212,-5.9546328246946,-7.65951716937307));
#42963=CARTESIAN_POINT('Ctrl Pts',(-6.25268993559297,-6.14253537363754,
-7.54511130591315));
#42964=CARTESIAN_POINT('Ctrl Pts',(-6.12139435816593,-6.34628266567896,
-7.44699738981473));
#42965=CARTESIAN_POINT('Ctrl Pts',(-5.93577020055708,-6.53124176918286,
-7.38633197376381));
#42966=CARTESIAN_POINT('Ctrl Pts',(-5.77425080851983,-6.63829527819499,
-7.37509770946464));
#42967=CARTESIAN_POINT('Ctrl Pts',(-5.6825824374102,-6.68541379044458,-7.37946349065171));
#42968=CARTESIAN_POINT('Ctrl Pts',(-5.67198720706453,-6.69068987183275,
-7.3801022400051));
#42969=CARTESIAN_POINT('',(-5.73278770456533,-6.6558833922326,-8.10254681684203));
#42970=CARTESIAN_POINT('',(-5.72001815523952,-6.64700891660902,-7.39409230498819));
#42971=CARTESIAN_POINT('Origin',(-5.8987602805625,-6.95917384373578,-7.74135788191406));
#42972=CARTESIAN_POINT('',(-5.99999999681378,-6.44014573036754,-7.42970716684666));
#42973=CARTESIAN_POINT('Ctrl Pts',(-6.0000000832888,-6.44014586670658,-7.42970731664913));
#42974=CARTESIAN_POINT('Ctrl Pts',(-5.95915137667849,-6.47968145316765,
-7.41730531005402));
#42975=CARTESIAN_POINT('Ctrl Pts',(-5.91542827660156,-6.5166771191331,-7.40809722880095));
#42976=CARTESIAN_POINT('Ctrl Pts',(-5.868798937096,-6.55119699478441,-7.40209707843446));
#42977=CARTESIAN_POINT('Ctrl Pts',(-5.82216959558716,-6.58571687191874,
-7.39609692781019));
#42978=CARTESIAN_POINT('Ctrl Pts',(-5.77263377981968,-6.6177605887956,-7.39330427821582));
#42979=CARTESIAN_POINT('Ctrl Pts',(-5.72001867762135,-6.64700982892112,
-7.39409331981127));
#42980=CARTESIAN_POINT('',(-5.99998808311055,-6.09546019408016,-8.13557730954211));
#42981=CARTESIAN_POINT('Ctrl Pts',(-5.99998808311055,-6.09546019408016,
-8.13557730954211));
#42982=CARTESIAN_POINT('Ctrl Pts',(-5.99998579341257,-6.09905757126837,
-8.1076121115612));
#42983=CARTESIAN_POINT('Ctrl Pts',(-5.99998684302836,-6.10332349437861,
-8.08015310005243));
#42984=CARTESIAN_POINT('Ctrl Pts',(-5.99998299213941,-6.10828599559105,
-8.05321832362444));
#42985=CARTESIAN_POINT('Ctrl Pts',(-5.99998186316054,-6.10974086979519,
-8.04532175902083));
#42986=CARTESIAN_POINT('Ctrl Pts',(-5.99998012470112,-6.11125530650231,
-8.03747020572751));
#42987=CARTESIAN_POINT('Ctrl Pts',(-5.99997728564091,-6.11282931570554,
-8.02966396994754));
#42988=CARTESIAN_POINT('Ctrl Pts',(-5.99996366274466,-6.12038201360534,
-7.99220666635636));
#42989=CARTESIAN_POINT('Ctrl Pts',(-5.99992845213204,-6.12930815877995,
-7.95579590653871));
#42990=CARTESIAN_POINT('Ctrl Pts',(-5.99991578864617,-6.13957445794852,
-7.92039221214192));
#42991=CARTESIAN_POINT('Ctrl Pts',(-5.99991509179514,-6.14013939569574,
-7.91844400441608));
#42992=CARTESIAN_POINT('Ctrl Pts',(-5.99991445763287,-6.14070839032029,
-7.91649883611599));
#42993=CARTESIAN_POINT('Ctrl Pts',(-5.99991389241991,-6.14128143696332,
-7.91455669723407));
#42994=CARTESIAN_POINT('Ctrl Pts',(-5.99990495768377,-6.15034000586679,
-7.88385588239449));
#42995=CARTESIAN_POINT('Ctrl Pts',(-5.99990284924714,-6.16043170965493,
-7.85392609166195));
#42996=CARTESIAN_POINT('Ctrl Pts',(-5.99990385986942,-6.17154887581139,
-7.82477895973108));
#42997=CARTESIAN_POINT('Ctrl Pts',(-5.99990456954584,-6.17935554187285,
-7.8043113403368));
#42998=CARTESIAN_POINT('Ctrl Pts',(-5.99990725999096,-6.18766785808837,
-7.78422897762939));
#42999=CARTESIAN_POINT('Ctrl Pts',(-5.99991517244305,-6.1964942566548,-7.76452836981471));
#43000=CARTESIAN_POINT('Ctrl Pts',(-5.999918104499,-6.1997649866577,-7.75722806850045));
#43001=CARTESIAN_POINT('Ctrl Pts',(-5.9999261926437,-6.20321482930646,-7.74973181446826));
#43002=CARTESIAN_POINT('Ctrl Pts',(-5.99993157519488,-6.20670228942552,
-7.74238378435717));
#43003=CARTESIAN_POINT('Ctrl Pts',(-5.99993702627722,-6.21023415222328,
-7.73494219841775));
#43004=CARTESIAN_POINT('Ctrl Pts',(-5.99993942941342,-6.21380446476958,
-7.72765294100298));
#43005=CARTESIAN_POINT('Ctrl Pts',(-5.99994447142085,-6.21721465616354,
-7.72086215695556));
#43006=CARTESIAN_POINT('Ctrl Pts',(-5.99994530679784,-6.21777966831269,
-7.71973703667761));
#43007=CARTESIAN_POINT('Ctrl Pts',(-5.99994624919116,-6.21834017787097,
-7.7186255700337));
#43008=CARTESIAN_POINT('Ctrl Pts',(-5.99994736554133,-6.21889515985152,
-7.71752929521157));
#43009=CARTESIAN_POINT('Ctrl Pts',(-5.99997424180662,-6.23225641805852,
-7.69113634647166));
#43010=CARTESIAN_POINT('Ctrl Pts',(-5.99996041212331,-6.24653889545146,
-7.66574508274203));
#43011=CARTESIAN_POINT('Ctrl Pts',(-5.99993586626681,-6.26166900270897,
-7.6413218863139));
#43012=CARTESIAN_POINT('Ctrl Pts',(-5.99991529890311,-6.27434676030037,
-7.6208573014532));
#43013=CARTESIAN_POINT('Ctrl Pts',(-5.99988811606785,-6.2876205692234,-7.60107176789985));
#43014=CARTESIAN_POINT('Ctrl Pts',(-5.99987116820446,-6.30147515965944,
-7.58195086878649));
#43015=CARTESIAN_POINT('Ctrl Pts',(-5.99985202391289,-6.31712529282017,
-7.56035191797967));
#43016=CARTESIAN_POINT('Ctrl Pts',(-5.99984750492891,-6.33351668140582,
-7.53959965094863));
#43017=CARTESIAN_POINT('Ctrl Pts',(-5.99986528484166,-6.35066442453289,
-7.51969184647213));
#43018=CARTESIAN_POINT('Ctrl Pts',(-5.99988250987291,-6.36727701511488,
-7.50040533146525));
#43019=CARTESIAN_POINT('Ctrl Pts',(-5.99992124591386,-6.38460059983747,
-7.48191118790163));
#43020=CARTESIAN_POINT('Ctrl Pts',(-5.99995587754498,-6.40266648904051,
-7.4642385727826));
#43021=CARTESIAN_POINT('Ctrl Pts',(-5.99997917503714,-6.41481982685424,
-7.45234979946069));
#43022=CARTESIAN_POINT('Ctrl Pts',(-5.99999991524962,-6.42730946144769,
-7.44083350199229));
#43023=CARTESIAN_POINT('Ctrl Pts',(-5.99999992273984,-6.44014559311225,
-7.4297070085014));
#43024=CARTESIAN_POINT('Ctrl Pts',(-5.99998808311055,-6.09546019408016,
-8.13557730954211));
#43025=CARTESIAN_POINT('Ctrl Pts',(-5.99998551891527,-6.11109455318528,
-8.12979418173387));
#43026=CARTESIAN_POINT('Ctrl Pts',(-5.9992401947774,-6.12784559555232,-8.12408493904144));
#43027=CARTESIAN_POINT('Ctrl Pts',(-5.99754680984414,-6.14566703424288,
-8.1185774313553));
#43028=CARTESIAN_POINT('Ctrl Pts',(-5.99687196598229,-6.15276919292727,
-8.11638259208213));
#43029=CARTESIAN_POINT('Ctrl Pts',(-5.99604634715655,-6.16004095183898,
-8.11422011573065));
#43030=CARTESIAN_POINT('Ctrl Pts',(-5.99505598209878,-6.16747772038915,
-8.11209946841976));
#43031=CARTESIAN_POINT('Ctrl Pts',(-5.99264929774847,-6.18554979830235,
-8.10694608719373));
#43032=CARTESIAN_POINT('Ctrl Pts',(-5.9892694657102,-6.20459955905458,-8.10203798932087));
#43033=CARTESIAN_POINT('Ctrl Pts',(-5.98476114151186,-6.22452690538448,
-8.0975132784811));
#43034=CARTESIAN_POINT('Ctrl Pts',(-5.98055933700287,-6.24309939706376,
-8.09329620145381));
#43035=CARTESIAN_POINT('Ctrl Pts',(-5.97537763983944,-6.2624343485505,-8.08941191476389));
#43036=CARTESIAN_POINT('Ctrl Pts',(-5.96908598759027,-6.2824110980282,-8.08599595429554));
#43037=CARTESIAN_POINT('Ctrl Pts',(-5.96754611749363,-6.28730037002395,
-8.08515990437285));
#43038=CARTESIAN_POINT('Ctrl Pts',(-5.96593972255001,-6.29222788468966,
-8.08435203394631));
#43039=CARTESIAN_POINT('Ctrl Pts',(-5.96426481096664,-6.29719146243715,
-8.08357459006554));
#43040=CARTESIAN_POINT('Ctrl Pts',(-5.96381007642168,-6.29853906209006,
-8.08336351588535));
#43041=CARTESIAN_POINT('Ctrl Pts',(-5.9633502911682,-6.29988931898542,-8.08315468514074));
#43042=CARTESIAN_POINT('Ctrl Pts',(-5.96288542938708,-6.30124219280347,
-8.08294813476418));
#43043=CARTESIAN_POINT('Ctrl Pts',(-5.9582989837985,-6.3145899929598,-8.08091025576045));
#43044=CARTESIAN_POINT('Ctrl Pts',(-5.95321825970403,-6.32819323848442,
-8.07909402244848));
#43045=CARTESIAN_POINT('Ctrl Pts',(-5.94761928847918,-6.34200851301402,
-8.0775370834204));
#43046=CARTESIAN_POINT('Ctrl Pts',(-5.94481980286676,-6.34891615027881,
-8.07675861390635));
#43047=CARTESIAN_POINT('Ctrl Pts',(-5.94189071345292,-6.3558767794314,-8.07604498720728));
#43048=CARTESIAN_POINT('Ctrl Pts',(-5.93882920449365,-6.36288396966655,
-8.07540138572607));
#43049=CARTESIAN_POINT('Ctrl Pts',(-5.93729845001401,-6.36638756478413,
-8.07507958498547));
#43050=CARTESIAN_POINT('Ctrl Pts',(-5.93573458735359,-6.36990279902876,
-8.07477529198379));
#43051=CARTESIAN_POINT('Ctrl Pts',(-5.93413726064459,-6.373428827563,-8.07448917805385));
#43052=CARTESIAN_POINT('Ctrl Pts',(-5.93307815068233,-6.37576676627447,
-8.07429946976698));
#43053=CARTESIAN_POINT('Ctrl Pts',(-5.93173234134964,-6.37870044829973,
-8.07407323849032));
#43054=CARTESIAN_POINT('Ctrl Pts',(-5.93063879363215,-6.38105333357039,
-8.07390055787731));
#43055=CARTESIAN_POINT('Ctrl Pts',(-5.93008307636399,-6.38224901891086,
-8.07381280532935));
#43056=CARTESIAN_POINT('Ctrl Pts',(-5.92959342492817,-6.38329503672707,
-8.07373826411038));
#43057=CARTESIAN_POINT('Ctrl Pts',(-5.92924452468266,-6.38403842738213,
-8.07368606009921));
#43058=CARTESIAN_POINT('Ctrl Pts',(-5.92334533252883,-6.39660764845899,
-8.07280339665307));
#43059=CARTESIAN_POINT('Ctrl Pts',(-5.91666161280742,-6.41008271491505,
-8.07210940739551));
#43060=CARTESIAN_POINT('Ctrl Pts',(-5.90905330569263,-6.42435950584694,
-8.07173091984199));
#43061=CARTESIAN_POINT('Ctrl Pts',(-5.90809031583021,-6.42616653134261,
-8.07168301435243));
#43062=CARTESIAN_POINT('Ctrl Pts',(-5.90711250287754,-6.4279863444395,-8.07164020169699));
#43063=CARTESIAN_POINT('Ctrl Pts',(-5.90611957366789,-6.42981868289155,
-8.07160277367536));
#43064=CARTESIAN_POINT('Ctrl Pts',(-5.89855598641619,-6.4437764269301,-8.0713176676431));
#43065=CARTESIAN_POINT('Ctrl Pts',(-5.89011476605191,-6.45846421800495,
-8.07134329748215));
#43066=CARTESIAN_POINT('Ctrl Pts',(-5.88068115795978,-6.47375412525542,
-8.07180866003445));
#43067=CARTESIAN_POINT('Ctrl Pts',(-5.8736586626388,-6.48513612258624,-8.07215508171257));
#43068=CARTESIAN_POINT('Ctrl Pts',(-5.86608628545536,-6.49685114602332,
-8.0727455237084));
#43069=CARTESIAN_POINT('Ctrl Pts',(-5.85791981639649,-6.50882979367172,
-8.07364182408336));
#43070=CARTESIAN_POINT('Ctrl Pts',(-5.84746905717488,-6.52415905794388,
-8.07478883380587));
#43071=CARTESIAN_POINT('Ctrl Pts',(-5.83604470384628,-6.53992227767247,
-8.07643553931398));
#43072=CARTESIAN_POINT('Ctrl Pts',(-5.82356408719711,-6.55593067209317,
-8.07873403133492));
#43073=CARTESIAN_POINT('Ctrl Pts',(-5.81185651825911,-6.57094750872356,
-8.08089015507022));
#43074=CARTESIAN_POINT('Ctrl Pts',(-5.79921850083814,-6.5861794471044,-8.08362064648541));
#43075=CARTESIAN_POINT('Ctrl Pts',(-5.78561695045326,-6.60144653247346,
-8.08704934513203));
#43076=CARTESIAN_POINT('Ctrl Pts',(-5.7728923678692,-6.6157292637136,-8.09025697645716));
#43077=CARTESIAN_POINT('Ctrl Pts',(-5.75932437550369,-6.63004293553971,
-8.09407553435004));
#43078=CARTESIAN_POINT('Ctrl Pts',(-5.74490778875738,-6.64420241550599,
-8.09862150095951));
#43079=CARTESIAN_POINT('Ctrl Pts',(-5.74093127011729,-6.64810801653422,
-8.09987541225473));
#43080=CARTESIAN_POINT('Ctrl Pts',(-5.73689033060084,-6.6520016430365,-8.10118476717543));
#43081=CARTESIAN_POINT('Ctrl Pts',(-5.73278520330964,-6.65587882437944,
-8.10255225722823));
#43082=CARTESIAN_POINT('Ctrl Pts',(-5.71725974766235,-6.24680066241192,
-7.76998179414862));
#43083=CARTESIAN_POINT('Ctrl Pts',(-5.7183153287713,-6.59326365452918,-8.03228739331712));
#43084=CARTESIAN_POINT('Ctrl Pts',(-5.7204069205709,-7.31940961941998,-8.65807896524696));
#43085=CARTESIAN_POINT('Ctrl Pts',(-5.72308359607531,-8.29718049086054,
-9.77129138847913));
#43086=CARTESIAN_POINT('Ctrl Pts',(-5.72473137529731,-9.14170426243484,
-11.0927069646456));
#43087=CARTESIAN_POINT('Ctrl Pts',(-5.725483124375,-9.77722228596547,-12.5261362769566));
#43088=CARTESIAN_POINT('Ctrl Pts',(-5.7253232146161,-10.1890896647104,-14.0392346326023));
#43089=CARTESIAN_POINT('Ctrl Pts',(-5.7240590756321,-10.362720345492,-15.5563820479767));
#43090=CARTESIAN_POINT('Ctrl Pts',(-5.72276355651685,-10.3310899414738,
-16.5600585885505));
#43091=CARTESIAN_POINT('Ctrl Pts',(-5.7220426403927,-10.2826264095249,-17.0373217476865));
#43092=CARTESIAN_POINT('Ctrl Pts',(-5.89595647066798,-6.21376083080576,
-7.81369164428259));
#43093=CARTESIAN_POINT('Ctrl Pts',(-5.89686291373834,-6.5580751590849,-8.07499205702994));
#43094=CARTESIAN_POINT('Ctrl Pts',(-5.89864718970208,-7.27968139022067,
-8.69817451202807));
#43095=CARTESIAN_POINT('Ctrl Pts',(-5.90092480081758,-8.25107147177759,
-9.80603802544213));
#43096=CARTESIAN_POINT('Ctrl Pts',(-5.90232044313017,-9.09019307701646,
-11.1204529998163));
#43097=CARTESIAN_POINT('Ctrl Pts',(-5.90295638986529,-9.72175698666846,
-12.5458378515269));
#43098=CARTESIAN_POINT('Ctrl Pts',(-5.90282113710503,-10.1313596816372,
-14.050327350289));
#43099=CARTESIAN_POINT('Ctrl Pts',(-5.90175163079886,-10.3045934944351,
-15.5587586508462));
#43100=CARTESIAN_POINT('Ctrl Pts',(-5.9006514436638,-10.2737520765702,-16.5568830510553));
#43101=CARTESIAN_POINT('Ctrl Pts',(-5.90003850788786,-10.2258942358848,
-17.0315309081517));
#43102=CARTESIAN_POINT('Ctrl Pts',(-6.00511198583713,-6.12219220459409,
-7.93483169827869));
#43103=CARTESIAN_POINT('Ctrl Pts',(-6.00560095016558,-6.46119445239523,
-8.19249553837079));
#43104=CARTESIAN_POINT('Ctrl Pts',(-6.00654860595358,-7.17172454535513,
-8.80693673850609));
#43105=CARTESIAN_POINT('Ctrl Pts',(-6.00775096201441,-8.12793979442155,
-9.89868707557194));
#43106=CARTESIAN_POINT('Ctrl Pts',(-6.00847951651781,-8.95409328932254,
-11.1936989420205));
#43107=CARTESIAN_POINT('Ctrl Pts',(-6.00881050940341,-9.57591183211347,
-12.5976250407049));
#43108=CARTESIAN_POINT('Ctrl Pts',(-6.00874014451152,-9.97942249726841,
-14.079558861051));
#43109=CARTESIAN_POINT('Ctrl Pts',(-6.00818336787537,-10.1504022323851,
-15.5651409909013));
#43110=CARTESIAN_POINT('Ctrl Pts',(-6.00760534674583,-10.1204055268136,
-16.5484230576379));
#43111=CARTESIAN_POINT('Ctrl Pts',(-6.00728240995462,-10.0734760765557,
-17.0159731176358));
#43112=CARTESIAN_POINT('Ctrl Pts',(-5.99984081826169,-6.00940195879855,
-8.08404669773291));
#43113=CARTESIAN_POINT('Ctrl Pts',(-5.99981404919679,-6.34209366151083,
-8.33692329269028));
#43114=CARTESIAN_POINT('Ctrl Pts',(-5.99973665501392,-7.03952549705589,
-8.94005087392584));
#43115=CARTESIAN_POINT('Ctrl Pts',(-5.99962568199747,-7.97795713266765,
-10.0114872699567));
#43116=CARTESIAN_POINT('Ctrl Pts',(-5.99954401869402,-8.78886222453736,
-11.2825987957422));
#43117=CARTESIAN_POINT('Ctrl Pts',(-5.9995051685709,-9.39911593306368,-12.6603955354204));
#43118=CARTESIAN_POINT('Ctrl Pts',(-5.99951348191174,-9.795189453441,-14.1150179548503));
#43119=CARTESIAN_POINT('Ctrl Pts',(-5.99957860547203,-9.96297502994334,
-15.5729285367099));
#43120=CARTESIAN_POINT('Ctrl Pts',(-5.99963682134737,-9.9335331720651,-16.538125769813));
#43121=CARTESIAN_POINT('Ctrl Pts',(-5.99966773997577,-9.88747576114577,
-16.9969875051557));
#43122=CARTESIAN_POINT('',(-5.99999997114735,-9.91329953294255,-16.8993693187113));
#43123=CARTESIAN_POINT('Ctrl Pts',(-6.,-6.09546019522424,-8.13557730902212));
#43124=CARTESIAN_POINT('Ctrl Pts',(-6.,-6.47284397492114,-8.42688307326569));
#43125=CARTESIAN_POINT('Ctrl Pts',(-6.,-6.82542683076759,-8.74185019941709));
#43126=CARTESIAN_POINT('Ctrl Pts',(-6.,-7.1553715768929,-9.08219270129307));
#43127=CARTESIAN_POINT('Ctrl Pts',(-6.,-7.48531632301845,-9.42253520316929));
#43128=CARTESIAN_POINT('Ctrl Pts',(-6.,-7.79262295942282,-9.78825308077012));
#43129=CARTESIAN_POINT('Ctrl Pts',(-6.,-8.07150656549643,-10.1733979628959));
#43130=CARTESIAN_POINT('Ctrl Pts',(-6.,-8.35039017156985,-10.5585428450215));
#43131=CARTESIAN_POINT('Ctrl Pts',(-6.,-8.60085074731254,-10.9631147316719));
#43132=CARTESIAN_POINT('Ctrl Pts',(-6.,-8.82146093334939,-11.3843741331592));
#43133=CARTESIAN_POINT('Ctrl Pts',(-6.,-9.0420711193864,-11.8056335346468));
#43134=CARTESIAN_POINT('Ctrl Pts',(-6.,-9.23283091571751,-12.2435804509713));
#43135=CARTESIAN_POINT('Ctrl Pts',(-6.,-9.39100132287916,-12.6919789565551));
#43136=CARTESIAN_POINT('Ctrl Pts',(-6.,-9.5491717300407,-13.1403774621387));
#43137=CARTESIAN_POINT('Ctrl Pts',(-6.,-9.67475274803281,-13.5992275569817));
#43138=CARTESIAN_POINT('Ctrl Pts',(-6.,-9.76681039167948,-14.0658327420193));
#43139=CARTESIAN_POINT('Ctrl Pts',(-6.,-9.85886803532621,-14.5324379270572));
#43140=CARTESIAN_POINT('Ctrl Pts',(-6.,-9.91740230462745,-15.0067982022898));
#43141=CARTESIAN_POINT('Ctrl Pts',(-6.,-9.94189523605327,-15.4800412501003));
#43142=CARTESIAN_POINT('Ctrl Pts',(-6.,-9.9663881501513,-15.95328396311));
#43143=CARTESIAN_POINT('Ctrl Pts',(-6.,-9.95683977453971,-16.4254094502785));
#43144=CARTESIAN_POINT('Ctrl Pts',(-6.,-9.91329811959712,-16.8993691888704));
#43145=CARTESIAN_POINT('',(-5.736443569433,-10.2877321037677,-16.9337809547651));
#43146=CARTESIAN_POINT('Origin',(-5.5999816381251,-9.91328781245259,-16.8993685785925));
#43147=CARTESIAN_POINT('Ctrl Pts',(-5.732787929952,-6.65588380271171,-8.10254632761798));
#43148=CARTESIAN_POINT('Ctrl Pts',(-5.73461480971849,-7.28539041071228,
-8.63201072144939));
#43149=CARTESIAN_POINT('Ctrl Pts',(-5.73605973940586,-7.85267746104921,
-9.23785131481548));
#43150=CARTESIAN_POINT('Ctrl Pts',(-5.73818934991676,-8.82745379673076,
-10.569912416548));
#43151=CARTESIAN_POINT('Ctrl Pts',(-5.73887403074029,-9.23545520213591,
-11.2957033768654));
#43152=CARTESIAN_POINT('Ctrl Pts',(-5.73948314352351,-9.86673752911049,
-12.8258684638728));
#43153=CARTESIAN_POINT('Ctrl Pts',(-5.7394075754832,-10.0903327788716,-13.630101648187));
#43154=CARTESIAN_POINT('Ctrl Pts',(-5.73849619057915,-10.3386823729398,
-15.2703412948045));
#43155=CARTESIAN_POINT('Ctrl Pts',(-5.73766037378285,-10.3633358173586,
-16.1063565589225));
#43156=CARTESIAN_POINT('Ctrl Pts',(-5.73644356975675,-10.2877321238833,
-16.9337807346159));
#43157=CARTESIAN_POINT('Origin',(-5.599999999997,-9.91330329119812,-16.8993688492357));
#43158=CARTESIAN_POINT('',(-5.593361696257,-10.1144356127388,-17.245059060506));
#43159=CARTESIAN_POINT('Origin',(-5.599999999997,-9.91330329119812,-16.8993688492357));
#43160=CARTESIAN_POINT('Origin',(-5.6,-9.91330329122126,-16.8993688492756));
#43161=CARTESIAN_POINT('Ctrl Pts',(-5.59335880963394,-10.1144382223412,
-17.2450574867612));
#43162=CARTESIAN_POINT('Ctrl Pts',(-5.59335897597996,-10.1110305794363,
-17.2470401530682));
#43163=CARTESIAN_POINT('Ctrl Pts',(-5.59336249921667,-10.0355852078339,
-17.290921844848));
#43164=CARTESIAN_POINT('Ctrl Pts',(-5.59336249921667,-9.95658496883865,
-17.3365326540989));
#43165=CARTESIAN_POINT('Ctrl Pts',(-5.59335897597996,-9.88085962320038,
-17.3799294166115));
#43166=CARTESIAN_POINT('Ctrl Pts',(-5.59335880963394,-9.87743876235887,
-17.3818891887806));
#43167=CARTESIAN_POINT('Ctrl Pts',(-5.8307400439972,-10.1164205431219,-17.2484645412161));
#43168=CARTESIAN_POINT('Ctrl Pts',(-5.83074021197856,-10.1130125214895,
-17.2504473136498));
#43169=CARTESIAN_POINT('Ctrl Pts',(-5.83074376985082,-10.0375588131129,
-17.2943314352281));
#43170=CARTESIAN_POINT('Ctrl Pts',(-5.83074376985082,-9.95855095808477,
-17.3399466416001));
#43171=CARTESIAN_POINT('Ctrl Pts',(-5.83074021197856,-9.88281933979065,
-17.3833494090707));
#43172=CARTESIAN_POINT('Ctrl Pts',(-5.8307400439972,-9.87939819767686,-17.3853094561641));
#43173=CARTESIAN_POINT('Ctrl Pts',(-6.0000034748831,-10.0326983105079,-17.1045694621535));
#43174=CARTESIAN_POINT('Ctrl Pts',(-6.0000035736193,-10.0293041517827,-17.106544087307));
#43175=CARTESIAN_POINT('Ctrl Pts',(-6.00000566486658,-9.95415740055512,
-17.1502479470959));
#43176=CARTESIAN_POINT('Ctrl Pts',(-6.00000566486658,-9.87547170337369,
-17.1956771555441));
#43177=CARTESIAN_POINT('Ctrl Pts',(-6.0000035736193,-9.80004967494144,-17.2389042212266));
#43178=CARTESIAN_POINT('Ctrl Pts',(-6.0000034748831,-9.79664252003289,-17.2408563363306));
#43179=CARTESIAN_POINT('Ctrl Pts',(-5.9999999999769,-9.91330295482212,-16.8993622715432));
#43180=CARTESIAN_POINT('Ctrl Pts',(-5.99999999996752,-9.90992861632663,
-16.9013253647287));
#43181=CARTESIAN_POINT('Ctrl Pts',(-5.99999999976692,-9.83522068214657,
-16.9447739934751));
#43182=CARTESIAN_POINT('Ctrl Pts',(-5.99999999976692,-9.75699439892162,
-16.98993795915));
#43183=CARTESIAN_POINT('Ctrl Pts',(-5.99999999996752,-9.68201281558226,
-17.0329126136425));
#43184=CARTESIAN_POINT('Ctrl Pts',(-5.9999999999769,-9.67862555776588,-17.034853329908));
#43185=CARTESIAN_POINT('Origin',(-5.47627053108701,8.61179369525734,14.9160892206269));
#43186=CARTESIAN_POINT('Ctrl Pts',(-6.00000000001697,-9.91329802718485,
-16.8993701947934));
#43187=CARTESIAN_POINT('Ctrl Pts',(-6.00000000001005,-9.90992616536128,
-16.9013320391245));
#43188=CARTESIAN_POINT('Ctrl Pts',(-6.00000000000346,-9.90655400604935,
-16.9032934158647));
#43189=CARTESIAN_POINT('Ctrl Pts',(-5.9999999999973,-9.90318155035885,-16.905254322156));
#43190=CARTESIAN_POINT('Ctrl Pts',(-5.99999999993207,-9.86751358933604,
-16.9259933727434));
#43191=CARTESIAN_POINT('Ctrl Pts',(-5.99999999990816,-9.83181247294484,
-16.9466797991169));
#43192=CARTESIAN_POINT('Ctrl Pts',(-5.99999999990816,-9.79607949297214,
-16.9673102431511));
#43193=CARTESIAN_POINT('Ctrl Pts',(-5.99999999990816,-9.76034664910772,
-16.9879406086032));
#43194=CARTESIAN_POINT('Ctrl Pts',(-5.99999999993208,-9.72458194169243,
-17.0085149922644));
#43195=CARTESIAN_POINT('Ctrl Pts',(-5.9999999999973,-9.68878892570765,-17.0290339621738));
#43196=CARTESIAN_POINT('Ctrl Pts',(-6.00000000000347,-9.68540449666689,
-17.0309741450765));
#43197=CARTESIAN_POINT('Ctrl Pts',(-6.00000000001005,-9.68201981452002,
-17.0329138325687));
#43198=CARTESIAN_POINT('Ctrl Pts',(-6.00000000001698,-9.67863488229806,
-17.0348530251248));
#43199=CARTESIAN_POINT('Ctrl Pts',(-5.67775659312587,-10.3018870984969,
-17.1369879289495));
#43200=CARTESIAN_POINT('Ctrl Pts',(-3.78517106208391,-11.0756618795401,
-16.643292974773));
#43201=CARTESIAN_POINT('Ctrl Pts',(-2.07379858077616E-10,-11.843298151568,
-16.1396478044549));
#43202=CARTESIAN_POINT('Ctrl Pts',(3.78517106166931,-11.0756618796282,-16.6432929747198));
#43203=CARTESIAN_POINT('Ctrl Pts',(5.67775659250446,-10.3018870987529,-17.1369879287883));
#43204=CARTESIAN_POINT('Ctrl Pts',(-5.67775659312587,-10.1072397989495,
-17.2516485514189));
#43205=CARTESIAN_POINT('Ctrl Pts',(-3.78517106208391,-10.3778358613942,
-17.0589591624347));
#43206=CARTESIAN_POINT('Ctrl Pts',(-2.07379858077616E-10,-10.7266017361378,
-16.9925638790986));
#43207=CARTESIAN_POINT('Ctrl Pts',(3.78517106166931,-10.3778358614304,-17.0589591624264));
#43208=CARTESIAN_POINT('Ctrl Pts',(5.67775659250446,-10.1072397990368,-17.2516485513547));
#43209=CARTESIAN_POINT('Ctrl Pts',(-5.67775659312587,-9.91157799214669,
-17.3647063741836));
#43210=CARTESIAN_POINT('Ctrl Pts',(-3.78517106208391,-9.67397381460403,
-17.4658518041024));
#43211=CARTESIAN_POINT('Ctrl Pts',(-2.07379858077616E-10,-9.51037124759094,
-17.7031909445496));
#43212=CARTESIAN_POINT('Ctrl Pts',(3.78517106166931,-9.67397381458855,-17.4658518041304));
#43213=CARTESIAN_POINT('Ctrl Pts',(5.67775659250446,-9.91157799207137,-17.3647063742117));
#43214=CARTESIAN_POINT('Ctrl Pts',(-5.67775659312587,-9.71502995626686,
-17.4760873358231));
#43215=CARTESIAN_POINT('Ctrl Pts',(-3.78517106208391,-8.96547267303902,
-17.8631643796455));
#43216=CARTESIAN_POINT('Ctrl Pts',(-2.07379858077616E-10,-8.21962531101494,
-18.2570844908793));
#43217=CARTESIAN_POINT('Ctrl Pts',(3.78517106166931,-8.96547267295871,-17.8631643796807));
#43218=CARTESIAN_POINT('Ctrl Pts',(5.67775659250446,-9.71502995601854,-17.4760873359463));
#43219=CARTESIAN_POINT('Ctrl Pts',(-5.59336169625719,-10.1144356127329,
-17.2450590604958));
#43220=CARTESIAN_POINT('Ctrl Pts',(-5.58012472829267,-10.1196353101486,
-17.2417795393872));
#43221=CARTESIAN_POINT('Ctrl Pts',(-5.56080272167237,-10.1272212315458,
-17.236996622306));
#43222=CARTESIAN_POINT('Ctrl Pts',(-5.53535951912591,-10.1371328509956,
-17.2307531058563));
#43223=CARTESIAN_POINT('Ctrl Pts',(-5.51000522085286,-10.1470098370174,
-17.2245314056576));
#43224=CARTESIAN_POINT('Ctrl Pts',(-5.4785722740891,-10.1591964229874,-17.2168593627599));
#43225=CARTESIAN_POINT('Ctrl Pts',(-5.44100421609337,-10.1735931464556,
-17.2078052457423));
#43226=CARTESIAN_POINT('Ctrl Pts',(-5.4135757571343,-10.1841042018537,-17.201194830132));
#43227=CARTESIAN_POINT('Ctrl Pts',(-5.38287654760146,-10.1957925666765,
-17.193848248765));
#43228=CARTESIAN_POINT('Ctrl Pts',(-5.34887846376144,-10.2086053972353,
-17.1858004892764));
#43229=CARTESIAN_POINT('Ctrl Pts',(-5.30328327342022,-10.2257888200095,
-17.1750075537855));
#43230=CARTESIAN_POINT('Ctrl Pts',(-5.25175535625055,-10.2449963320756,
-17.1629524969779));
#43231=CARTESIAN_POINT('Ctrl Pts',(-5.19421238137895,-10.2660648138751,
-17.149741746653));
#43232=CARTESIAN_POINT('Ctrl Pts',(-5.15775456135626,-10.2794132881121,
-17.1413717386931));
#43233=CARTESIAN_POINT('Ctrl Pts',(-5.11888187196832,-10.2935079656825,
-17.132538302818));
#43234=CARTESIAN_POINT('Ctrl Pts',(-5.07757050664895,-10.3082982014974,
-17.1232736070199));
#43235=CARTESIAN_POINT('Ctrl Pts',(-5.01427929152024,-10.3309576316452,
-17.1090795988983));
#43236=CARTESIAN_POINT('Ctrl Pts',(-4.94526457275114,-10.3552518085848,
-17.0938720536587));
#43237=CARTESIAN_POINT('Ctrl Pts',(-4.8704300836545,-10.3809642378146,-17.0777883362319));
#43238=CARTESIAN_POINT('Ctrl Pts',(-4.84061248884309,-10.3912092839911,
-17.0713798235918));
#43239=CARTESIAN_POINT('Ctrl Pts',(-4.80987082608312,-10.4016790077201,
-17.0648324870689));
#43240=CARTESIAN_POINT('Ctrl Pts',(-4.77819856291882,-10.4123577253344,
-17.0581561389736));
#43241=CARTESIAN_POINT('Ctrl Pts',(-4.7010630993418,-10.4383649553613,-17.0418963850475));
#43242=CARTESIAN_POINT('Ctrl Pts',(-4.61840846666524,-10.4656148338015,
-17.0248696191768));
#43243=CARTESIAN_POINT('Ctrl Pts',(-4.53013413338453,-10.4938511480454,
-17.0072368403959));
#43244=CARTESIAN_POINT('Ctrl Pts',(-4.50292955811853,-10.5025530765396,
-17.0018027324319));
#43245=CARTESIAN_POINT('Ctrl Pts',(-4.4751911941991,-10.5113483768928,-16.9963112527045));
#43246=CARTESIAN_POINT('Ctrl Pts',(-4.44691597455289,-10.520228683786,-16.9907676180755));
#43247=CARTESIAN_POINT('Ctrl Pts',(-4.35781070905515,-10.5482136866724,
-16.9732976552732));
#43248=CARTESIAN_POINT('Ctrl Pts',(-4.26337415633484,-10.5770461790196,
-16.9553077638445));
#43249=CARTESIAN_POINT('Ctrl Pts',(-4.16350817952473,-10.6064366031141,
-16.9369792766364));
#43250=CARTESIAN_POINT('Ctrl Pts',(-4.13544195081837,-10.6146964568777,
-16.9318282579386));
#43251=CARTESIAN_POINT('Ctrl Pts',(-4.10694687152408,-10.6230001091607,
-16.9266506566067));
#43252=CARTESIAN_POINT('Ctrl Pts',(-4.07802072640047,-10.6313404886027,
-16.921450882072));
#43253=CARTESIAN_POINT('Ctrl Pts',(-3.98959649917496,-10.6568361640123,
-16.9055557103159));
#43254=CARTESIAN_POINT('Ctrl Pts',(-3.89714408356194,-10.6826770133847,
-16.889452138432));
#43255=CARTESIAN_POINT('Ctrl Pts',(-3.80060148524953,-10.7086443711872,
-16.8732769081817));
#43256=CARTESIAN_POINT('Ctrl Pts',(-3.75616521987444,-10.7205965293285,
-16.8658318338159));
#43257=CARTESIAN_POINT('Ctrl Pts',(-3.71086243888832,-10.7325751201715,
-16.8583718019914));
#43258=CARTESIAN_POINT('Ctrl Pts',(-3.66468717718357,-10.7445568543748,
-16.8509113382743));
#43259=CARTESIAN_POINT('Ctrl Pts',(-3.62904937723011,-10.7538042875428,
-16.845153395521));
#43260=CARTESIAN_POINT('Ctrl Pts',(-3.59289186918105,-10.7630535677352,
-16.8393952106142));
#43261=CARTESIAN_POINT('Ctrl Pts',(-3.5562120702994,-10.7722935290167,-16.8336437594243));
#43262=CARTESIAN_POINT('Ctrl Pts',(-3.51410949029397,-10.782899536164,-16.8270420074723));
#43263=CARTESIAN_POINT('Ctrl Pts',(-3.47131870452021,-10.7934934543348,
-16.8204490092829));
#43264=CARTESIAN_POINT('Ctrl Pts',(-3.42783597889092,-10.8040574386497,
-16.813875902478));
#43265=CARTESIAN_POINT('Ctrl Pts',(-3.40609461607628,-10.8093394308071,
-16.8105893490756));
#43266=CARTESIAN_POINT('Ctrl Pts',(-3.3841802682972,-10.8146139394134,-16.8073077683825));
#43267=CARTESIAN_POINT('Ctrl Pts',(-3.36209246612069,-10.8198786844039,
-16.8040325823261));
#43268=CARTESIAN_POINT('Ctrl Pts',(-3.35104856503244,-10.8225110568992,
-16.8023949892978));
#43269=CARTESIAN_POINT('Ctrl Pts',(-3.33996130034482,-10.825140988483,-16.8007589949167));
#43270=CARTESIAN_POINT('Ctrl Pts',(-3.32883061462407,-10.8277681893696,
-16.7991247798285));
#43271=CARTESIAN_POINT('Ctrl Pts',(-3.3232652717637,-10.8290817898129,-16.7983076722845));
#43272=CARTESIAN_POINT('Ctrl Pts',(-3.31768907364504,-10.8303947075814,
-16.7974910095628));
#43273=CARTESIAN_POINT('Ctrl Pts',(-3.31210201314107,-10.831706906117,-16.7966748144487));
#43274=CARTESIAN_POINT('Ctrl Pts',(-3.30651495263711,-10.8330191046525,
-16.7958586193346));
#43275=CARTESIAN_POINT('Ctrl Pts',(-3.30209405058536,-10.8340555250056,
-16.7952139715887));
#43276=CARTESIAN_POINT('Ctrl Pts',(-3.29530823736295,-10.8356413073638,
-16.7942276547745));
#43277=CARTESIAN_POINT('Ctrl Pts',(-3.26371351550637,-10.8430247042966,
-16.7896353672494));
#43278=CARTESIAN_POINT('Ctrl Pts',(-3.23221976326762,-10.8502790172281,
-16.7851240198793));
#43279=CARTESIAN_POINT('Ctrl Pts',(-3.20082837941875,-10.857405906264,-16.7806925395476));
#43280=CARTESIAN_POINT('Ctrl Pts',(-3.02529692313373,-10.8972573896286,
-16.755912994948));
#43281=CARTESIAN_POINT('Ctrl Pts',(-2.85296934939383,-10.9331235998,-16.7336312409334));
#43282=CARTESIAN_POINT('Ctrl Pts',(-2.68408332988402,-10.9653143544167,
-16.7136486696483));
#43283=CARTESIAN_POINT('Ctrl Pts',(-2.50184473255019,-11.0000501956988,
-16.6920862231373));
#43284=CARTESIAN_POINT('Ctrl Pts',(-2.32361410469579,-11.0305070294388,
-16.6732004871531));
#43285=CARTESIAN_POINT('Ctrl Pts',(-2.14965775603431,-11.0571033277888,
-16.656724449575));
#43286=CARTESIAN_POINT('Ctrl Pts',(-2.13682704056364,-11.059065024153,-16.6555092059126));
#43287=CARTESIAN_POINT('Ctrl Pts',(-2.12401955526259,-11.0610057211373,
-16.6543070705806));
#43288=CARTESIAN_POINT('Ctrl Pts',(-2.11123539610953,-11.0629255879676,
-16.6531179359837));
#43289=CARTESIAN_POINT('Ctrl Pts',(-1.93625472004346,-11.0892033894171,
-16.6368418889479));
#43290=CARTESIAN_POINT('Ctrl Pts',(-1.76564841864985,-11.1115791716701,
-16.6230010120623));
#43291=CARTESIAN_POINT('Ctrl Pts',(-1.59964960282788,-11.1305058856433,
-16.6113061329138));
#43292=CARTESIAN_POINT('Ctrl Pts',(-1.55747658935585,-11.1353143329772,
-16.6083349774063));
#43293=CARTESIAN_POINT('Ctrl Pts',(-1.51560070218881,-11.1399001376491,
-16.6055023611455));
#43294=CARTESIAN_POINT('Ctrl Pts',(-1.47402524336761,-11.1442706692096,
-16.6028036016203));
#43295=CARTESIAN_POINT('Ctrl Pts',(-1.30954622475426,-11.161561175731,-16.59212688678));
#43296=CARTESIAN_POINT('Ctrl Pts',(-1.14977310552627,-11.1754837801492,
-16.5835441025915));
#43297=CARTESIAN_POINT('Ctrl Pts',(-0.994888664990271,-11.1865079150371,
-16.5767563060732));
#43298=CARTESIAN_POINT('Ctrl Pts',(-0.923054601787837,-11.1916208133989,
-16.5736081847873));
#43299=CARTESIAN_POINT('Ctrl Pts',(-0.852271416166483,-11.1961100038712,
-16.5708463593852));
#43300=CARTESIAN_POINT('Ctrl Pts',(-0.782553962123819,-11.2000210008409,
-16.5684420216565));
#43301=CARTESIAN_POINT('Ctrl Pts',(-0.633225991298167,-11.2083979740022,
-16.563292165295));
#43302=CARTESIAN_POINT('Ctrl Pts',(-0.488789985414885,-11.2141242830436,
-16.5597808094322));
#43303=CARTESIAN_POINT('Ctrl Pts',(-0.349367804833761,-11.2176486586726,
-16.5576200264894));
#43304=CARTESIAN_POINT('Ctrl Pts',(-0.262283841740363,-11.21985000566,-16.5562703879939));
#43305=CARTESIAN_POINT('Ctrl Pts',(-0.177155094990459,-11.2211917674833,
-16.5554480857796));
#43306=CARTESIAN_POINT('Ctrl Pts',(-0.0940037411538417,-11.2217777919864,
-16.5550872420774));
#43307=CARTESIAN_POINT('Ctrl Pts',(0.0408033095314012,-11.2227278695407,
-16.5545022332591));
#43308=CARTESIAN_POINT('Ctrl Pts',(0.170411322734702,-11.2216936622582,
-16.5551292702637));
#43309=CARTESIAN_POINT('Ctrl Pts',(0.294749910394146,-11.2191042251408,
-16.5567126569722));
#43310=CARTESIAN_POINT('Ctrl Pts',(0.343180997798596,-11.2180956142363,
-16.5573294014723));
#43311=CARTESIAN_POINT('Ctrl Pts',(0.390812982750298,-11.216850659833,-16.558091441881));
#43312=CARTESIAN_POINT('Ctrl Pts',(0.437643011558179,-11.2153932381847,
-16.5589844415374));
#43313=CARTESIAN_POINT('Ctrl Pts',(0.474088856675121,-11.2142589881103,
-16.5596794256746));
#43314=CARTESIAN_POINT('Ctrl Pts',(0.510048983107251,-11.2129960331579,
-16.5604537385973));
#43315=CARTESIAN_POINT('Ctrl Pts',(0.545522325941037,-11.2116152815913,
-16.5613008068628));
#43316=CARTESIAN_POINT('Ctrl Pts',(0.575342929721347,-11.2104545551952,
-16.5620128933228));
#43317=CARTESIAN_POINT('Ctrl Pts',(0.604819534315609,-11.2092105794191,
-16.5627763970877));
#43318=CARTESIAN_POINT('Ctrl Pts',(0.633951734731624,-11.2078897952418,
-16.5635874263828));
#43319=CARTESIAN_POINT('Ctrl Pts',(0.665845058433713,-11.2064438283492,
-16.564475324292));
#43320=CARTESIAN_POINT('Ctrl Pts',(0.697325520347901,-11.2049058146175,
-16.5654201765311));
#43321=CARTESIAN_POINT('Ctrl Pts',(0.728392804494912,-11.2032839637244,
-16.5664170102246));
#43322=CARTESIAN_POINT('Ctrl Pts',(0.743926446568417,-11.2024730382779,
-16.5669154270713));
#43323=CARTESIAN_POINT('Ctrl Pts',(0.759356794199198,-11.2016411533226,
-16.5674268389585));
#43324=CARTESIAN_POINT('Ctrl Pts',(0.774683802193014,-11.2007893104001,
-16.5679506381934));
#43325=CARTESIAN_POINT('Ctrl Pts',(0.782347306189922,-11.2003633889388,
-16.5682125378109));
#43326=CARTESIAN_POINT('Ctrl Pts',(0.789984975277527,-11.1999324779726,
-16.5684775342458));
#43327=CARTESIAN_POINT('Ctrl Pts',(0.797596805103168,-11.1994967017585,
-16.5687455519958));
#43328=CARTESIAN_POINT('Ctrl Pts',(0.805208634928809,-11.1990609255445,
-16.5690135697459));
#43329=CARTESIAN_POINT('Ctrl Pts',(0.814558096372233,-11.1985163947011,
-16.5693485181722));
#43330=CARTESIAN_POINT('Ctrl Pts',(0.820354772663952,-11.1981749011472,
-16.5695585939035));
#43331=CARTESIAN_POINT('Ctrl Pts',(0.913219558123246,-11.1927040547485,
-16.5729240807328));
#43332=CARTESIAN_POINT('Ctrl Pts',(1.01097505007198,-11.18602334519,-16.5770368529345));
#43333=CARTESIAN_POINT('Ctrl Pts',(1.11356403244014,-11.1778368406865,-16.5820825950803));
#43334=CARTESIAN_POINT('Ctrl Pts',(1.22619397592018,-11.1688490769107,-16.5876221924093));
#43335=CARTESIAN_POINT('Ctrl Pts',(1.3446506836048,-11.1580464090106,-16.5942863065747));
#43336=CARTESIAN_POINT('Ctrl Pts',(1.46882933599734,-11.1450092847503,-16.6023380665375));
#43337=CARTESIAN_POINT('Ctrl Pts',(1.51533012697266,-11.1401273136669,-16.6053531838688));
#43338=CARTESIAN_POINT('Ctrl Pts',(1.56263293993733,-11.1349316887056,-16.6085631034439));
#43339=CARTESIAN_POINT('Ctrl Pts',(1.61073097180307,-11.1293992405122,-16.6119824130128));
#43340=CARTESIAN_POINT('Ctrl Pts',(1.74016071397297,-11.114511659556,-16.621183628504));
#43341=CARTESIAN_POINT('Ctrl Pts',(1.87535186247608,-11.0971867682461,-16.6318998991873));
#43342=CARTESIAN_POINT('Ctrl Pts',(2.0161480133904,-11.076962068608,-16.6444228013579));
#43343=CARTESIAN_POINT('Ctrl Pts',(2.02946096582092,-11.0750497261011,-16.6456069019161));
#43344=CARTESIAN_POINT('Ctrl Pts',(2.04282399839302,-11.0731114398401,-16.6468071672487));
#43345=CARTESIAN_POINT('Ctrl Pts',(2.05623695836665,-11.0711468080309,-16.6480238514605));
#43346=CARTESIAN_POINT('Ctrl Pts',(2.18613474374757,-11.052120335007,-16.659806827398));
#43347=CARTESIAN_POINT('Ctrl Pts',(2.32071794504607,-11.0306238249927,-16.6731290660953));
#43348=CARTESIAN_POINT('Ctrl Pts',(2.45983349748882,-11.0062919740499,-16.6882214249664));
#43349=CARTESIAN_POINT('Ctrl Pts',(2.57754555014244,-10.9857036784276,-16.7009917623652));
#43350=CARTESIAN_POINT('Ctrl Pts',(2.69850206667232,-10.9630849751568,-16.7150297166465));
#43351=CARTESIAN_POINT('Ctrl Pts',(2.82259417732661,-10.9382138516592,-16.7304759714643));
#43352=CARTESIAN_POINT('Ctrl Pts',(2.92928969130115,-10.9168294357546,-16.7437568004233));
#43353=CARTESIAN_POINT('Ctrl Pts',(3.03830297427961,-10.8937797171167,-16.7580788499927));
#43354=CARTESIAN_POINT('Ctrl Pts',(3.14955604559843,-10.8689251872062,-16.7735308186299));
#43355=CARTESIAN_POINT('Ctrl Pts',(3.24644396472019,-10.8472799089659,-16.7869876074613));
#43356=CARTESIAN_POINT('Ctrl Pts',(3.34503044443255,-10.8242657538655,-16.8013013974624));
#43357=CARTESIAN_POINT('Ctrl Pts',(3.4452591362198,-10.7997924913389,-16.8165298503263));
#43358=CARTESIAN_POINT('Ctrl Pts',(3.44870611269044,-10.7989508285517,-16.8170535738007));
#43359=CARTESIAN_POINT('Ctrl Pts',(3.45215503088173,-10.7981074401231,-16.817578379043));
#43360=CARTESIAN_POINT('Ctrl Pts',(3.45560588843955,-10.7972623224504,-16.8181042683679));
#43361=CARTESIAN_POINT('Ctrl Pts',(3.53367151632138,-10.7781439900793,-16.830000986692));
#43362=CARTESIAN_POINT('Ctrl Pts',(3.61272981791193,-10.7581406445687,-16.842452520378));
#43363=CARTESIAN_POINT('Ctrl Pts',(3.6927523583703,-10.7372109243013,-16.8554855073975));
#43364=CARTESIAN_POINT('Ctrl Pts',(3.6994455828851,-10.7354603260826,-16.8565756091078));
#43365=CARTESIAN_POINT('Ctrl Pts',(3.70614555314959,-10.7337032472821,-16.8576697785203));
#43366=CARTESIAN_POINT('Ctrl Pts',(3.71285225154974,-10.7319396639566,-16.8587680310963));
#43367=CARTESIAN_POINT('Ctrl Pts',(3.74623736860275,-10.7231607637824,-16.8642349968991));
#43368=CARTESIAN_POINT('Ctrl Pts',(3.77978920910826,-10.7142206840802,-16.8698031415053));
#43369=CARTESIAN_POINT('Ctrl Pts',(3.8135056146136,-10.7051165161308,-16.8754743575615));
#43370=CARTESIAN_POINT('Ctrl Pts',(3.83375044264756,-10.6996499691556,-16.8788796076788));
#43371=CARTESIAN_POINT('Ctrl Pts',(3.85405460221175,-10.6941242623235,-16.882322018926));
#43372=CARTESIAN_POINT('Ctrl Pts',(3.87441762408892,-10.6885387708392,-16.8858019987448));
#43373=CARTESIAN_POINT('Ctrl Pts',(3.8845991350275,-10.685746025097,-16.8875419886541));
#43374=CARTESIAN_POINT('Ctrl Pts',(3.89479536154432,-10.6829383331958,-16.889291370713));
#43375=CARTESIAN_POINT('Ctrl Pts',(3.9050062438488,-10.6801156172595,-16.8910501957667));
#43376=CARTESIAN_POINT('Ctrl Pts',(3.91011168500104,-10.6787042592913,-16.8919296082936));
#43377=CARTESIAN_POINT('Ctrl Pts',(3.9152207901002,-10.6772891453145,-16.8928113815695));
#43378=CARTESIAN_POINT('Ctrl Pts',(3.92033355162271,-10.6758702656219,-16.8936955219368));
#43379=CARTESIAN_POINT('Ctrl Pts',(3.92544631314522,-10.6744513859293,-16.8945796623041));
#43380=CARTESIAN_POINT('Ctrl Pts',(3.93232800673322,-10.6725369449989,-16.8957726344704));
#43381=CARTESIAN_POINT('Ctrl Pts',(3.93568279791968,-10.6716023196972,-16.896355050652));
#43382=CARTESIAN_POINT('Ctrl Pts',(3.94201776597147,-10.6698374344637,-16.8974548472408));
#43383=CARTESIAN_POINT('Ctrl Pts',(3.94833529222159,-10.6680732144636,-16.8985542612453));
#43384=CARTESIAN_POINT('Ctrl Pts',(3.95463539437183,-10.6663097239537,-16.8996532525245));
#43385=CARTESIAN_POINT('Ctrl Pts',(4.029847930132,-10.6452566378487,-16.9127733446943));
#43386=CARTESIAN_POINT('Ctrl Pts',(4.10257711988876,-10.6243083475567,-16.9258326928244));
#43387=CARTESIAN_POINT('Ctrl Pts',(4.17285368553367,-10.6035689783872,-16.938766316102));
#43388=CARTESIAN_POINT('Ctrl Pts',(4.24078041999403,-10.5835230696334,-16.951267478985));
#43389=CARTESIAN_POINT('Ctrl Pts',(4.30641583381684,-10.5636722621969,-16.9636512381799));
#43390=CARTESIAN_POINT('Ctrl Pts',(4.36978780547811,-10.5441021612752,-16.9758641581216));
#43391=CARTESIAN_POINT('Ctrl Pts',(4.43123718186365,-10.5251257831396,-16.9877065593377));
#43392=CARTESIAN_POINT('Ctrl Pts',(4.49055838833727,-10.5064132731806,-16.9993883734015));
#43393=CARTESIAN_POINT('Ctrl Pts',(4.54777651243732,-10.4880356345445,-17.0108652653892));
#43394=CARTESIAN_POINT('Ctrl Pts',(4.60352991910268,-10.470128442085,-17.0220483622892));
#43395=CARTESIAN_POINT('Ctrl Pts',(4.65728654873519,-10.4525391465315,-17.0330369286175));
#43396=CARTESIAN_POINT('Ctrl Pts',(4.70906899456592,-10.4353274409371,-17.0437936677973));
#43397=CARTESIAN_POINT('Ctrl Pts',(4.75988646526016,-10.4184364785539,-17.0543499532192));
#43398=CARTESIAN_POINT('Ctrl Pts',(4.80880265148368,-10.4019091283525,-17.0646829976357));
#43399=CARTESIAN_POINT('Ctrl Pts',(4.85583810557444,-10.3857965650477,-17.0747607860637));
#43400=CARTESIAN_POINT('Ctrl Pts',(4.90206735032973,-10.3699601784952,-17.0846658365588));
#43401=CARTESIAN_POINT('Ctrl Pts',(4.946479786719,-10.3545244514947,-17.0943243290815));
#43402=CARTESIAN_POINT('Ctrl Pts',(4.98909401540873,-10.3395333433219,-17.103708699377));
#43403=CARTESIAN_POINT('Ctrl Pts',(4.98946319241318,-10.3394034718546,-17.1037899983661));
#43404=CARTESIAN_POINT('Ctrl Pts',(4.98983223445392,-10.3392736337286,-17.1038712767975));
#43405=CARTESIAN_POINT('Ctrl Pts',(4.99020114154273,-10.3391438289709,-17.1039525346539));
#43406=CARTESIAN_POINT('Ctrl Pts',(5.03326624116998,-10.3239908135093,-17.1134383314568));
#43407=CARTESIAN_POINT('Ctrl Pts',(5.07449235854055,-10.3092929024427,-17.1226435416269));
#43408=CARTESIAN_POINT('Ctrl Pts',(5.1138976567057,-10.2950910016694,-17.1315424101203));
#43409=CARTESIAN_POINT('Ctrl Pts',(5.15370169377103,-10.2807453930557,-17.140531325516));
#43410=CARTESIAN_POINT('Ctrl Pts',(5.19164787993578,-10.2669058765484,-17.149207678055));
#43411=CARTESIAN_POINT('Ctrl Pts',(5.22775373278064,-10.2536101379609,-17.1575475826569));
#43412=CARTESIAN_POINT('Ctrl Pts',(5.26453890978093,-10.240064242801,-17.1660444008394));
#43413=CARTESIAN_POINT('Ctrl Pts',(5.29941385717798,-10.2270827796985,-17.1741919971205));
#43414=CARTESIAN_POINT('Ctrl Pts',(5.33239574608239,-10.2147010350817,-17.1819677752936));
#43415=CARTESIAN_POINT('Ctrl Pts',(5.36640991178116,-10.2019317630047,-17.1899869220437));
#43416=CARTESIAN_POINT('Ctrl Pts',(5.39841067752601,-10.1898003462685,-17.19761061042));
#43417=CARTESIAN_POINT('Ctrl Pts',(5.42841530805322,-10.178340594185,-17.2048168552523));
#43418=CARTESIAN_POINT('Ctrl Pts',(5.45996274036015,-10.1662915955219,-17.2123936364703));
#43419=CARTESIAN_POINT('Ctrl Pts',(5.48930350857564,-10.1549851364485,-17.2195089260922));
#43420=CARTESIAN_POINT('Ctrl Pts',(5.51645571937467,-10.1444548599959,-17.2261403666752));
#43421=CARTESIAN_POINT('Ctrl Pts',(5.54440396502199,-10.1336158621991,-17.232966224495));
#43422=CARTESIAN_POINT('Ctrl Pts',(5.57003347968119,-10.1235992310435,-17.2392794342393));
#43423=CARTESIAN_POINT('Ctrl Pts',(5.5933616600179,-10.1144355422305,-17.2450591005858));
#43424=CARTESIAN_POINT('Ctrl Pts',(-5.84637332548169,-10.2457285222001,
-16.9490859041272));
#43425=CARTESIAN_POINT('Ctrl Pts',(-5.81071186277041,-10.2597918225017,
-16.9400659709806));
#43426=CARTESIAN_POINT('Ctrl Pts',(-5.69191724338071,-10.3062068549176,
-16.9103314356046));
#43427=CARTESIAN_POINT('Ctrl Pts',(-5.48049048445379,-10.3862539649999,
-16.8592260848499));
#43428=CARTESIAN_POINT('Ctrl Pts',(-5.20214452272255,-10.4866571133216,
-16.7953170882305));
#43429=CARTESIAN_POINT('Ctrl Pts',(-4.89413796043385,-10.5916763009553,
-16.7286060724361));
#43430=CARTESIAN_POINT('Ctrl Pts',(-4.55276036895968,-10.7006317075456,
-16.6594985240082));
#43431=CARTESIAN_POINT('Ctrl Pts',(-4.17237911330225,-10.8128338020862,
-16.5884198593204));
#43432=CARTESIAN_POINT('Ctrl Pts',(-3.74657608403547,-10.9269277982907,
-16.5162278749803));
#43433=CARTESIAN_POINT('Ctrl Pts',(-3.27004596366195,-11.0401715973013,
-16.4446665253294));
#43434=CARTESIAN_POINT('Ctrl Pts',(-2.73872015992667,-11.1484285626666,
-16.3763657772148));
#43435=CARTESIAN_POINT('Ctrl Pts',(-2.14782149455781,-11.2465594493992,
-16.314586419439));
#43436=CARTESIAN_POINT('Ctrl Pts',(-1.49674277405162,-11.3274272171767,
-16.263833005406));
#43437=CARTESIAN_POINT('Ctrl Pts',(-0.805541188003819,-11.3814775262563,
-16.2300679937111));
#43438=CARTESIAN_POINT('Ctrl Pts',(-0.113422498730109,-11.4024991021397,
-16.2170495617272));
#43439=CARTESIAN_POINT('Ctrl Pts',(0.536119675481227,-11.3923378993577,
-16.2233276646495));
#43440=CARTESIAN_POINT('Ctrl Pts',(1.11982241638366,-11.3587982050083,-16.2442236936773));
#43441=CARTESIAN_POINT('Ctrl Pts',(1.63691910407471,-11.3100218589162,-16.2747549957963));
#43442=CARTESIAN_POINT('Ctrl Pts',(2.09764987884417,-11.2515354414113,-16.3114736122001));
#43443=CARTESIAN_POINT('Ctrl Pts',(2.51229038323631,-11.1867215225181,-16.3522535319986));
#43444=CARTESIAN_POINT('Ctrl Pts',(2.88628054447622,-11.1183510319995,-16.3953417834328));
#43445=CARTESIAN_POINT('Ctrl Pts',(3.2233003370683,-11.0487029073154,-16.4392911535778));
#43446=CARTESIAN_POINT('Ctrl Pts',(3.52771849233986,-10.9792399963371,-16.483168618013));
#43447=CARTESIAN_POINT('Ctrl Pts',(3.80296220772403,-10.9110754271386,-16.5262629591106));
#43448=CARTESIAN_POINT('Ctrl Pts',(4.05167352300846,-10.8451033354659,-16.5680024561924));
#43449=CARTESIAN_POINT('Ctrl Pts',(4.27619687662968,-10.7819779872887,-16.6079681104034));
#43450=CARTESIAN_POINT('Ctrl Pts',(4.47888810571171,-10.7220827433237,-16.6459133079799));
#43451=CARTESIAN_POINT('Ctrl Pts',(4.66210367536694,-10.6655684627837,-16.6817395203754));
#43452=CARTESIAN_POINT('Ctrl Pts',(4.82816201161895,-10.6123989400204,-16.7154675137374));
#43453=CARTESIAN_POINT('Ctrl Pts',(4.97930409772923,-10.5623954933759,-16.7472090922686));
#43454=CARTESIAN_POINT('Ctrl Pts',(5.11759466981168,-10.5152990600229,-16.777127743207));
#43455=CARTESIAN_POINT('Ctrl Pts',(5.2446356860934,-10.4708992468505,-16.8053566586536));
#43456=CARTESIAN_POINT('Ctrl Pts',(5.361519589857,-10.4290877510992,-16.8319645189151));
#43457=CARTESIAN_POINT('Ctrl Pts',(5.46894761068017,-10.389845269209,-16.8569634140839));
#43458=CARTESIAN_POINT('Ctrl Pts',(5.56755786494024,-10.353137310211,-16.8803748902788));
#43459=CARTESIAN_POINT('Ctrl Pts',(5.65799402488361,-10.3188938968047,-16.9022427847047));
#43460=CARTESIAN_POINT('Ctrl Pts',(5.74090216942931,-10.2870141534843,-16.922630231597));
#43461=CARTESIAN_POINT('Ctrl Pts',(5.80283684814847,-10.262865189594,-16.9380975469863));
#43462=CARTESIAN_POINT('Ctrl Pts',(5.83721009878716,-10.2493419733393,-16.9467690913668));
#43463=CARTESIAN_POINT('Ctrl Pts',(5.84634760391269,-10.2457385356534,-16.94908046904));
#43464=CARTESIAN_POINT('Ctrl Pts',(-5.81214087226646,-10.2495588877839,
-17.0923483286303));
#43465=CARTESIAN_POINT('Ctrl Pts',(-5.77669421366777,-10.263585043884,-17.0833806892945));
#43466=CARTESIAN_POINT('Ctrl Pts',(-5.65860674633896,-10.3098810943373,
-17.0538165479733));
#43467=CARTESIAN_POINT('Ctrl Pts',(-5.44839807609833,-10.3897402705518,
-17.002994561743));
#43468=CARTESIAN_POINT('Ctrl Pts',(-5.17161875998938,-10.4899251179542,
-16.9394319559991));
#43469=CARTESIAN_POINT('Ctrl Pts',(-4.86533505594304,-10.5947248316,-16.8730806258442));
#43470=CARTESIAN_POINT('Ctrl Pts',(-4.52587295636493,-10.7034566982716,
-16.8043472696556));
#43471=CARTESIAN_POINT('Ctrl Pts',(-4.14764429910443,-10.815429902991,-16.7336572517321));
#43472=CARTESIAN_POINT('Ctrl Pts',(-3.72427883476413,-10.9292907205645,
-16.6618651175188));
#43473=CARTESIAN_POINT('Ctrl Pts',(-3.2505124902038,-11.0423015126171,-16.5907059004491));
#43474=CARTESIAN_POINT('Ctrl Pts',(-2.72230931494296,-11.1503335008612,
-16.522794637113));
#43475=CARTESIAN_POINT('Ctrl Pts',(-2.13492568104469,-11.2482580101081,
-16.4613723404917));
#43476=CARTESIAN_POINT('Ctrl Pts',(-1.48775542557803,-11.3289535679597,
-16.4109153319803));
#43477=CARTESIAN_POINT('Ctrl Pts',(-0.800722870402349,-11.3828875444853,
-16.3773484312674));
#43478=CARTESIAN_POINT('Ctrl Pts',(-0.112751530280082,-11.4038638339061,
-16.3644057238811));
#43479=CARTESIAN_POINT('Ctrl Pts',(0.532923322872193,-11.393724488833,-16.3706474396948));
#43480=CARTESIAN_POINT('Ctrl Pts',(1.11310674869981,-11.3602570986451,-16.3914210675063));
#43481=CARTESIAN_POINT('Ctrl Pts',(1.62709029934784,-11.3115853094998,-16.421773479825));
#43482=CARTESIAN_POINT('Ctrl Pts',(2.08505695572989,-11.2532232613542,-16.4582779258125));
#43483=CARTESIAN_POINT('Ctrl Pts',(2.49722536832563,-11.1885459997271,-16.4988216357698));
#43484=CARTESIAN_POINT('Ctrl Pts',(2.8690023751527,-11.1203184890061,-16.5416623854398));
#43485=CARTESIAN_POINT('Ctrl Pts',(3.20404389664109,-11.0508149453896,-16.5853615650137));
#43486=CARTESIAN_POINT('Ctrl Pts',(3.50668982747596,-10.9814953247755,-16.6289915145168));
#43487=CARTESIAN_POINT('Ctrl Pts',(3.78034401638953,-10.9134706619404,-16.6718449093925));
#43488=CARTESIAN_POINT('Ctrl Pts',(4.02762985992248,-10.8476334958496,-16.7133529789763));
#43489=CARTESIAN_POINT('Ctrl Pts',(4.25087514568035,-10.7846370103216,-16.7530987152803));
#43490=CARTESIAN_POINT('Ctrl Pts',(4.4524193755322,-10.7248640421826,-16.7908364851191));
#43491=CARTESIAN_POINT('Ctrl Pts',(4.63460310804401,-10.6684653950088,-16.8264679115715));
#43492=CARTESIAN_POINT('Ctrl Pts',(4.7997295023731,-10.615405180405,-16.8600132720348));
#43493=CARTESIAN_POINT('Ctrl Pts',(4.95002508579651,-10.5655053209492,-16.8915834110162));
#43494=CARTESIAN_POINT('Ctrl Pts',(5.08754142422316,-10.5185075294211,-16.9213406010467));
#43495=CARTESIAN_POINT('Ctrl Pts',(5.21387010174365,-10.4742021033152,-16.949416999978));
#43496=CARTESIAN_POINT('Ctrl Pts',(5.33009618342973,-10.4324812281455,-16.9758806130043));
#43497=CARTESIAN_POINT('Ctrl Pts',(5.43691587090918,-10.3933258857094,-17.000743180377));
#43498=CARTESIAN_POINT('Ctrl Pts',(5.53496282001455,-10.3567018589229,-17.0240258852323));
#43499=CARTESIAN_POINT('Ctrl Pts',(5.62487650588722,-10.3225394406628,-17.0457721441461));
#43500=CARTESIAN_POINT('Ctrl Pts',(5.70729921987737,-10.2907379563893,-17.0660446662553));
#43501=CARTESIAN_POINT('Ctrl Pts',(5.76886605571337,-10.2666505418325,-17.0814235370967));
#43502=CARTESIAN_POINT('Ctrl Pts',(5.80303331070594,-10.2531625980629,-17.0900450461037));
#43503=CARTESIAN_POINT('Ctrl Pts',(5.81211594917672,-10.2495686064607,-17.0923430612159));
#43504=CARTESIAN_POINT('Ctrl Pts',(-5.75637734409201,-10.1837214316228,
-17.211851398876));
#43505=CARTESIAN_POINT('Ctrl Pts',(-5.72124284752165,-10.1976641910222,
-17.2029834527919));
#43506=CARTESIAN_POINT('Ctrl Pts',(-5.60419033019956,-10.2436872748253,
-17.1737470798349));
#43507=CARTESIAN_POINT('Ctrl Pts',(-5.39580264084002,-10.3230857151126,
-17.1234851683103));
#43508=CARTESIAN_POINT('Ctrl Pts',(-5.12141647158099,-10.42269850384,-17.0606253549015));
#43509=CARTESIAN_POINT('Ctrl Pts',(-4.81780583424873,-10.5268967653542,
-16.9950167689353));
#43510=CARTESIAN_POINT('Ctrl Pts',(-4.48135309698756,-10.6349959889591,
-16.9270663881488));
#43511=CARTESIAN_POINT('Ctrl Pts',(-4.10654376052558,-10.7463050991349,
-16.8571984811656));
#43512=CARTESIAN_POINT('Ctrl Pts',(-3.68709091827589,-10.8594751597388,
-16.7862604612738));
#43513=CARTESIAN_POINT('Ctrl Pts',(-3.21780670798508,-10.971783037663,-16.7159682018366));
#43514=CARTESIAN_POINT('Ctrl Pts',(-2.69471979108215,-11.0791253962985,
-16.6489041174503));
#43515=CARTESIAN_POINT('Ctrl Pts',(-2.11315352363968,-11.1764086181218,
-16.5882650970455));
#43516=CARTESIAN_POINT('Ctrl Pts',(-1.47251555563333,-11.2565631728444,
-16.5384635825327));
#43517=CARTESIAN_POINT('Ctrl Pts',(-0.792512707503636,-11.3101287606434,
-16.5053381510962));
#43518=CARTESIAN_POINT('Ctrl Pts',(-0.111600877647295,-11.3309605049197,
-16.4925657128992));
#43519=CARTESIAN_POINT('Ctrl Pts',(0.527465568466855,-11.3208910656544,
-16.498725432769));
#43520=CARTESIAN_POINT('Ctrl Pts',(1.10169493934813,-11.2876532359364,-16.5192254848422));
#43521=CARTESIAN_POINT('Ctrl Pts',(1.61044354821197,-11.2393115573349,-16.549180465967));
#43522=CARTESIAN_POINT('Ctrl Pts',(2.06379404302651,-11.1813397325491,-16.5852117077644));
#43523=CARTESIAN_POINT('Ctrl Pts',(2.471861519669,-11.1170880815756,-16.6252363961343));
#43524=CARTESIAN_POINT('Ctrl Pts',(2.83999173167234,-11.0493021153008,-16.6675363377561));
#43525=CARTESIAN_POINT('Ctrl Pts',(3.17179488221991,-10.9802409395444,-16.7106918698678));
#43526=CARTESIAN_POINT('Ctrl Pts',(3.47155832012703,-10.9113554185891,-16.7537869552704));
#43527=CARTESIAN_POINT('Ctrl Pts',(3.74264328254365,-10.8437502095096,-16.796122535093));
#43528=CARTESIAN_POINT('Ctrl Pts',(3.98763901526073,-10.7783131840131,-16.8371359548506));
#43529=CARTESIAN_POINT('Ctrl Pts',(4.20884309009698,-10.7156945421076,-16.8764141939803));
#43530=CARTESIAN_POINT('Ctrl Pts',(4.40856598476383,-10.6562758598002,-16.9137134248617));
#43531=CARTESIAN_POINT('Ctrl Pts',(4.58912056820789,-10.6002080549719,-16.9489353282972));
#43532=CARTESIAN_POINT('Ctrl Pts',(4.75278392451138,-10.5474563849102,-16.9820989261338));
#43533=CARTESIAN_POINT('Ctrl Pts',(4.90175832806563,-10.4978446501649,-17.0133128760172));
#43534=CARTESIAN_POINT('Ctrl Pts',(5.03807359652703,-10.4511168044891,-17.0427368019685));
#43535=CARTESIAN_POINT('Ctrl Pts',(5.16330433230364,-10.4070650240004,-17.0705006587464));
#43536=CARTESIAN_POINT('Ctrl Pts',(5.27852354531286,-10.3655827319811,-17.0966710388853));
#43537=CARTESIAN_POINT('Ctrl Pts',(5.38441915340594,-10.3266515868676,-17.1212589517494));
#43538=CARTESIAN_POINT('Ctrl Pts',(5.48161746197151,-10.2902380611074,-17.1442848117902));
#43539=CARTESIAN_POINT('Ctrl Pts',(5.57075099042334,-10.2562732309174,-17.165791113276));
#43540=CARTESIAN_POINT('Ctrl Pts',(5.65245559249821,-10.2246572217323,-17.1858395574668));
#43541=CARTESIAN_POINT('Ctrl Pts',(5.71348329886499,-10.2007116154242,-17.2010479984918));
#43542=CARTESIAN_POINT('Ctrl Pts',(5.74735040680101,-10.1873035413794,-17.2095738079189));
#43543=CARTESIAN_POINT('Ctrl Pts',(5.75635321170445,-10.183730856004,-17.2118463092144));
#43544=CARTESIAN_POINT('Ctrl Pts',(-5.69417817154424,-10.0659581588309,
-17.2751179674529));
#43545=CARTESIAN_POINT('Ctrl Pts',(-5.65936864914472,-10.0797938193227,
-17.2663701428645));
#43546=CARTESIAN_POINT('Ctrl Pts',(-5.54339858367167,-10.1254637566733,
-17.2375302403083));
#43547=CARTESIAN_POINT('Ctrl Pts',(-5.33694163763027,-10.2042532095778,
-17.1879536089715));
#43548=CARTESIAN_POINT('Ctrl Pts',(-5.06512710375388,-10.3030947989692,
-17.1259628950955));
#43549=CARTESIAN_POINT('Ctrl Pts',(-4.76441598180649,-10.4064721735374,
-17.0612792228816));
#43550=CARTESIAN_POINT('Ctrl Pts',(-4.43125170592017,-10.5137006103613,
-16.9943088394544));
#43551=CARTESIAN_POINT('Ctrl Pts',(-4.0602026902282,-10.6240898693539,-16.9254741696221));
#43552=CARTESIAN_POINT('Ctrl Pts',(-3.64507829848461,-10.7362982384052,
-16.855613542186));
#43553=CARTESIAN_POINT('Ctrl Pts',(-3.18078122530719,-10.8476232159053,
-16.7864186128264));
#43554=CARTESIAN_POINT('Ctrl Pts',(-2.66341923621865,-10.9539976173594,
-16.7204303040473));
#43555=CARTESIAN_POINT('Ctrl Pts',(-2.08839798587963,-11.0503779004316,
-16.6607889637688));
#43556=CARTESIAN_POINT('Ctrl Pts',(-1.45514799384261,-11.1297688198829,
-16.6118247794394));
#43557=CARTESIAN_POINT('Ctrl Pts',(-0.783132822844211,-11.1828134874774,
-16.5792648005158));
#43558=CARTESIAN_POINT('Ctrl Pts',(-0.110281963132231,-11.2034404779047,
-16.5667111358745));
#43559=CARTESIAN_POINT('Ctrl Pts',(0.521223569944504,-11.1934701070349,
-16.5727654222531));
#43560=CARTESIAN_POINT('Ctrl Pts',(1.088675687679,-11.1605570758883,-16.5929146993741));
#43561=CARTESIAN_POINT('Ctrl Pts',(1.59148448878036,-11.112681877478,-16.6223611758767));
#43562=CARTESIAN_POINT('Ctrl Pts',(2.03961626720081,-11.0552607044016,-16.6577881393295));
#43563=CARTESIAN_POINT('Ctrl Pts',(2.4430640223962,-10.9916086294779,-16.6971513458778));
#43564=CARTESIAN_POINT('Ctrl Pts',(2.80710095595344,-10.9244434772457,-16.7387634185779));
#43565=CARTESIAN_POINT('Ctrl Pts',(3.13528225919823,-10.8560029362005,-16.7812288621149));
#43566=CARTESIAN_POINT('Ctrl Pts',(3.4318332440259,-10.7877250356114,-16.8236463772724));
#43567=CARTESIAN_POINT('Ctrl Pts',(3.70006480314895,-10.7207054935996,-16.8653273080683));
#43568=CARTESIAN_POINT('Ctrl Pts',(3.94252576464268,-10.6558257052943,-16.9057166281625));
#43569=CARTESIAN_POINT('Ctrl Pts',(4.16147809567636,-10.5937317915771,-16.9444062223776));
#43570=CARTESIAN_POINT('Ctrl Pts',(4.3591984151706,-10.5348036715704,-16.9811544051073));
#43571=CARTESIAN_POINT('Ctrl Pts',(4.53796761309588,-10.4791925166925,-17.0158628051438));
#43572=CARTESIAN_POINT('Ctrl Pts',(4.7000329475385,-10.4268652489092,-17.0485487613563));
#43573=CARTESIAN_POINT('Ctrl Pts',(4.84756920767978,-10.377648313081,-17.0793181086446));
#43574=CARTESIAN_POINT('Ctrl Pts',(4.98258177189424,-10.3312887637657,-17.1083271049463));
#43575=CARTESIAN_POINT('Ctrl Pts',(5.10662625028276,-10.2875813360151,-17.1357029288908));
#43576=CARTESIAN_POINT('Ctrl Pts',(5.22076218401111,-10.2464211057805,-17.1615104048565));
#43577=CARTESIAN_POINT('Ctrl Pts',(5.32566819367259,-10.2077906165106,-17.1857596279649));
#43578=CARTESIAN_POINT('Ctrl Pts',(5.42196233402055,-10.1716572594301,-17.2084700461599));
#43579=CARTESIAN_POINT('Ctrl Pts',(5.51026929292823,-10.137953195577,-17.2296829791277));
#43580=CARTESIAN_POINT('Ctrl Pts',(5.59121757886941,-10.1065797333569,-17.2494588099646));
#43581=CARTESIAN_POINT('Ctrl Pts',(5.65168088096111,-10.0828178525011,-17.2644609425763));
#43582=CARTESIAN_POINT('Ctrl Pts',(5.68523498109198,-10.0695126493564,-17.2728712786581));
#43583=CARTESIAN_POINT('Ctrl Pts',(5.69415460746513,-10.065967369274,-17.2751130174018));
#43584=CARTESIAN_POINT('',(5.73644274981206,-10.2877306125196,-16.9337807222045));
#43585=CARTESIAN_POINT('Origin',(5.599999999773,-9.91330329131332,-16.8993688489362));
#43586=CARTESIAN_POINT('Ctrl Pts',(-5.73644387793508,-10.2877346863084,
-16.9337810350649));
#43587=CARTESIAN_POINT('Ctrl Pts',(-5.66411038088194,-10.3157397295418,
-16.9158630928389));
#43588=CARTESIAN_POINT('Ctrl Pts',(-5.58548128629471,-10.3456524214079,
-16.8967577754712));
#43589=CARTESIAN_POINT('Ctrl Pts',(-5.50055659255391,-10.3771725884232,
-16.8766547496469));
#43590=CARTESIAN_POINT('Ctrl Pts',(-5.41741953929581,-10.4080292649496,
-16.8569748867591));
#43591=CARTESIAN_POINT('Ctrl Pts',(-5.32824913848286,-10.4404262972982,
-16.8363389758404));
#43592=CARTESIAN_POINT('Ctrl Pts',(-5.23304538859569,-10.4740375140448,
-16.8149530263938));
#43593=CARTESIAN_POINT('Ctrl Pts',(-5.13477098481712,-10.5087328100804,
-16.7928773052841));
#43594=CARTESIAN_POINT('Ctrl Pts',(-5.03006776232682,-10.5447221363093,
-16.7700022193492));
#43595=CARTESIAN_POINT('Ctrl Pts',(-4.91893571945363,-10.5815974269667,
-16.7465854206368));
#43596=CARTESIAN_POINT('Ctrl Pts',(-4.80780367658045,-10.618472717624,-16.7231686219243));
#43597=CARTESIAN_POINT('Ctrl Pts',(-4.69024281332438,-10.6562339759072,
-16.6992101083396));
#43598=CARTESIAN_POINT('Ctrl Pts',(-4.56625312801428,-10.6944230049809,
-16.6749991117564));
#43599=CARTESIAN_POINT('Ctrl Pts',(-4.44622756306065,-10.7313910783988,
-16.651562173952));
#43600=CARTESIAN_POINT('Ctrl Pts',(-4.32017768330217,-10.7687597630938,
-16.6278887933617));
#43601=CARTESIAN_POINT('Ctrl Pts',(-4.18810348873885,-10.8060686256879,
-16.6042695578197));
#43602=CARTESIAN_POINT('Ctrl Pts',(-4.0516176077232,-10.8446237196462,-16.5798613667834));
#43603=CARTESIAN_POINT('Ctrl Pts',(-3.90869822869223,-10.8831151989686,
-16.555510827552));
#43604=CARTESIAN_POINT('Ctrl Pts',(-3.75934535164596,-10.9209854312692,
-16.5315698199977));
#43605=CARTESIAN_POINT('Ctrl Pts',(-3.60999247459969,-10.9588556635699,
-16.5076288124434));
#43606=CARTESIAN_POINT('Ctrl Pts',(-3.4542060995381,-10.9961046535704,-16.4840973331131));
#43607=CARTESIAN_POINT('Ctrl Pts',(-3.29198622646121,-11.0321243882891,
-16.4613590111071));
#43608=CARTESIAN_POINT('Ctrl Pts',(-3.21175020597794,-11.0499402089889,
-16.4501123467151));
#43609=CARTESIAN_POINT('Ctrl Pts',(-3.12994028314089,-11.0674545261354,
-16.4390602110145));
#43610=CARTESIAN_POINT('Ctrl Pts',(-3.04655646263601,-11.084589205439,-16.4282519173722));
#43611=CARTESIAN_POINT('Ctrl Pts',(-3.00486455238357,-11.0931565450908,
-16.4228477705511));
#43612=CARTESIAN_POINT('Ctrl Pts',(-2.96277915898731,-11.1016289310983,
-16.4175045824374));
#43613=CARTESIAN_POINT('Ctrl Pts',(-2.9203002937044,-11.1099963096612,-16.4122287337783));
#43614=CARTESIAN_POINT('Ctrl Pts',(-2.89906086106294,-11.1141799989426,
-16.4095908094488));
#43615=CARTESIAN_POINT('Ctrl Pts',(-2.87772305988289,-11.1183374336123,
-16.4069697198654));
#43616=CARTESIAN_POINT('Ctrl Pts',(-2.85628689001648,-11.122467339776,-16.4043662682671));
#43617=CARTESIAN_POINT('Ctrl Pts',(-2.84556880508328,-11.1245322928579,
-16.403064542468));
#43618=CARTESIAN_POINT('Ctrl Pts',(-2.83482612794603,-11.1265903636395,
-16.4017672261584));
#43619=CARTESIAN_POINT('Ctrl Pts',(-2.82405885859587,-11.1286413917732,
-16.4004744204714));
#43620=CARTESIAN_POINT('Ctrl Pts',(-2.81867522392079,-11.12966690584,-16.3998280176279));
#43621=CARTESIAN_POINT('Ctrl Pts',(-2.81328544119046,-11.1306906592339,
-16.3991827424396));
#43622=CARTESIAN_POINT('Ctrl Pts',(-2.80788951040494,-11.1317126318419,
-16.3985386075961));
#43623=CARTESIAN_POINT('Ctrl Pts',(-2.80249357961942,-11.1327346044499,
-16.3978944727525));
#43624=CARTESIAN_POINT('Ctrl Pts',(-2.79531854980475,-11.1340886500716,
-16.3970410666963));
#43625=CARTESIAN_POINT('Ctrl Pts',(-2.79168327387877,-11.1347731871501,
-16.3966096368024));
#43626=CARTESIAN_POINT('Ctrl Pts',(-2.0459690089911,-11.2751941826081,-16.3081092223224));
#43627=CARTESIAN_POINT('Ctrl Pts',(-1.30026708119672,-11.3593704604482,
-16.255262289602));
#43628=CARTESIAN_POINT('Ctrl Pts',(-0.55454783475753,-11.3872667590075,
-16.2380733656739));
#43629=CARTESIAN_POINT('Ctrl Pts',(-0.369699771189191,-11.3941816626982,
-16.2338125941864));
#43630=CARTESIAN_POINT('Ctrl Pts',(-0.184850643494956,-11.3976383226358,
-16.2317429663731));
#43631=CARTESIAN_POINT('Ctrl Pts',(1.57296398128892E-12,-11.39763584854,
-16.2318648968627));
#43632=CARTESIAN_POINT('Ctrl Pts',(6.95448539688949E-5,-11.3976358476092,
-16.2318649427356));
#43633=CARTESIAN_POINT('Ctrl Pts',(0.000139089706577813,-11.3976358461888,
-16.2318649889188));
#43634=CARTESIAN_POINT('Ctrl Pts',(0.00020863455940168,-11.3976358442788,
-16.2318650354121));
#43635=CARTESIAN_POINT('Ctrl Pts',(0.4655335588341,-11.397623064167,-16.2321761224093));
#43636=CARTESIAN_POINT('Ctrl Pts',(0.930858482086974,-11.3756953217017,
-16.2460734435159));
#43637=CARTESIAN_POINT('Ctrl Pts',(1.39618340431804,-11.3318636296086,-16.2735530557509));
#43638=CARTESIAN_POINT('Ctrl Pts',(1.62884586543357,-11.3099477835621,-16.2872928618684));
#43639=CARTESIAN_POINT('Ctrl Pts',(1.86150832640041,-11.2825561673347,-16.3044279609873));
#43640=CARTESIAN_POINT('Ctrl Pts',(2.09417078585648,-11.2496914820838,-16.3249561696155));
#43641=CARTESIAN_POINT('Ctrl Pts',(2.21050201558451,-11.2332591394584,-16.3352202739296));
#43642=CARTESIAN_POINT('Ctrl Pts',(2.32683324685152,-11.2154585426896,-16.3463326560338));
#43643=CARTESIAN_POINT('Ctrl Pts',(2.44316447733801,-11.1962901146661,-16.3582929162943));
#43644=CARTESIAN_POINT('Ctrl Pts',(2.50133009258126,-11.1867059006543,-16.3642730464246));
#43645=CARTESIAN_POINT('Ctrl Pts',(2.55949570773231,-11.1767797296686,-16.3704651461174));
#43646=CARTESIAN_POINT('Ctrl Pts',(2.61766132280913,-11.1665116597524,-16.3768691619699));
#43647=CARTESIAN_POINT('Ctrl Pts',(2.64674413034754,-11.1613776247943,-16.3800711698961));
#43648=CARTESIAN_POINT('Ctrl Pts',(2.67582693787642,-11.156158115155,-16.3833261568642));
#43649=CARTESIAN_POINT('Ctrl Pts',(2.70490974539752,-11.1508531384236,-16.3866341157703));
#43650=CARTESIAN_POINT('Ctrl Pts',(2.73217487744855,-11.1458797227379,-16.3897353272447));
#43651=CARTESIAN_POINT('Ctrl Pts',(2.75944000949303,-11.1408311894926,-16.3928830960866));
#43652=CARTESIAN_POINT('Ctrl Pts',(2.78670514153725,-11.1357075451166,-16.3960774162571));
#43653=CARTESIAN_POINT('Ctrl Pts',(2.78852281700686,-11.1353659688249,-16.3962903709351));
#43654=CARTESIAN_POINT('Ctrl Pts',(2.7917228120462,-11.1347637864464,-16.3966657965686));
#43655=CARTESIAN_POINT('Ctrl Pts',(2.79215816794584,-11.1346818147619,-16.3967169009717));
#43656=CARTESIAN_POINT('Ctrl Pts',(2.80635173931964,-11.1320093553875,-16.3983830182642));
#43657=CARTESIAN_POINT('Ctrl Pts',(2.82657061154179,-11.128185218442,-16.4007801386854));
#43658=CARTESIAN_POINT('Ctrl Pts',(2.85281478461229,-11.1231354779899,-16.403954948736));
#43659=CARTESIAN_POINT('Ctrl Pts',(2.87905925167368,-11.11808568097,-16.4071297943512));
#43660=CARTESIAN_POINT('Ctrl Pts',(2.91132915457671,-11.1118102528191,-16.4110823469024));
#43661=CARTESIAN_POINT('Ctrl Pts',(2.94962449332137,-11.1041911936577,-16.4158871377949));
#43662=CARTESIAN_POINT('Ctrl Pts',(2.98792028538756,-11.0965720443055,-16.4206919855641));
#43663=CARTESIAN_POINT('Ctrl Pts',(3.03224165594858,-11.0876092319031,-16.4263490916455));
#43664=CARTESIAN_POINT('Ctrl Pts',(3.08258860500442,-11.0771406830763,-16.4329608363572));
#43665=CARTESIAN_POINT('Ctrl Pts',(3.13293654055834,-11.0666719291288,-16.4395727106193));
#43666=CARTESIAN_POINT('Ctrl Pts',(3.18931029073976,-11.0546973795104,-16.4471392605945));
#43667=CARTESIAN_POINT('Ctrl Pts',(3.25170985554867,-11.0410108839757,-16.4557907238688));
#43668=CARTESIAN_POINT('Ctrl Pts',(3.31411012526371,-11.0273242338295,-16.4644422848758));
#43669=CARTESIAN_POINT('Ctrl Pts',(3.38253634575007,-11.0119255987223,-16.4741787833184));
#43670=CARTESIAN_POINT('Ctrl Pts',(3.45698851700775,-10.994564758146,-16.4851583180191));
#43671=CARTESIAN_POINT('Ctrl Pts',(3.53144210666456,-10.9772035868257,-16.4961380618926));
#43672=CARTESIAN_POINT('Ctrl Pts',(3.61192187669741,-10.9578801348977,-16.5083608888898));
#43673=CARTESIAN_POINT('Ctrl Pts',(3.69842782710629,-10.9363001083078,-16.522012771196));
#43674=CARTESIAN_POINT('Ctrl Pts',(3.77372513295017,-10.9175162228689,-16.5338957682904));
#43675=CARTESIAN_POINT('Ctrl Pts',(3.8535881563074,-10.8970219759816,-16.5468619110245));
#43676=CARTESIAN_POINT('Ctrl Pts',(3.93801689717799,-10.8745961180402,-16.5610510335625));
#43677=CARTESIAN_POINT('Ctrl Pts',(3.98561590417564,-10.8619529285519,-16.5690505386601));
#43678=CARTESIAN_POINT('Ctrl Pts',(4.03466610085732,-10.848695329643,-16.577439050651));
#43679=CARTESIAN_POINT('Ctrl Pts',(4.08516749280931,-10.8347801299124,-16.5862438846901));
#43680=CARTESIAN_POINT('Ctrl Pts',(4.1104181887853,-10.8278225300471,-16.5906463017096));
#43681=CARTESIAN_POINT('Ctrl Pts',(4.13603167403025,-10.8207004942125,-16.5951527971566));
#43682=CARTESIAN_POINT('Ctrl Pts',(4.16200796064675,-10.8134083791393,-16.5997669698694));
#43683=CARTESIAN_POINT('Ctrl Pts',(4.174996103955,-10.8097623216026,-16.6020740562258));
#43684=CARTESIAN_POINT('Ctrl Pts',(4.18807494701854,-10.8060737420132,-16.6044080617712));
#43685=CARTESIAN_POINT('Ctrl Pts',(4.20124448968825,-10.8023419207142,-16.6067694410442));
#43686=CARTESIAN_POINT('Ctrl Pts',(4.20782926102311,-10.8004760100647,-16.6079501306807));
#43687=CARTESIAN_POINT('Ctrl Pts',(4.21443670722149,-10.7985992888488,-16.6091376637407));
#43688=CARTESIAN_POINT('Ctrl Pts',(4.22106682828487,-10.7967116661656,-16.6103320976921));
#43689=CARTESIAN_POINT('Ctrl Pts',(4.22769694934825,-10.7948240434824,-16.6115265316436));
#43690=CARTESIAN_POINT('Ctrl Pts',(4.23593845337816,-10.7924710696898,-16.6130154304985));
#43691=CARTESIAN_POINT('Ctrl Pts',(4.24102521599387,-10.7910160022244,-16.613936159866));
#43692=CARTESIAN_POINT('Ctrl Pts',(4.37039631656774,-10.7540094238506,-16.6373529733884));
#43693=CARTESIAN_POINT('Ctrl Pts',(4.49374156102956,-10.717036468039,-16.6607655980989));
#43694=CARTESIAN_POINT('Ctrl Pts',(4.61106095067793,-10.6805477767372,-16.6838896275652));
#43695=CARTESIAN_POINT('Ctrl Pts',(4.72934382251309,-10.6437594230846,-16.7072035624728));
#43696=CARTESIAN_POINT('Ctrl Pts',(4.8415014587966,-10.6074633789056,-16.7302241060399));
#43697=CARTESIAN_POINT('Ctrl Pts',(4.94753386085931,-10.5720761142316,-16.7526883702007));
#43698=CARTESIAN_POINT('Ctrl Pts',(5.05275937819688,-10.536958139348,-16.7749816859414));
#43699=CARTESIAN_POINT('Ctrl Pts',(5.15195253014755,-10.5027351059202,-16.7967271939759));
#43700=CARTESIAN_POINT('Ctrl Pts',(5.24511331801198,-10.4697697435228,-16.8176958739611));
#43701=CARTESIAN_POINT('Ctrl Pts',(5.33934566178715,-10.436425206263,-16.8389057403242));
#43702=CARTESIAN_POINT('Ctrl Pts',(5.42740607222585,-10.4043675230243,-16.8593207521068));
#43703=CARTESIAN_POINT('Ctrl Pts',(5.50929455067416,-10.3739261855197,-16.8787328097754));
#43704=CARTESIAN_POINT('Ctrl Pts',(5.59118302912246,-10.3434848480152,-16.8981448674441));
#43705=CARTESIAN_POINT('Ctrl Pts',(5.66689957558038,-10.3146598542873,-16.9165539721416));
#43706=CARTESIAN_POINT('Ctrl Pts',(5.73644419139399,-10.2877345675643,-16.9337810842183));
#43707=CARTESIAN_POINT('Origin',(5.6,-9.91330329119712,-16.8993688492374));
#43708=CARTESIAN_POINT('Origin',(5.59997427807579,-9.91328074797112,-16.8993778521222));
#43709=CARTESIAN_POINT('Ctrl Pts',(5.71191448556623,-6.68641831441597,-8.11927463999024));
#43710=CARTESIAN_POINT('Ctrl Pts',(5.7168759054207,-6.68389354726089,-8.11895890170305));
#43711=CARTESIAN_POINT('Ctrl Pts',(5.76414643547332,-6.65912533256178,-8.11648535844413));
#43712=CARTESIAN_POINT('Ctrl Pts',(5.84911284240881,-6.60163408410921,-8.12175910200295));
#43713=CARTESIAN_POINT('Ctrl Pts',(5.94753227223416,-6.50077330422613,-8.15338978637534));
#43714=CARTESIAN_POINT('Ctrl Pts',(6.01567270245349,-6.3915836303806,-8.20453568510677));
#43715=CARTESIAN_POINT('Ctrl Pts',(6.047167932251,-6.29514927095438,-8.26241592878045));
#43716=CARTESIAN_POINT('Ctrl Pts',(6.05142447490775,-6.23968542500596,-8.30199013668189));
#43717=CARTESIAN_POINT('Ctrl Pts',(6.05077307745104,-6.21841924779483,-8.3182258932679));
#43718=CARTESIAN_POINT('Ctrl Pts',(5.5958237720461,-6.47865804576311,-7.91172653548768));
#43719=CARTESIAN_POINT('Ctrl Pts',(5.60045279817831,-6.47632066092237,-7.91140915880332));
#43720=CARTESIAN_POINT('Ctrl Pts',(5.64456317555875,-6.45339163238793,-7.9088723405948));
#43721=CARTESIAN_POINT('Ctrl Pts',(5.7239570434588,-6.40018274878796,-7.91317737346647));
#43722=CARTESIAN_POINT('Ctrl Pts',(5.81592621444901,-6.30700766623194,-7.94151439908247));
#43723=CARTESIAN_POINT('Ctrl Pts',(5.87944784527059,-6.20656378539426,-7.9878106170003));
#43724=CARTESIAN_POINT('Ctrl Pts',(5.90863950647487,-6.11851238644606,-8.04024697029675));
#43725=CARTESIAN_POINT('Ctrl Pts',(5.91254319769911,-6.0683720124862,-8.0759627702088));
#43726=CARTESIAN_POINT('Ctrl Pts',(5.91194524499303,-6.04924136375469,-8.09057876431784));
#43727=CARTESIAN_POINT('Ctrl Pts',(5.57866412926808,-6.48058524862489,-7.59641729171106));
#43728=CARTESIAN_POINT('Ctrl Pts',(5.5852468819953,-6.47729943274961,-7.59598815404801));
#43729=CARTESIAN_POINT('Ctrl Pts',(5.64791407954493,-6.44510808730406,-7.59260301057773));
#43730=CARTESIAN_POINT('Ctrl Pts',(5.75974745989275,-6.37116557785623,-7.59922899854909));
#43731=CARTESIAN_POINT('Ctrl Pts',(5.88925329949016,-6.24220063399352,-7.63974090522205));
#43732=CARTESIAN_POINT('Ctrl Pts',(5.9800639380707,-6.10141985758422,-7.70592676409287));
#43733=CARTESIAN_POINT('Ctrl Pts',(6.02330320121339,-5.97417844313933,-7.7824635611915));
#43734=CARTESIAN_POINT('Ctrl Pts',(6.02945845991953,-5.89849949258906,-7.83645796824914));
#43735=CARTESIAN_POINT('Ctrl Pts',(6.02852064698248,-5.86900455921464,-7.85896864395111));
#43736=CARTESIAN_POINT('Ctrl Pts',(5.67168409656827,-6.6909363017478,-7.38004192628035));
#43737=CARTESIAN_POINT('Ctrl Pts',(5.68122596548323,-6.68618796862182,-7.3794641679516));
#43738=CARTESIAN_POINT('Ctrl Pts',(5.77200236259354,-6.63970455067086,-7.37500175316839));
#43739=CARTESIAN_POINT('Ctrl Pts',(5.93302216132211,-6.53360398538186,-7.38571690041905));
#43740=CARTESIAN_POINT('Ctrl Pts',(6.11944510133186,-6.34883503080788,-7.44589119956688));
#43741=CARTESIAN_POINT('Ctrl Pts',(6.25156373113289,-6.14507680730802,-7.54366771878732));
#43742=CARTESIAN_POINT('Ctrl Pts',(6.31599311123261,-5.956762721389,-7.65805067473802));
#43743=CARTESIAN_POINT('Ctrl Pts',(6.32552838135578,-5.84142450668251,-7.74047848722718));
#43744=CARTESIAN_POINT('Ctrl Pts',(6.32408019253049,-5.79585959851974,-7.77522307010303));
#43745=CARTESIAN_POINT('',(5.99998739574857,-6.0954555957118,-8.13557466247078));
#43746=CARTESIAN_POINT('',(5.99999998791472,-6.44014497786806,-7.42970782965953));
#43747=CARTESIAN_POINT('Ctrl Pts',(5.99998739574857,-6.0954555957118,-8.13557466247078));
#43748=CARTESIAN_POINT('Ctrl Pts',(5.9999852507051,-6.09852553841938,-8.11170571829663));
#43749=CARTESIAN_POINT('Ctrl Pts',(5.99998676083024,-6.10206236150406,-8.08798616475802));
#43750=CARTESIAN_POINT('Ctrl Pts',(5.99999979802884,-6.10612978800577,-8.06451310294154));
#43751=CARTESIAN_POINT('Ctrl Pts',(6.00000674447814,-6.10829698456647,-8.05200624170718));
#43752=CARTESIAN_POINT('Ctrl Pts',(6.00001622801463,-6.11061426766856,-8.03956966677541));
#43753=CARTESIAN_POINT('Ctrl Pts',(6.00002591391681,-6.11308675051894,-8.02721971866998));
#43754=CARTESIAN_POINT('Ctrl Pts',(6.00004505311857,-6.11797234064786,-8.00281640094944));
#43755=CARTESIAN_POINT('Ctrl Pts',(6.00006656966194,-6.12346689318343,-7.97875098022345));
#43756=CARTESIAN_POINT('Ctrl Pts',(6.00008775917612,-6.12957143329631,-7.95514338530885));
#43757=CARTESIAN_POINT('Ctrl Pts',(6.00010095494808,-6.13337303622687,-7.94044175335113));
#43758=CARTESIAN_POINT('Ctrl Pts',(6.00011343875003,-6.1374102015521,-7.92591787378617));
#43759=CARTESIAN_POINT('Ctrl Pts',(6.00012222024973,-6.14167330870094,-7.91160086667585));
#43760=CARTESIAN_POINT('Ctrl Pts',(6.000136666637,-6.14868651816037,-7.88804805268568));
#43761=CARTESIAN_POINT('Ctrl Pts',(6.00013998635602,-6.15631378632345,-7.8650561610896));
#43762=CARTESIAN_POINT('Ctrl Pts',(6.00012429255407,-6.16447084918693,-7.84274607149054));
#43763=CARTESIAN_POINT('Ctrl Pts',(6.0001192880969,-6.16707198254142,-7.83563180509723));
#43764=CARTESIAN_POINT('Ctrl Pts',(6.00011246210241,-6.16972662339921,-7.82858674352641));
#43765=CARTESIAN_POINT('Ctrl Pts',(6.00010394449708,-6.17243108075715,-7.8216143988938));
#43766=CARTESIAN_POINT('Ctrl Pts',(6.00009903895563,-6.1739886579333,-7.81759881889872));
#43767=CARTESIAN_POINT('Ctrl Pts',(6.00009357731723,-6.1755627513357,-7.81360735402424));
#43768=CARTESIAN_POINT('Ctrl Pts',(6.0000876760401,-6.1771526374344,-7.80964059033505));
#43769=CARTESIAN_POINT('Ctrl Pts',(6.0000691361879,-6.18214753136233,-7.79717833666742));
#43770=CARTESIAN_POINT('Ctrl Pts',(6.00005142588151,-6.1873620291741,-7.78478770193526));
#43771=CARTESIAN_POINT('Ctrl Pts',(6.00003087539323,-6.19270944962128,-7.77268560910881));
#43772=CARTESIAN_POINT('Ctrl Pts',(6.00001013895765,-6.19810525521661,-7.76047401272637));
#43773=CARTESIAN_POINT('Ctrl Pts',(5.99998605869799,-6.20363625240065,-7.74855670970051));
#43774=CARTESIAN_POINT('Ctrl Pts',(5.9999679811411,-6.20916221676034,-7.73714583029187));
#43775=CARTESIAN_POINT('Ctrl Pts',(5.9999573196392,-6.21242123455163,-7.73041609832358));
#43776=CARTESIAN_POINT('Ctrl Pts',(5.9999490416756,-6.21567752560429,-7.72386226018103));
#43777=CARTESIAN_POINT('Ctrl Pts',(5.99994794613539,-6.21889483549495,-7.7175251660673));
#43778=CARTESIAN_POINT('Ctrl Pts',(5.99994403320275,-6.23038607679768,-7.69489101514807));
#43779=CARTESIAN_POINT('Ctrl Pts',(5.99996394684146,-6.24267989067564,-7.67262426789394));
#43780=CARTESIAN_POINT('Ctrl Pts',(5.99998990573708,-6.25576816623256,-7.65088898742367));
#43781=CARTESIAN_POINT('Ctrl Pts',(6.00001571597285,-6.26878148863728,-7.6292781792552));
#43782=CARTESIAN_POINT('Ctrl Pts',(6.00004678534973,-6.28258014939282,-7.60819371272941));
#43783=CARTESIAN_POINT('Ctrl Pts',(6.00006724493389,-6.29710486864247,-7.58779355113598));
#43784=CARTESIAN_POINT('Ctrl Pts',(6.00007042028293,-6.29935912039344,-7.58462742453473));
#43785=CARTESIAN_POINT('Ctrl Pts',(6.00007335502221,-6.30163076232049,-7.58147775836599));
#43786=CARTESIAN_POINT('Ctrl Pts',(6.00007600935326,-6.30391946558269,-7.57834511352832));
#43787=CARTESIAN_POINT('Ctrl Pts',(6.00009312908458,-6.31868099461108,-7.55814038516948));
#43788=CARTESIAN_POINT('Ctrl Pts',(6.00009752375211,-6.33415600309633,-7.53864552190102));
#43789=CARTESIAN_POINT('Ctrl Pts',(6.00008809825533,-6.35023290373304,-7.51999565200792));
#43790=CARTESIAN_POINT('Ctrl Pts',(6.00007855534302,-6.36651007792217,-7.50111345650805));
#43791=CARTESIAN_POINT('Ctrl Pts',(6.00005445377403,-6.38340350354771,-7.48309820525124));
#43792=CARTESIAN_POINT('Ctrl Pts',(6.00003199274435,-6.40075610903027,-7.46606026200349));
#43793=CARTESIAN_POINT('Ctrl Pts',(6.00001529295041,-6.41365778539459,-7.45339253726803));
#43794=CARTESIAN_POINT('Ctrl Pts',(5.99999988409202,-6.42681233722686,-7.44126443393272));
#43795=CARTESIAN_POINT('Ctrl Pts',(5.99999988835028,-6.44014484659843,-7.4297076782196));
#43796=CARTESIAN_POINT('',(5.72001531319857,-6.64701102057165,-7.39409186140856));
#43797=CARTESIAN_POINT('Ctrl Pts',(5.72001583932162,-6.64701193943656,-7.39409288351738));
#43798=CARTESIAN_POINT('Ctrl Pts',(5.77262443156593,-6.61776628438278,-7.39330399074791));
#43799=CARTESIAN_POINT('Ctrl Pts',(5.82215801012378,-6.58572561272941,-7.39609520796243));
#43800=CARTESIAN_POINT('Ctrl Pts',(5.86878812167724,-6.55120568929977,-7.40209507796886));
#43801=CARTESIAN_POINT('Ctrl Pts',(5.91541823323071,-6.51668576587012,-7.40809494797528));
#43802=CARTESIAN_POINT('Ctrl Pts',(5.95914511084897,-6.47968695772417,-7.41730389800646));
#43803=CARTESIAN_POINT('Ctrl Pts',(6.00000005306065,-6.44014511329477,-7.42970798589524));
#43804=CARTESIAN_POINT('',(5.732785031286,-6.65588656996562,-8.10254649550562));
#43805=CARTESIAN_POINT('Origin',(5.89877289526359,-6.9591999244832,-7.74135689824448));
#43806=CARTESIAN_POINT('Ctrl Pts',(5.73278241139749,-6.65588178673174,-8.1025521928097));
#43807=CARTESIAN_POINT('Ctrl Pts',(5.74767871087474,-6.64180973010437,-8.09758786339362));
#43808=CARTESIAN_POINT('Ctrl Pts',(5.76173626685014,-6.62751756008203,-8.09338492315945));
#43809=CARTESIAN_POINT('Ctrl Pts',(5.77495191999532,-6.61320028672805,-8.08982392122754));
#43810=CARTESIAN_POINT('Ctrl Pts',(5.78903153877291,-6.59794702996169,-8.08603012086695));
#43811=CARTESIAN_POINT('Ctrl Pts',(5.8021557260155,-6.58266504801332,-8.08296512516117));
#43812=CARTESIAN_POINT('Ctrl Pts',(5.81434877348918,-6.56754232129755,-8.08050383231665));
#43813=CARTESIAN_POINT('Ctrl Pts',(5.8170465327943,-6.56419635903469,-8.07995926167602));
#43814=CARTESIAN_POINT('Ctrl Pts',(5.81969880745718,-6.56085802597551,-8.07944430865289));
#43815=CARTESIAN_POINT('Ctrl Pts',(5.82230601940132,-6.557529086438,-8.07895772156423));
#43816=CARTESIAN_POINT('Ctrl Pts',(5.83435660366248,-6.5421426632179,-8.0767087065866));
#43817=CARTESIAN_POINT('Ctrl Pts',(5.84544361982858,-6.52696063865089,-8.07506371238998));
#43818=CARTESIAN_POINT('Ctrl Pts',(5.85563656380534,-6.51215017531834,-8.07388973150728));
#43819=CARTESIAN_POINT('Ctrl Pts',(5.85625536372891,-6.51125105200331,-8.0738184607064));
#43820=CARTESIAN_POINT('Ctrl Pts',(5.85687087189929,-6.51035328450495,-8.07374893287642));
#43821=CARTESIAN_POINT('Ctrl Pts',(5.85748310512795,-6.50945690510748,-8.07368112089833));
#43822=CARTESIAN_POINT('Ctrl Pts',(5.86845369943394,-6.49339470159828,-8.07246599949395));
#43823=CARTESIAN_POINT('Ctrl Pts',(5.87837191641668,-6.47778228369507,-8.07179977148889));
#43824=CARTESIAN_POINT('Ctrl Pts',(5.88734075182149,-6.46277817850691,-8.07154035811203));
#43825=CARTESIAN_POINT('Ctrl Pts',(5.89145115664845,-6.45590181790867,-8.0714214693212));
#43826=CARTESIAN_POINT('Ctrl Pts',(5.89536230645623,-6.44915254784001,-8.07138837201233));
#43827=CARTESIAN_POINT('Ctrl Pts',(5.89908474664214,-6.44254252224732,-8.07142897801076));
#43828=CARTESIAN_POINT('Ctrl Pts',(5.90118652860432,-6.43881033801699,-8.07145190516359));
#43829=CARTESIAN_POINT('Ctrl Pts',(5.90322815576402,-6.43512251272292,-8.07149834565494));
#43830=CARTESIAN_POINT('Ctrl Pts',(5.90521156699562,-6.43148099641133,-8.07156624623327));
#43831=CARTESIAN_POINT('Ctrl Pts',(5.90881698396612,-6.42486149940584,-8.07168967494717));
#43832=CARTESIAN_POINT('Ctrl Pts',(5.91223006400224,-6.41839514362771,-8.07188393007648));
#43833=CARTESIAN_POINT('Ctrl Pts',(5.91546372479684,-6.41209325625483,-8.07213628843071));
#43834=CARTESIAN_POINT('Ctrl Pts',(5.91797000559497,-6.407208916085,-8.07233188127042));
#43835=CARTESIAN_POINT('Ctrl Pts',(5.92036843480492,-6.40242343749142,-8.07256237877867));
#43836=CARTESIAN_POINT('Ctrl Pts',(5.9226649903207,-6.39774121022765,-8.07282239460074));
#43837=CARTESIAN_POINT('Ctrl Pts',(5.92381326807859,-6.39540009659577,-8.07295240251177));
#43838=CARTESIAN_POINT('Ctrl Pts',(5.92493607055781,-6.39308479275801,-8.07308979378538));
#43839=CARTESIAN_POINT('Ctrl Pts',(5.92603412444383,-6.39079580758985,-8.07323393102872));
#43840=CARTESIAN_POINT('Ctrl Pts',(5.92680721312934,-6.38918423956271,-8.07333541135988));
#43841=CARTESIAN_POINT('Ctrl Pts',(5.92725985702953,-6.38823408194907,-8.07339689715456));
#43842=CARTESIAN_POINT('Ctrl Pts',(5.9280443649142,-6.38657648170654,-8.07350892546876));
#43843=CARTESIAN_POINT('Ctrl Pts',(5.92837413013627,-6.38587971508029,-8.07355601618974));
#43844=CARTESIAN_POINT('Ctrl Pts',(5.92876221469405,-6.38505782686567,-8.07361225806707));
#43845=CARTESIAN_POINT('Ctrl Pts',(5.9292547487712,-6.38400829604505,-8.07368595978997));
#43846=CARTESIAN_POINT('Ctrl Pts',(5.93919911343165,-6.36281805218796,-8.07517401278488));
#43847=CARTESIAN_POINT('Ctrl Pts',(5.94793617525635,-6.34198588487123,-8.07733346319839));
#43848=CARTESIAN_POINT('Ctrl Pts',(5.95554257224008,-6.32167919878544,-8.08002789788969));
#43849=CARTESIAN_POINT('Ctrl Pts',(5.95842928866023,-6.31397257444173,-8.08105046729844));
#43850=CARTESIAN_POINT('Ctrl Pts',(5.96115320640223,-6.30634113839236,-8.08215034001233));
#43851=CARTESIAN_POINT('Ctrl Pts',(5.96371874232458,-6.29879233915127,-8.08332088594868));
#43852=CARTESIAN_POINT('Ctrl Pts',(5.97059811501146,-6.27855056320671,-8.08645965382682));
#43853=CARTESIAN_POINT('Ctrl Pts',(5.97633958227157,-6.25890622506058,-8.09010441703621));
#43854=CARTESIAN_POINT('Ctrl Pts',(5.98107332870542,-6.23999045283084,-8.09411401504301));
#43855=CARTESIAN_POINT('Ctrl Pts',(5.98611100847453,-6.21986018087598,-8.09838105195412));
#43856=CARTESIAN_POINT('Ctrl Pts',(5.99000695822762,-6.20055486208303,-8.10306152212758));
#43857=CARTESIAN_POINT('Ctrl Pts',(5.9929112894325,-6.18218287564415,-8.10801549090924));
#43858=CARTESIAN_POINT('Ctrl Pts',(5.99361898202317,-6.17770621035992,-8.10922261459931));
#43859=CARTESIAN_POINT('Ctrl Pts',(5.99426778624819,-6.17328474936486,-8.11044610040774));
#43860=CARTESIAN_POINT('Ctrl Pts',(5.99485986278369,-6.16891966840703,-8.11168415004286));
#43861=CARTESIAN_POINT('Ctrl Pts',(5.99739682055055,-6.15021596141139,-8.1169890041441));
#43862=CARTESIAN_POINT('Ctrl Pts',(5.99889426451141,-6.1325504049427,-8.12255868624874));
#43863=CARTESIAN_POINT('Ctrl Pts',(5.99956526180203,-6.11598503100764,-8.12825285692962));
#43864=CARTESIAN_POINT('Ctrl Pts',(5.99985052305375,-6.10894258930165,-8.1306736211841));
#43865=CARTESIAN_POINT('Ctrl Pts',(5.9999861332358,-6.10209851722248,-8.1331172754017));
#43866=CARTESIAN_POINT('Ctrl Pts',(5.99998739574857,-6.0954555957118,-8.13557466247077));
#43867=CARTESIAN_POINT('Ctrl Pts',(5.99970218884702,-6.00683889572887,-8.08733125571215));
#43868=CARTESIAN_POINT('Ctrl Pts',(5.99970218884702,-6.35108172829139,-8.34755327096762));
#43869=CARTESIAN_POINT('Ctrl Pts',(5.99970218884702,-7.06961527830159,-8.96852445968389));
#43870=CARTESIAN_POINT('Ctrl Pts',(5.99970218884702,-8.03090172607189,-10.0756749999051));
#43871=CARTESIAN_POINT('Ctrl Pts',(5.99970218884702,-8.85234907043669,-11.3899817047342));
#43872=CARTESIAN_POINT('Ctrl Pts',(5.99970218884702,-9.45956831200042,-12.8151106326851));
#43873=CARTESIAN_POINT('Ctrl Pts',(5.99970218884702,-9.8386683762363,-14.3182479126164));
#43874=CARTESIAN_POINT('Ctrl Pts',(5.99970218884702,-9.96649290703559,-15.7255792696104));
#43875=CARTESIAN_POINT('Ctrl Pts',(5.99970218884702,-9.92671360417176,-16.6207571809547));
#43876=CARTESIAN_POINT('Ctrl Pts',(5.99970218884702,-9.88830104579072,-16.997130460064));
#43877=CARTESIAN_POINT('Ctrl Pts',(6.00690077783577,-6.11926434196324,-7.93859628419385));
#43878=CARTESIAN_POINT('Ctrl Pts',(6.00690077783577,-6.47001458246786,-8.20373515941894));
#43879=CARTESIAN_POINT('Ctrl Pts',(6.00690077783577,-7.20199451917009,-8.83632563854109));
#43880=CARTESIAN_POINT('Ctrl Pts',(6.00690077783577,-8.18145565313282,-9.96441656147784));
#43881=CARTESIAN_POINT('Ctrl Pts',(6.00690077783577,-9.01829931826486,-11.3033520080679));
#43882=CARTESIAN_POINT('Ctrl Pts',(6.00690077783577,-9.63699837320393,-12.7554188501705));
#43883=CARTESIAN_POINT('Ctrl Pts',(6.00690077783577,-10.0232003582101,-14.2867394397005));
#43884=CARTESIAN_POINT('Ctrl Pts',(6.00690077783577,-10.1534445291253,-15.7206518840566));
#43885=CARTESIAN_POINT('Ctrl Pts',(6.00690077783577,-10.1129217549952,-16.6325905678065));
#43886=CARTESIAN_POINT('Ctrl Pts',(6.00690077783577,-10.0737824039727,-17.0160648976741));
#43887=CARTESIAN_POINT('Ctrl Pts',(5.89988019332797,-6.21151563398466,-7.81655101996858));
#43888=CARTESIAN_POINT('Ctrl Pts',(5.89988019332797,-6.56760556234862,-8.08572445053743));
#43889=CARTESIAN_POINT('Ctrl Pts',(5.89988019332797,-7.31061900246748,-8.72784919959662));
#43890=CARTESIAN_POINT('Ctrl Pts',(5.89988019332797,-8.30499347090845,-9.87312286385892));
#43891=CARTESIAN_POINT('Ctrl Pts',(5.89988019332797,-9.15447066813245,-11.2322675542128));
#43892=CARTESIAN_POINT('Ctrl Pts',(5.89988019332797,-9.78258954439533,-12.7064384436462));
#43893=CARTESIAN_POINT('Ctrl Pts',(5.89988019332797,-10.174619047903,-14.2608849963055));
#43894=CARTESIAN_POINT('Ctrl Pts',(5.89988019332797,-10.3068486672459,-15.7166086918849));
#43895=CARTESIAN_POINT('Ctrl Pts',(5.89988019332797,-10.265715833855,-16.6423005157086));
#43896=CARTESIAN_POINT('Ctrl Pts',(5.89988019332797,-10.2259801093083,-17.0316016501771));
#43897=CARTESIAN_POINT('Ctrl Pts',(5.72194804881404,-6.24586098767294,-7.77111330658825));
#43898=CARTESIAN_POINT('Ctrl Pts',(5.72194804881404,-6.60393889326845,-8.04178881075682));
#43899=CARTESIAN_POINT('Ctrl Pts',(5.72194804881404,-7.35106013034822,-8.68746318894069));
#43900=CARTESIAN_POINT('Ctrl Pts',(5.72194804881404,-8.35098686517315,-9.83913402461853));
#43901=CARTESIAN_POINT('Ctrl Pts',(5.72194804881404,-9.20516755346836,-11.2058026597302));
#43902=CARTESIAN_POINT('Ctrl Pts',(5.72194804881404,-9.83679344939564,-12.6882029333488));
#43903=CARTESIAN_POINT('Ctrl Pts',(5.72194804881404,-10.2309925505249,-14.2512593316319));
#43904=CARTESIAN_POINT('Ctrl Pts',(5.72194804881404,-10.3639613565709,-15.7151034027759));
#43905=CARTESIAN_POINT('Ctrl Pts',(5.72194804881404,-10.3226013968126,-16.6459155501193));
#43906=CARTESIAN_POINT('Ctrl Pts',(5.72194804881404,-10.2826436411267,-17.0373860164276));
#43907=CARTESIAN_POINT('Ctrl Pts',(5.73278343892927,-6.6558836604587,-8.10254996082558));
#43908=CARTESIAN_POINT('Ctrl Pts',(5.73338951161688,-6.8647510746576,-8.27821818491745));
#43909=CARTESIAN_POINT('Ctrl Pts',(5.73395354695775,-7.06684952503181,-8.46233459868889));
#43910=CARTESIAN_POINT('Ctrl Pts',(5.73447555411707,-7.26144433882555,-8.65430876002968));
#43911=CARTESIAN_POINT('Ctrl Pts',(5.73532470425807,-7.57799213059554,-8.96659353095752));
#43912=CARTESIAN_POINT('Ctrl Pts',(5.73606264101921,-7.87468578917018,-9.29967289629772));
#43913=CARTESIAN_POINT('Ctrl Pts',(5.73668942284259,-8.14888325133039,-9.65097686333643));
#43914=CARTESIAN_POINT('Ctrl Pts',(5.73681690262199,-8.20465167135523,-9.72242780615646));
#43915=CARTESIAN_POINT('Ctrl Pts',(5.73693978433038,-8.25948937240233,-9.79463252356511));
#43916=CARTESIAN_POINT('Ctrl Pts',(5.73705806848171,-8.31337392813761,-9.86756921526368));
#43917=CARTESIAN_POINT('Ctrl Pts',(5.73707478428951,-8.32098884414092,-9.87787656165014));
#43918=CARTESIAN_POINT('Ctrl Pts',(5.7370914082791,-8.32858472468886,-9.88819852625709));
#43919=CARTESIAN_POINT('Ctrl Pts',(5.73710794045192,-8.33616152004608,-9.89853503587695));
#43920=CARTESIAN_POINT('Ctrl Pts',(5.73767502817431,-8.59606127247122,-10.2530986956414));
#43921=CARTESIAN_POINT('Ctrl Pts',(5.73813408881152,-8.8335074050344,-10.6247800471307));
#43922=CARTESIAN_POINT('Ctrl Pts',(5.73848518367663,-9.04647680356154,-11.0106030415808));
#43923=CARTESIAN_POINT('Ctrl Pts',(5.73855071710724,-9.08622849658298,-11.0826186332201));
#43924=CARTESIAN_POINT('Ctrl Pts',(5.7386124889711,-9.12512733602101,-11.1551268007166));
#43925=CARTESIAN_POINT('Ctrl Pts',(5.73867049958713,-9.16316004565204,-11.228108028484));
#43926=CARTESIAN_POINT('Ctrl Pts',(5.73897977938334,-9.36592894363117,-11.6172026596877));
#43927=CARTESIAN_POINT('Ctrl Pts',(5.7391821511709,-9.54408075696241,-12.0197473164057));
#43928=CARTESIAN_POINT('Ctrl Pts',(5.73927764632406,-9.69602494696988,-12.4324947986501));
#43929=CARTESIAN_POINT('Ctrl Pts',(5.73929840882887,-9.72906057097882,-12.5222341340823));
#43930=CARTESIAN_POINT('Ctrl Pts',(5.73931411902672,-9.76085723580346,-12.6124555976131));
#43931=CARTESIAN_POINT('Ctrl Pts',(5.73932477703702,-9.79139843860385,-12.7031255267129));
#43932=CARTESIAN_POINT('Ctrl Pts',(5.7393735862753,-9.9312643988762,-13.1183559544157));
#43933=CARTESIAN_POINT('Ctrl Pts',(5.73931644079582,-10.0448015289714,-13.5429957199903));
#43934=CARTESIAN_POINT('Ctrl Pts',(5.73915333152432,-10.1308662049193,-13.9736567908168));
#43935=CARTESIAN_POINT('Ctrl Pts',(5.7391174741561,-10.1497863603912,-14.0683318049964));
#43936=CARTESIAN_POINT('Ctrl Pts',(5.73907649563359,-10.1673787538509,-14.1632976307152));
#43937=CARTESIAN_POINT('Ctrl Pts',(5.73903039564908,-10.1836311146258,-14.2585179559314));
#43938=CARTESIAN_POINT('Ctrl Pts',(5.73900084443474,-10.194049274242,-14.31955650661));
#43939=CARTESIAN_POINT('Ctrl Pts',(5.73896918874735,-10.2039167967521,-14.3806996319841));
#43940=CARTESIAN_POINT('Ctrl Pts',(5.73893542849059,-10.2132325779621,-14.4419375696272));
#43941=CARTESIAN_POINT('Ctrl Pts',(5.73869640194468,-10.2791893928211,-14.8755092931832));
#43942=CARTESIAN_POINT('Ctrl Pts',(5.73835187087254,-10.3174891438493,-15.3138381747238));
#43943=CARTESIAN_POINT('Ctrl Pts',(5.73790179978098,-10.3277354971762,-15.7534299763543));
#43944=CARTESIAN_POINT('Ctrl Pts',(5.73786596841969,-10.3285512367224,-15.7884270533972));
#43945=CARTESIAN_POINT('Ctrl Pts',(5.73782946811548,-10.3291891649064,-15.8234321079199));
#43946=CARTESIAN_POINT('Ctrl Pts',(5.73779229884493,-10.3296490796853,-15.8584433625832));
#43947=CARTESIAN_POINT('Ctrl Pts',(5.73741169570001,-10.33435848099,-16.2169490161895));
#43948=CARTESIAN_POINT('Ctrl Pts',(5.73696095042926,-10.3204029417981,-16.576106838384));
#43949=CARTESIAN_POINT('Ctrl Pts',(5.73644003522184,-10.287721746545,-16.9337799081518));
#43950=CARTESIAN_POINT('Ctrl Pts',(5.9999999993059,-6.09545559723548,-8.1355746616996));
#43951=CARTESIAN_POINT('Ctrl Pts',(5.9999999993156,-6.21632000246365,-8.22886961536299));
#43952=CARTESIAN_POINT('Ctrl Pts',(5.99999999835916,-6.33462436300169,-8.3246240217504));
#43953=CARTESIAN_POINT('Ctrl Pts',(5.99999999609535,-6.45047432846417,-8.42285685600839));
#43954=CARTESIAN_POINT('Ctrl Pts',(5.99999999382032,-6.56689816955468,-8.52157629748484));
#43955=CARTESIAN_POINT('Ctrl Pts',(5.9999999902401,-6.68084357504832,-8.62279909937612));
#43956=CARTESIAN_POINT('Ctrl Pts',(5.99999999039156,-6.79238504196438,-8.7265856228609));
#43957=CARTESIAN_POINT('Ctrl Pts',(5.99999999048548,-6.86154926350248,-8.79094118766957));
#43958=CARTESIAN_POINT('Ctrl Pts',(5.99999999231393,-6.92978852009233,-8.85628328040707));
#43959=CARTESIAN_POINT('Ctrl Pts',(5.99999999505289,-6.99711341831894,-8.9226333709323));
#43960=CARTESIAN_POINT('Ctrl Pts',(5.9999999972169,-7.05030583281631,-8.97505560416431));
#43961=CARTESIAN_POINT('Ctrl Pts',(5.99999999999962,-7.10292736651186,-9.02810717281959));
#43962=CARTESIAN_POINT('Ctrl Pts',(5.99999999999962,-7.15498473399384,-9.08180207094362));
#43963=CARTESIAN_POINT('Ctrl Pts',(5.99999999999962,-7.28285593185063,-9.2136956198115));
#43964=CARTESIAN_POINT('Ctrl Pts',(5.99999998462023,-7.40736537484194,-9.34940593933384));
#43965=CARTESIAN_POINT('Ctrl Pts',(5.99999998025195,-7.52813264110009,-9.48859830995591));
#43966=CARTESIAN_POINT('Ctrl Pts',(5.99999997588669,-7.64881610288076,-9.62769409029944));
#43967=CARTESIAN_POINT('Ctrl Pts',(5.99999998175304,-7.76576225718329,-9.77026676590069));
#43968=CARTESIAN_POINT('Ctrl Pts',(5.99999999007195,-7.87862812274216,-9.91594547377447));
#43969=CARTESIAN_POINT('Ctrl Pts',(5.99999999337621,-7.92345823073153,-9.9738087805714));
#43970=CARTESIAN_POINT('Ctrl Pts',(5.99999999675166,-7.96764503899738,-10.0321617334311));
#43971=CARTESIAN_POINT('Ctrl Pts',(5.99999999861007,-8.01116883173431,-10.0909796561054));
#43972=CARTESIAN_POINT('Ctrl Pts',(5.99999999947163,-8.03134643779373,-10.1182476122812));
#43973=CARTESIAN_POINT('Ctrl Pts',(5.99999999999962,-8.05138156043679,-10.1456154909224));
#43974=CARTESIAN_POINT('Ctrl Pts',(5.99999999999962,-8.07127252639277,-10.1730804652344));
#43975=CARTESIAN_POINT('Ctrl Pts',(5.99999999999962,-8.19608224407421,-10.3454147650165));
#43976=CARTESIAN_POINT('Ctrl Pts',(5.99999998564321,-8.31516617400978,-10.5216179734177));
#43977=CARTESIAN_POINT('Ctrl Pts',(5.99999998504708,-8.42843403911075,-10.7014457915073));
#43978=CARTESIAN_POINT('Ctrl Pts',(5.99999998445023,-8.54183900473007,-10.8814912749255));
#43979=CARTESIAN_POINT('Ctrl Pts',(5.99999999412996,-8.64941414963471,-11.0651706214989));
#43980=CARTESIAN_POINT('Ctrl Pts',(5.9999999983805,-8.7510270922678,-11.2522696464205));
#43981=CARTESIAN_POINT('Ctrl Pts',(5.99999999937175,-8.77472398227683,-11.295902523291));
#43982=CARTESIAN_POINT('Ctrl Pts',(5.99999999999963,-8.79809642264477,-11.3397214970844));
#43983=CARTESIAN_POINT('Ctrl Pts',(5.99999999999963,-8.82114237775435,-11.3837240507049));
#43984=CARTESIAN_POINT('Ctrl Pts',(5.99999999999963,-8.82427077957775,-11.3896972320431));
#43985=CARTESIAN_POINT('Ctrl Pts',(5.99999999998808,-8.82739320263783,-11.3956737752782));
#43986=CARTESIAN_POINT('Ctrl Pts',(5.99999999996603,-8.83050963567541,-11.4016536636707));
#43987=CARTESIAN_POINT('Ctrl Pts',(5.99999999925238,-8.93137509851493,-11.5951967955668));
#43988=CARTESIAN_POINT('Ctrl Pts',(5.99999999047918,-9.0259620484505,-11.7922463184232));
#43989=CARTESIAN_POINT('Ctrl Pts',(5.99999999007257,-9.11398098223997,-11.9922073236602));
#43990=CARTESIAN_POINT('Ctrl Pts',(5.9999999896657,-9.20205429336523,-12.1922918630763));
#43991=CARTESIAN_POINT('Ctrl Pts',(5.99999999693156,-9.28355123916782,-12.395290972675));
#43992=CARTESIAN_POINT('Ctrl Pts',(5.99999999941396,-9.35822889393878,-12.6005865753142));
#43993=CARTESIAN_POINT('Ctrl Pts',(5.99999999977838,-9.36919170568964,-12.6307243327453));
#43994=CARTESIAN_POINT('Ctrl Pts',(5.99999999999963,-9.38000764283712,-12.6609115505662));
#43995=CARTESIAN_POINT('Ctrl Pts',(5.99999999999963,-9.3906760268368,-12.6911462437714));
#43996=CARTESIAN_POINT('Ctrl Pts',(5.99999999999963,-9.40612090546474,-12.7349177434587));
#43997=CARTESIAN_POINT('Ctrl Pts',(5.99999999953036,-9.42125510905206,-12.7787890010936));
#43998=CARTESIAN_POINT('Ctrl Pts',(5.99999999872729,-9.43607771846652,-12.82275774804));
#43999=CARTESIAN_POINT('Ctrl Pts',(5.99999999501562,-9.50458504372292,-13.0259730635049));
#44000=CARTESIAN_POINT('Ctrl Pts',(5.99999998445147,-9.56644039632124,-13.2312698568886));
#44001=CARTESIAN_POINT('Ctrl Pts',(5.99999998419192,-9.62157188140313,-13.4383965501976));
#44002=CARTESIAN_POINT('Ctrl Pts',(5.99999998393238,-9.67670336648502,-13.6455232435065));
#44003=CARTESIAN_POINT('Ctrl Pts',(5.99999999999963,-9.72511108983177,-13.8544804123467));
#44004=CARTESIAN_POINT('Ctrl Pts',(5.99999999999962,-9.76667145420375,-14.0650241450564));
#44005=CARTESIAN_POINT('Ctrl Pts',(5.99999999999962,-9.7835072985383,-14.1503140977091));
#44006=CARTESIAN_POINT('Ctrl Pts',(5.99999999597128,-9.79923294555681,-14.2358640307631));
#44007=CARTESIAN_POINT('Ctrl Pts',(5.99999999157414,-9.81383348710217,-14.3216199001221));
#44008=CARTESIAN_POINT('Ctrl Pts',(5.99999998233605,-9.84450828541726,-14.5017874636846));
#44009=CARTESIAN_POINT('Ctrl Pts',(5.99999997355903,-9.87021359544724,-14.6828643853021));
#44010=CARTESIAN_POINT('Ctrl Pts',(5.99999997660565,-9.89091099303221,-14.8643517495919));
#44011=CARTESIAN_POINT('Ctrl Pts',(5.99999997965609,-9.91163423873525,-15.0460657658943));
#44012=CARTESIAN_POINT('Ctrl Pts',(5.99999999487371,-9.92733703853263,-15.2281907937088));
#44013=CARTESIAN_POINT('Ctrl Pts',(5.9999999991423,-9.9380328969175,-15.4102231927563));
#44014=CARTESIAN_POINT('Ctrl Pts',(5.99999999968359,-9.93938920244837,-15.4333061039863));
#44015=CARTESIAN_POINT('Ctrl Pts',(5.99999999999963,-9.94066506549936,-15.4563875273483));
#44016=CARTESIAN_POINT('Ctrl Pts',(5.99999999999963,-9.94186057345894,-15.4794664384282));
#44017=CARTESIAN_POINT('Ctrl Pts',(5.99999999999963,-9.94849006795469,-15.6074467774512));
#44018=CARTESIAN_POINT('Ctrl Pts',(5.99999999306092,-9.95260895372041,-15.7353412105235));
#44019=CARTESIAN_POINT('Ctrl Pts',(5.99999999145036,-9.9542448330683,-15.8632214087634));
#44020=CARTESIAN_POINT('Ctrl Pts',(5.99999998952808,-9.95619734135282,-16.0158531702759));
#44021=CARTESIAN_POINT('Ctrl Pts',(5.99999999274889,-9.95461394974177,-16.1684648502107));
#44022=CARTESIAN_POINT('Ctrl Pts',(5.99999999547939,-9.94950717517158,-16.3211506606758));
#44023=CARTESIAN_POINT('Ctrl Pts',(5.99999999819765,-9.94442331957945,-16.4731512239872));
#44024=CARTESIAN_POINT('Ctrl Pts',(5.99999999961507,-9.93584763338568,-16.6252257133007));
#44025=CARTESIAN_POINT('Ctrl Pts',(5.99999999985074,-9.92374096699956,-16.7774656808718));
#44026=CARTESIAN_POINT('Ctrl Pts',(5.99999999991362,-9.92051052208515,-16.8180881621829));
#44027=CARTESIAN_POINT('Ctrl Pts',(5.99999999993317,-9.91702838885872,-16.8587223964478));
#44028=CARTESIAN_POINT('Ctrl Pts',(5.99999999993286,-9.91329319860811,-16.8993700414499));
#44029=CARTESIAN_POINT('Ctrl Pts',(-5.843530343916,-6.4054425445004,-7.94861181432332));
#44030=CARTESIAN_POINT('Ctrl Pts',(-3.895686895944,-7.50111660415432,-7.93455833697476));
#44031=CARTESIAN_POINT('Ctrl Pts',(0.0001666015266142,-8.59741061726458,
-7.91991847694548));
#44032=CARTESIAN_POINT('Ctrl Pts',(3.896020098997,-7.50102283673824,-7.93455958914352));
#44033=CARTESIAN_POINT('Ctrl Pts',(5.844030148496,-6.4051613892978,-7.94861542050703));
#44034=CARTESIAN_POINT('Ctrl Pts',(-5.843530343916,-7.02207566989846,-8.43809511982169));
#44035=CARTESIAN_POINT('Ctrl Pts',(-3.895686895944,-8.0413509136543,-8.43217728733141));
#44036=CARTESIAN_POINT('Ctrl Pts',(0.0001666015266142,-9.06227941450043,
-8.42460895688274));
#44037=CARTESIAN_POINT('Ctrl Pts',(3.896020098997,-8.04126359234196,-8.43217793466096));
#44038=CARTESIAN_POINT('Ctrl Pts',(5.844030148496,-7.02181411900168,-8.43809663834368));
#44039=CARTESIAN_POINT('Ctrl Pts',(-5.843530343916,-8.22106584996092,-9.63752182400419));
#44040=CARTESIAN_POINT('Ctrl Pts',(-3.895686895944,-9.09188988950535,-9.61305631917377));
#44041=CARTESIAN_POINT('Ctrl Pts',(0.0001666015266142,-9.96180820070112,
-9.58947287128109));
#44042=CARTESIAN_POINT('Ctrl Pts',(3.896020098997,-9.09181548429369,-9.61305833630071));
#44043=CARTESIAN_POINT('Ctrl Pts',(5.844030148496,-8.22084239233718,-9.63752810198184));
#44044=CARTESIAN_POINT('Ctrl Pts',(-5.843530343916,-9.55783038259166,-11.8732201358514));
#44045=CARTESIAN_POINT('Ctrl Pts',(-3.895686895944,-10.2763900681484,-11.732826252669));
#44046=CARTESIAN_POINT('Ctrl Pts',(0.0001666015266142,-10.9955725683266,
-11.5921560888784));
#44047=CARTESIAN_POINT('Ctrl Pts',(3.896020098997,-10.2763285555545,-11.7328382843669));
#44048=CARTESIAN_POINT('Ctrl Pts',(5.844030148496,-9.55764599674235,-11.8732561615906));
#44049=CARTESIAN_POINT('Ctrl Pts',(-5.843530343916,-10.2973084082931,-14.4766646359851));
#44050=CARTESIAN_POINT('Ctrl Pts',(-3.895686895944,-10.9728038426106,-14.1582376099169));
#44051=CARTESIAN_POINT('Ctrl Pts',(0.0001666015266142,-11.6469750229257,
-13.8399443711029));
#44052=CARTESIAN_POINT('Ctrl Pts',(3.896020098997,-10.972746179898,-14.1582648339447));
#44053=CARTESIAN_POINT('Ctrl Pts',(5.844030148496,-10.2971350729153,-14.4767463458862));
#44054=CARTESIAN_POINT('Ctrl Pts',(-5.843530343916,-10.3258757623353,-16.2770693533102));
#44055=CARTESIAN_POINT('Ctrl Pts',(-3.895686895944,-11.0553896713365,-15.8346874642404));
#44056=CARTESIAN_POINT('Ctrl Pts',(0.0001666015266142,-11.7876699880132,
-15.3921227748421));
#44057=CARTESIAN_POINT('Ctrl Pts',(3.896020098997,-11.0553270384729,-15.8347253173623));
#44058=CARTESIAN_POINT('Ctrl Pts',(5.844030148496,-10.3256885656043,-16.2771828706193));
#44059=CARTESIAN_POINT('Ctrl Pts',(-5.843530343916,-10.225161154803,-17.1593148751532));
#44060=CARTESIAN_POINT('Ctrl Pts',(-3.895686895944,-11.003363098979,-16.6619434543588));
#44061=CARTESIAN_POINT('Ctrl Pts',(0.0001666015266142,-11.7816843621865,
-16.1645455971594));
#44062=CARTESIAN_POINT('Ctrl Pts',(3.896020098997,-11.0032965281671,-16.6619859974273));
#44063=CARTESIAN_POINT('Ctrl Pts',(5.844030148496,-10.2249614644564,-17.1594425030394));
#44064=CARTESIAN_POINT('Ctrl Pts',(-5.73278975501823,-6.65588713914762,
-8.10254235490726));
#44065=CARTESIAN_POINT('Ctrl Pts',(-5.37897179112506,-6.85202415254095,
-8.10465391657496));
#44066=CARTESIAN_POINT('Ctrl Pts',(-5.01613184499411,-7.0312284216845,-8.10373386681346));
#44067=CARTESIAN_POINT('Ctrl Pts',(-4.64588304903464,-7.19219343306865,
-8.10100473255839));
#44068=CARTESIAN_POINT('Ctrl Pts',(-4.37154851834488,-7.31145988670049,
-8.09898259022268));
#44069=CARTESIAN_POINT('Ctrl Pts',(-4.09314651694435,-7.42070943831706,
-8.09596903559524));
#44070=CARTESIAN_POINT('Ctrl Pts',(-3.81133323615115,-7.51943452553296,
-8.09247487047289));
#44071=CARTESIAN_POINT('Ctrl Pts',(-3.57225617964817,-7.6031882194261,-8.08951058607141));
#44072=CARTESIAN_POINT('Ctrl Pts',(-3.33072401753176,-7.67936667759463,
-8.0862006579435));
#44073=CARTESIAN_POINT('Ctrl Pts',(-3.08713739488102,-7.74770051014093,
-8.08285930770894));
#44074=CARTESIAN_POINT('Ctrl Pts',(-3.0435950629987,-7.7599155258226,-8.08226202457711));
#44075=CARTESIAN_POINT('Ctrl Pts',(-2.99998708420428,-7.77188001335109,
-8.08166373982413));
#44076=CARTESIAN_POINT('Ctrl Pts',(-2.95631574691158,-7.78359262272358,
-8.0810662505597));
#44077=CARTESIAN_POINT('Ctrl Pts',(-2.75788908834141,-7.83681045586082,
-8.07835147685176));
#44078=CARTESIAN_POINT('Ctrl Pts',(-2.55814961936489,-7.88487194894928,
-8.07569834222977));
#44079=CARTESIAN_POINT('Ctrl Pts',(-2.35736414035255,-7.92758001824303,
-8.07319712986884));
#44080=CARTESIAN_POINT('Ctrl Pts',(-2.16341814364899,-7.96883329565734,
-8.07078111788085));
#44081=CARTESIAN_POINT('Ctrl Pts',(-1.96849618498995,-8.00509159254689,
-8.06850686502789));
#44082=CARTESIAN_POINT('Ctrl Pts',(-1.7728387183633,-8.03622543206867,-8.06645526106578));
#44083=CARTESIAN_POINT('Ctrl Pts',(-1.58027048296615,-8.06686770011606,
-8.06443604983132));
#44084=CARTESIAN_POINT('Ctrl Pts',(-1.38698978208197,-8.09254589079393,
-8.06263252184692));
#44085=CARTESIAN_POINT('Ctrl Pts',(-1.19322585901438,-8.11318585606419,
-8.06112117401782));
#44086=CARTESIAN_POINT('Ctrl Pts',(-0.995042175532004,-8.13429661950999,
-8.05957535230316));
#44087=CARTESIAN_POINT('Ctrl Pts',(-0.796352973824406,-8.15013618939897,
-8.05833520502664));
#44088=CARTESIAN_POINT('Ctrl Pts',(-0.597403544878113,-8.16068270620361,
-8.05748174952326));
#44089=CARTESIAN_POINT('Ctrl Pts',(-0.408635679381983,-8.17068948770669,
-8.05667197100556));
#44090=CARTESIAN_POINT('Ctrl Pts',(-0.219633540211193,-8.17593135769825,
-8.05621031569765));
#44091=CARTESIAN_POINT('Ctrl Pts',(-0.030606653255842,-8.17644149281921,
-8.05616518408145));
#44092=CARTESIAN_POINT('Ctrl Pts',(-0.0204111189774602,-8.17646900795315,
-8.05616274981959));
#44093=CARTESIAN_POINT('Ctrl Pts',(-0.0102155127029499,-8.17648277019785,
-8.05616152710882));
#44094=CARTESIAN_POINT('Ctrl Pts',(-1.98673096702962E-5,-8.17648278911332,
-8.05616152661429));
#44095=CARTESIAN_POINT('Ctrl Pts',(-1.32448725733915E-5,-8.1764827891256,
-8.05616152661397));
#44096=CARTESIAN_POINT('Ctrl Pts',(-6.62243549213079E-6,-8.17648278913209,
-8.05616152661416));
#44097=CARTESIAN_POINT('Ctrl Pts',(1.57207580286922E-12,-8.17648278913278,
-8.05616152661487));
#44098=CARTESIAN_POINT('Ctrl Pts',(0.189380764722651,-8.17648280885812,
-8.05616154692102));
#44099=CARTESIAN_POINT('Ctrl Pts',(0.378748155853062,-8.17173673284014,
-8.05658332229546));
#44100=CARTESIAN_POINT('Ctrl Pts',(0.567891470777629,-8.16220840147887,
-8.05735811422046));
#44101=CARTESIAN_POINT('Ctrl Pts',(0.76929744390324,-8.15206232335369,-8.05818313794223));
#44102=CARTESIAN_POINT('Ctrl Pts',(0.970449344071629,-8.13649340887974,
-8.0594084403906));
#44103=CARTESIAN_POINT('Ctrl Pts',(1.17109277311662,-8.11552159247827,-8.06095004077886));
#44104=CARTESIAN_POINT('Ctrl Pts',(1.36687872490619,-8.09505749328269,-8.06245431979129));
#44105=CARTESIAN_POINT('Ctrl Pts',(1.5621805272216,-8.06944945144144,-8.0642597540552));
#44106=CARTESIAN_POINT('Ctrl Pts',(1.75676181475598,-8.03877216157455,-8.06628749697816));
#44107=CARTESIAN_POINT('Ctrl Pts',(1.95858448633675,-8.00695320983338,-8.06839070278574));
#44108=CARTESIAN_POINT('Ctrl Pts',(2.15963201702165,-7.96968067936552,-8.07073306287983));
#44109=CARTESIAN_POINT('Ctrl Pts',(2.35964065808733,-7.92709592124367,-8.07322586199765));
#44110=CARTESIAN_POINT('Ctrl Pts',(2.55964929915301,-7.88451116312181,-8.07571866111547));
#44111=CARTESIAN_POINT('Ctrl Pts',(2.75861905059947,-7.8366145558886,-8.078361884372));
#44112=CARTESIAN_POINT('Ctrl Pts',(2.95628616370335,-7.78360100621361,-8.08106628369463));
#44113=CARTESIAN_POINT('Ctrl Pts',(3.19882702103404,-7.71855249315338,-8.08438462694341));
#44114=CARTESIAN_POINT('Ctrl Pts',(3.43941382619942,-7.64573047320529,-8.08772747266317));
#44115=CARTESIAN_POINT('Ctrl Pts',(3.67765454918082,-7.56538919415433,-8.09078719554358));
#44116=CARTESIAN_POINT('Ctrl Pts',(3.96256884455284,-7.4693083116602,-8.09444634658038));
#44117=CARTESIAN_POINT('Ctrl Pts',(4.24412777542588,-7.36247414363688,-8.09770025029678));
#44118=CARTESIAN_POINT('Ctrl Pts',(4.52166081822969,-7.24539697669584,-8.10002600204554));
#44119=CARTESIAN_POINT('Ctrl Pts',(4.88863124915102,-7.09059069500283,-8.10310124711487));
#44120=CARTESIAN_POINT('Ctrl Pts',(5.2485629478173,-6.91788157640933,-8.10455102844123));
#44121=CARTESIAN_POINT('Ctrl Pts',(5.59990580189133,-6.72852560770424,-8.10319440285958));
#44122=CARTESIAN_POINT('Ctrl Pts',(5.64433782730844,-6.7045790008021,-8.10302283932377));
#44123=CARTESIAN_POINT('Ctrl Pts',(5.68863249132303,-6.68036614677505,-8.1028064622695));
#44124=CARTESIAN_POINT('Ctrl Pts',(5.7327866587865,-6.65588954538727,-8.10254295270174));
#44125=CARTESIAN_POINT('Ctrl Pts',(-5.84422295831999,-6.60976874991002,
-8.11490727298548));
#44126=CARTESIAN_POINT('Ctrl Pts',(-5.38938859865608,-6.87258866136879,
-8.12252792038973));
#44127=CARTESIAN_POINT('Ctrl Pts',(-4.35944142742656,-7.38493398830133,
-8.12651592016639));
#44128=CARTESIAN_POINT('Ctrl Pts',(-2.6946127460268,-7.93716129789442,-8.10974134360217));
#44129=CARTESIAN_POINT('Ctrl Pts',(-0.898320559210476,-8.22897502366934,
-8.09288659504273));
#44130=CARTESIAN_POINT('Ctrl Pts',(0.901429467966184,-8.22872398638616,
-8.09290350846181));
#44131=CARTESIAN_POINT('Ctrl Pts',(2.69770232818102,-7.93640182698235,-8.10977803300697));
#44132=CARTESIAN_POINT('Ctrl Pts',(4.36144900498123,-7.38403171477856,-8.12652349002812));
#44133=CARTESIAN_POINT('Ctrl Pts',(5.39040673669931,-6.87200650754738,-8.12251173095811));
#44134=CARTESIAN_POINT('Ctrl Pts',(5.84433195526982,-6.60970579078957,-8.11490540146884));
#44135=CARTESIAN_POINT('Ctrl Pts',(-5.72538011317797,-6.40695333589681,
-7.90742516593913));
#44136=CARTESIAN_POINT('Ctrl Pts',(-5.27970274304097,-6.66325795360347,
-7.91616927074093));
#44137=CARTESIAN_POINT('Ctrl Pts',(-4.27051957708516,-7.16304589521579,
-7.92255131832025));
#44138=CARTESIAN_POINT('Ctrl Pts',(-2.63947098547294,-7.70187917833143,
-7.90877350684347));
#44139=CARTESIAN_POINT('Ctrl Pts',(-0.879898351178121,-7.98663045155091,
-7.89367055524914));
#44140=CARTESIAN_POINT('Ctrl Pts',(0.882943541812166,-7.98638549093034,
-7.8936859086404));
#44141=CARTESIAN_POINT('Ctrl Pts',(2.64249762386501,-7.70113809089933,-7.90880579224764));
#44142=CARTESIAN_POINT('Ctrl Pts',(4.27248663614319,-7.16216559288129,-7.92255439312653));
#44143=CARTESIAN_POINT('Ctrl Pts',(5.28070038169628,-6.66269021335986,-7.91615058063814));
#44144=CARTESIAN_POINT('Ctrl Pts',(5.72548691629843,-6.40689193398313,-7.90742302702228));
#44145=CARTESIAN_POINT('Ctrl Pts',(-5.71943342809842,-6.40362121884893,
-7.5939596963265));
#44146=CARTESIAN_POINT('Ctrl Pts',(-5.27504920141105,-6.65726716852875,
-7.60270658234416));
#44147=CARTESIAN_POINT('Ctrl Pts',(-4.26853728029364,-7.15224503866711,
-7.60918179401112));
#44148=CARTESIAN_POINT('Ctrl Pts',(-2.63985305700298,-7.68689312320676,
-7.59558855876745));
#44149=CARTESIAN_POINT('Ctrl Pts',(-0.880379460818149,-7.96992923865942,
-7.58057647387013));
#44150=CARTESIAN_POINT('Ctrl Pts',(0.883425978655007,-7.96968558206291,
-7.58059176063567));
#44151=CARTESIAN_POINT('Ctrl Pts',(2.6428776046023,-7.68615698642532,-7.59562058355163));
#44152=CARTESIAN_POINT('Ctrl Pts',(4.2704995400594,-7.15137263723294,-7.60918461824791));
#44153=CARTESIAN_POINT('Ctrl Pts',(5.27604396018071,-6.65670529607616,-7.60268786578122));
#44154=CARTESIAN_POINT('Ctrl Pts',(5.71953991627837,-6.40356045813047,-7.59395755126392));
#44155=CARTESIAN_POINT('Ctrl Pts',(-5.83024166502501,-6.60193592346308,
-7.37785692368633));
#44156=CARTESIAN_POINT('Ctrl Pts',(-5.3784477878881,-6.85850456404399,-7.38548409954249));
#44157=CARTESIAN_POINT('Ctrl Pts',(-4.35478131953797,-7.35954007744269,
-7.38969113283958));
#44158=CARTESIAN_POINT('Ctrl Pts',(-2.69551165346364,-7.90192684740847,
-7.37335052155497));
#44159=CARTESIAN_POINT('Ctrl Pts',(-0.899451974758108,-8.18970778644358,
-7.35670941095802));
#44160=CARTESIAN_POINT('Ctrl Pts',(0.902564004795844,-8.18945981524842,
-7.35672616772986));
#44161=CARTESIAN_POINT('Ctrl Pts',(2.69859632014915,-7.90117901678993,-7.37338659820303));
#44162=CARTESIAN_POINT('Ctrl Pts',(4.35677761289836,-7.35865638110693,-7.38969811357579));
#44163=CARTESIAN_POINT('Ctrl Pts',(5.37945915464754,-6.85793620703642,-7.38546784792074));
#44164=CARTESIAN_POINT('Ctrl Pts',(5.83034992147577,-6.60187447197138,-7.37785503772092));
#44165=CARTESIAN_POINT('Ctrl Pts',(-5.7200175232721,-6.64700781289157,-7.39409107725312));
#44166=CARTESIAN_POINT('Ctrl Pts',(-5.51371324185327,-6.76166932142692,
-7.39720426684975));
#44167=CARTESIAN_POINT('Ctrl Pts',(-5.30244990809323,-6.87155186606564,
-7.39917723806279));
#44168=CARTESIAN_POINT('Ctrl Pts',(-5.08630387814312,-6.97606931525954,
-7.40024850210269));
#44169=CARTESIAN_POINT('Ctrl Pts',(-4.87015784819301,-7.08058676445345,
-7.40131976614259));
#44170=CARTESIAN_POINT('Ctrl Pts',(-4.64912885670142,-7.17973930199014,
-7.40148918223241));
#44171=CARTESIAN_POINT('Ctrl Pts',(-4.4233223550221,-7.27289273489692,-7.40101846283964));
#44172=CARTESIAN_POINT('Ctrl Pts',(-4.41102142472513,-7.27796731812011,
-7.40099282014823));
#44173=CARTESIAN_POINT('Ctrl Pts',(-4.39870632454384,-7.28302408624263,
-7.40096528384693));
#44174=CARTESIAN_POINT('Ctrl Pts',(-4.38637708600296,-7.28806293330809,
-7.40093589965471));
#44175=CARTESIAN_POINT('Ctrl Pts',(-4.17423011394607,-7.37476546112847,
-7.400430291187));
#44176=CARTESIAN_POINT('Ctrl Pts',(-3.95789714003301,-7.45617951152167,
-7.39936226650764));
#44177=CARTESIAN_POINT('Ctrl Pts',(-3.73752760079179,-7.53183568206427,
-7.39788683592457));
#44178=CARTESIAN_POINT('Ctrl Pts',(-3.71639529957566,-7.53909071826515,
-7.39774534974816));
#44179=CARTESIAN_POINT('Ctrl Pts',(-3.69522588741974,-7.54629276995919,
-7.39760013151133));
#44180=CARTESIAN_POINT('Ctrl Pts',(-3.67401950167808,-7.55344139995593,
-7.39745132725152));
#44181=CARTESIAN_POINT('Ctrl Pts',(-3.55284525913626,-7.59428899348834,
-7.39660105301393));
#44182=CARTESIAN_POINT('Ctrl Pts',(-3.43046441960889,-7.63339399527552,
-7.39563199523097));
#44183=CARTESIAN_POINT('Ctrl Pts',(-3.30690773257217,-7.67068044224599,
-7.39456257166012));
#44184=CARTESIAN_POINT('Ctrl Pts',(-3.24512938905381,-7.68932366573122,
-7.3940278598747));
#44185=CARTESIAN_POINT('Ctrl Pts',(-3.18305707852317,-7.70751223189553,
-7.39346803903621));
#44186=CARTESIAN_POINT('Ctrl Pts',(-3.12069513729051,-7.72523682409344,
-7.39288485977133));
#44187=CARTESIAN_POINT('Ctrl Pts',(-3.08951416667418,-7.73409912019239,
-7.39259327013889));
#44188=CARTESIAN_POINT('Ctrl Pts',(-3.05826078818309,-7.74284542176459,
-7.39229583995104));
#44189=CARTESIAN_POINT('Ctrl Pts',(-3.02693555934582,-7.75147456866553,
-7.39199276680285));
#44190=CARTESIAN_POINT('Ctrl Pts',(-3.0038616182549,-7.75783073698889,-7.3917695252743));
#44191=CARTESIAN_POINT('Ctrl Pts',(-2.97980770982277,-7.76437813570979,
-7.39153386934831));
#44192=CARTESIAN_POINT('Ctrl Pts',(-2.95685308918717,-7.77055206877725,
-7.39130652327029));
#44193=CARTESIAN_POINT('Ctrl Pts',(-2.94864447067566,-7.77275987966077,
-7.39122522385549));
#44194=CARTESIAN_POINT('Ctrl Pts',(-2.94057656484299,-7.77492041245755,
-7.39114499476737));
#44195=CARTESIAN_POINT('Ctrl Pts',(-2.93274488786755,-7.77700938676643,
-7.39106680435592));
#44196=CARTESIAN_POINT('Ctrl Pts',(-2.84286196192221,-7.80098421663956,
-7.3901694252909));
#44197=CARTESIAN_POINT('Ctrl Pts',(-2.75267957579997,-7.82388471216904,
-7.38926607338874));
#44198=CARTESIAN_POINT('Ctrl Pts',(-2.66221234566274,-7.84569650678844,
-7.38837077971031));
#44199=CARTESIAN_POINT('Ctrl Pts',(-2.40391363455117,-7.9079727412733,-7.38581457009881));
#44200=CARTESIAN_POINT('Ctrl Pts',(-2.14329376638944,-7.96137761868093,
-7.38332392021102));
#44201=CARTESIAN_POINT('Ctrl Pts',(-1.88082100481702,-8.00567783504727,
-7.38110967219702));
#44202=CARTESIAN_POINT('Ctrl Pts',(-1.62315194251182,-8.04916728188605,
-7.37893594869877));
#44203=CARTESIAN_POINT('Ctrl Pts',(-1.36369666562235,-8.08388241259931,
-7.37702839999861));
#44204=CARTESIAN_POINT('Ctrl Pts',(-1.10289072817735,-8.10955302367032,
-7.37558982376376));
#44205=CARTESIAN_POINT('Ctrl Pts',(-1.0302688443648,-8.11670105163647,-7.37518924961577));
#44206=CARTESIAN_POINT('Ctrl Pts',(-0.957542217175731,-8.12314750265828,
-7.374825067595));
#44207=CARTESIAN_POINT('Ctrl Pts',(-0.884720229343273,-8.12888581949315,
-7.37450173617424));
#44208=CARTESIAN_POINT('Ctrl Pts',(-0.621866153454331,-8.14959851923789,
-7.37333465759893));
#44209=CARTESIAN_POINT('Ctrl Pts',(-0.357769019522488,-8.16108897896362,
-7.37269961871155));
#44210=CARTESIAN_POINT('Ctrl Pts',(-0.0929439746577478,-8.16327002316267,
-7.37257848004112));
#44211=CARTESIAN_POINT('Ctrl Pts',(-0.0619677561530355,-8.16352513688015,
-7.37256431061872));
#44212=CARTESIAN_POINT('Ctrl Pts',(-0.0309815892461447,-8.16365282469521,
-7.37255717553758));
#44213=CARTESIAN_POINT('Ctrl Pts',(1.36919838106928E-5,-8.16365290107928,
-7.37255704847296));
#44214=CARTESIAN_POINT('Ctrl Pts',(0.260481133587845,-8.1636535429694,-7.3725559806912));
#44215=CARTESIAN_POINT('Ctrl Pts',(0.520290709605892,-8.15466266469011,
-7.37303196871935));
#44216=CARTESIAN_POINT('Ctrl Pts',(0.778967847162538,-8.13675976149421,
-7.37401334251466));
#44217=CARTESIAN_POINT('Ctrl Pts',(0.815264655427029,-8.1342476792483,-7.37415104597319));
#44218=CARTESIAN_POINT('Ctrl Pts',(0.851539175291451,-8.13156004608175,
-7.37429870473853));
#44219=CARTESIAN_POINT('Ctrl Pts',(0.887790101292666,-8.12869700051921,
-7.37445640166713));
#44220=CARTESIAN_POINT('Ctrl Pts',(1.08697684364434,-8.11296552047956,-7.37532289367028));
#44221=CARTESIAN_POINT('Ctrl Pts',(1.28545136831308,-8.09193964782705,-7.37649227436005));
#44222=CARTESIAN_POINT('Ctrl Pts',(1.48302725142221,-8.06574169304764,-7.37787936089373));
#44223=CARTESIAN_POINT('Ctrl Pts',(1.72792448366118,-8.03326907283289,-7.37959866816763));
#44224=CARTESIAN_POINT('Ctrl Pts',(1.97142847485369,-7.99282198952477,-7.38168606335154));
#44225=CARTESIAN_POINT('Ctrl Pts',(2.21317518510619,-7.94461687274513,-7.38396070087494));
#44226=CARTESIAN_POINT('Ctrl Pts',(2.33404854023243,-7.92051431435531,-7.38509801963663));
#44227=CARTESIAN_POINT('Ctrl Pts',(2.45448288511245,-7.89447302683783,-7.38628058810975));
#44228=CARTESIAN_POINT('Ctrl Pts',(2.5744345461666,-7.86652469780926,-7.38747652781115));
#44229=CARTESIAN_POINT('Ctrl Pts',(2.60474934218281,-7.85946145344858,-7.38777877179658));
#44230=CARTESIAN_POINT('Ctrl Pts',(2.6350333592709,-7.85227644061828,-7.38808180844263));
#44231=CARTESIAN_POINT('Ctrl Pts',(2.66528580642343,-7.84497013890992,-7.38838515239865));
#44232=CARTESIAN_POINT('Ctrl Pts',(2.694885836671,-7.83782140312418,-7.38868195451282));
#44233=CARTESIAN_POINT('Ctrl Pts',(2.72445564398435,-7.83055655339874,-7.3889790508266));
#44234=CARTESIAN_POINT('Ctrl Pts',(2.75399469624353,-7.82317623364713,-7.38927581213863));
#44235=CARTESIAN_POINT('Ctrl Pts',(2.78385928494455,-7.81571457875279,-7.38957584392192));
#44236=CARTESIAN_POINT('Ctrl Pts',(2.81369238495066,-7.80813485455885,-7.38987558891595));
#44237=CARTESIAN_POINT('Ctrl Pts',(2.8434933475593,-7.80043765701813,-7.3901744906164));
#44238=CARTESIAN_POINT('Ctrl Pts',(2.86560649665769,-7.79472612081399,-7.39039628405156));
#44239=CARTESIAN_POINT('Ctrl Pts',(2.88674831666762,-7.78920060926862,-7.39060806890174));
#44240=CARTESIAN_POINT('Ctrl Pts',(2.90904172325111,-7.7833043905423,-7.39083087286923));
#44241=CARTESIAN_POINT('Ctrl Pts',(2.91679220472072,-7.78125452284676,-7.3909083324542));
#44242=CARTESIAN_POINT('Ctrl Pts',(2.92468175519996,-7.77915941817535,-7.39098711927652));
#44243=CARTESIAN_POINT('Ctrl Pts',(2.93279917759592,-7.77699424572049,-7.391068097953));
#44244=CARTESIAN_POINT('Ctrl Pts',(3.15805061537049,-7.71691258621102,-7.39331518605765));
#44245=CARTESIAN_POINT('Ctrl Pts',(3.37963538387188,-7.65068123739186,-7.39538046713975));
#44246=CARTESIAN_POINT('Ctrl Pts',(3.59738192019367,-7.57882478942696,-7.39706852248287));
#44247=CARTESIAN_POINT('Ctrl Pts',(3.82052223618586,-7.5051883919172,-7.39879839249155));
#44248=CARTESIAN_POINT('Ctrl Pts',(4.03963186912597,-7.42564470520827,-7.40013221739745));
#44249=CARTESIAN_POINT('Ctrl Pts',(4.25454557778461,-7.34071227879178,-7.40088182818385));
#44250=CARTESIAN_POINT('Ctrl Pts',(4.31206231045888,-7.31798205978405,-7.401082444345));
#44251=CARTESIAN_POINT('Ctrl Pts',(4.36927861548813,-7.29486562978467,-7.40124133192306));
#44252=CARTESIAN_POINT('Ctrl Pts',(4.42619154442692,-7.27137239769755,-7.40135512978351));
#44253=CARTESIAN_POINT('Ctrl Pts',(4.65147047778588,-7.17837893620424,-7.40180557682775));
#44254=CARTESIAN_POINT('Ctrl Pts',(4.8719950275897,-7.07948568452959,-7.40154785261369));
#44255=CARTESIAN_POINT('Ctrl Pts',(5.08766384430848,-6.97524835766162,-7.40039572003413));
#44256=CARTESIAN_POINT('Ctrl Pts',(5.30333266102726,-6.87101103079365,-7.39924358745457));
#44257=CARTESIAN_POINT('Ctrl Pts',(5.51414587167326,-6.76142934734901,-7.39719722479767));
#44258=CARTESIAN_POINT('Ctrl Pts',(5.72001467857883,-6.64700991222121,-7.39409062851839));
#44259=CARTESIAN_POINT('Ctrl Pts',(6.05066939030811,-10.3127953565056,-1.22617515269708));
#44260=CARTESIAN_POINT('Ctrl Pts',(6.05130921732087,-10.3094309468474,-1.25222015897757));
#44261=CARTESIAN_POINT('Ctrl Pts',(6.04716617417261,-10.3028567867706,-1.31997136664705));
#44262=CARTESIAN_POINT('Ctrl Pts',(6.01576910230258,-10.3008720417499,-1.43277663512264));
#44263=CARTESIAN_POINT('Ctrl Pts',(5.94717377016299,-10.3112693333796,-1.55348066131538));
#44264=CARTESIAN_POINT('Ctrl Pts',(5.84901708021604,-10.334275868274,-1.65610810365757));
#44265=CARTESIAN_POINT('Ctrl Pts',(5.76450435111265,-10.3583100007465,-1.70838528469582));
#44266=CARTESIAN_POINT('Ctrl Pts',(5.71748516972109,-10.37274644705,-1.72859734565015));
#44267=CARTESIAN_POINT('Ctrl Pts',(5.71213042723896,-10.3744035443872,-1.73079093733939));
#44268=CARTESIAN_POINT('Ctrl Pts',(5.91207393029035,-10.0311964577302,-1.19349828764901));
#44269=CARTESIAN_POINT('Ctrl Pts',(5.91266157430069,-10.0281594687441,-1.21694391136227));
#44270=CARTESIAN_POINT('Ctrl Pts',(5.90886049650901,-10.0222648764306,-1.27818392833765));
#44271=CARTESIAN_POINT('Ctrl Pts',(5.87975076332791,-10.0208075082426,-1.38101232835033));
#44272=CARTESIAN_POINT('Ctrl Pts',(5.81578180589495,-10.0310304108616,-1.49171175501008));
#44273=CARTESIAN_POINT('Ctrl Pts',(5.72402711176062,-10.0530519067873,-1.58611209758615));
#44274=CARTESIAN_POINT('Ctrl Pts',(5.64503109213434,-10.0757988066388,-1.6342245583265));
#44275=CARTESIAN_POINT('Ctrl Pts',(5.60113930969898,-10.089381109962,-1.65281889954393));
#44276=CARTESIAN_POINT('Ctrl Pts',(5.59614154922131,-10.0909391882732,-1.65483685123968));
#44277=CARTESIAN_POINT('Ctrl Pts',(6.02856620736513,-9.74070678474308,-1.15324175165922));
#44278=CARTESIAN_POINT('Ctrl Pts',(6.02948707486004,-9.73604662848835,-1.18936361391473));
#44279=CARTESIAN_POINT('Ctrl Pts',(6.02349351115603,-9.72707553668167,-1.28184356126626));
#44280=CARTESIAN_POINT('Ctrl Pts',(5.98036953308613,-9.72431468556907,-1.43080025677482));
#44281=CARTESIAN_POINT('Ctrl Pts',(5.88895461810126,-9.7375088295263,-1.58654545187936));
#44282=CARTESIAN_POINT('Ctrl Pts',(5.75979132356852,-9.76686971121646,-1.71781231137828));
#44283=CARTESIAN_POINT('Ctrl Pts',(5.64854720753488,-9.79791761496062,-1.78497284675799));
#44284=CARTESIAN_POINT('Ctrl Pts',(5.58621679756139,-9.81682449515364,-1.81115576311391));
#44285=CARTESIAN_POINT('Ctrl Pts',(5.57911215103403,-9.81899805900445,-1.81400075163189));
#44286=CARTESIAN_POINT('Ctrl Pts',(6.32386216337528,-9.63155076077824,-1.13176716249797));
#44287=CARTESIAN_POINT('Ctrl Pts',(6.32528345230293,-9.62437976652278,-1.18753995793898));
#44288=CARTESIAN_POINT('Ctrl Pts',(6.31599868199734,-9.61059072740038,-1.32855375525905));
#44289=CARTESIAN_POINT('Ctrl Pts',(6.25173598350599,-9.60554910845383,-1.54953718978642));
#44290=CARTESIAN_POINT('Ctrl Pts',(6.11877552868139,-9.62291443242936,-1.77588068427804));
#44291=CARTESIAN_POINT('Ctrl Pts',(5.93288973882408,-9.66313299096965,-1.9649659533792));
#44292=CARTESIAN_POINT('Ctrl Pts',(5.77275010998209,-9.70663429398153,-2.0619138892666));
#44293=CARTESIAN_POINT('Ctrl Pts',(5.6824894231339,-9.73355771741979,-2.09992236202094));
#44294=CARTESIAN_POINT('Ctrl Pts',(5.67219369876869,-9.73665822595086,-2.10405548617845));
#44295=CARTESIAN_POINT('',(5.73278505653102,-10.3449524964723,-1.71289224212846));
#44296=CARTESIAN_POINT('',(5.72001587123307,-9.72697769588761,-2.0594345452005));
#44297=CARTESIAN_POINT('Origin',(5.89875825683544,-10.1838012062076,-2.15614435592649));
#44298=CARTESIAN_POINT('',(5.99999998667943,-9.65438790406946,-1.86247695099856));
#44299=CARTESIAN_POINT('Ctrl Pts',(6.00000003796097,-9.65438809185475,-1.86247698722521));
#44300=CARTESIAN_POINT('Ctrl Pts',(5.95882273790821,-9.66348805825028,-1.90324205679966));
#44301=CARTESIAN_POINT('Ctrl Pts',(5.91487788445314,-9.67407471952828,-1.93999595034449));
#44302=CARTESIAN_POINT('Ctrl Pts',(5.86822767748739,-9.68615017643769,-1.97285849162915));
#44303=CARTESIAN_POINT('Ctrl Pts',(5.82157747052231,-9.69822563334693,-2.00572103291333));
#44304=CARTESIAN_POINT('Ctrl Pts',(5.77222173582301,-9.71178946761864,-2.03469214155817));
#44305=CARTESIAN_POINT('Ctrl Pts',(5.72001606109556,-9.72697818111165,-2.0594346479375));
#44306=CARTESIAN_POINT('',(5.99998684676694,-10.0933419068472,-1.2110347738228));
#44307=CARTESIAN_POINT('Ctrl Pts',(5.99998684676694,-10.0933419068472,-1.2110347738228));
#44308=CARTESIAN_POINT('Ctrl Pts',(5.99998481317996,-10.0709318263906,-1.22812637108207));
#44309=CARTESIAN_POINT('Ctrl Pts',(5.99998609830006,-10.0492937981165,-1.2455430819064));
#44310=CARTESIAN_POINT('Ctrl Pts',(5.99998227627453,-10.0284575477685,-1.26330025491489));
#44311=CARTESIAN_POINT('Ctrl Pts',(5.99998116448161,-10.0223964695217,-1.26846565719452));
#44312=CARTESIAN_POINT('Ctrl Pts',(5.99997943623455,-10.0164030435298,-1.27365962773701));
#44313=CARTESIAN_POINT('Ctrl Pts',(5.99997660921889,-10.0104775368722,-1.27888202729153));
#44314=CARTESIAN_POINT('Ctrl Pts',(5.99996297131451,-9.98189209455754,-1.30407558622867));
#44315=CARTESIAN_POINT('Ctrl Pts',(5.99992758485034,-9.954890878723,-1.32993076951105));
#44316=CARTESIAN_POINT('Ctrl Pts',(5.99991487015089,-9.92942364904202,-1.35643845475696));
#44317=CARTESIAN_POINT('Ctrl Pts',(5.99991410384967,-9.92788876656782,-1.35803604436625));
#44318=CARTESIAN_POINT('Ctrl Pts',(5.99991341291059,-9.92635944489813,-1.35963600871984));
#44319=CARTESIAN_POINT('Ctrl Pts',(5.99991280551292,-9.92483566959625,-1.36123834883611));
#44320=CARTESIAN_POINT('Ctrl Pts',(5.99990375315627,-9.90212607069442,-1.38511883915503));
#44321=CARTESIAN_POINT('Ctrl Pts',(5.99990215490928,-9.88067245865394,-1.40953845039357));
#44322=CARTESIAN_POINT('Ctrl Pts',(5.99990391521304,-9.86048117020938,-1.43448402417505));
#44323=CARTESIAN_POINT('Ctrl Pts',(5.99990506541729,-9.84728793261089,-1.45078377061438));
#44324=CARTESIAN_POINT('Ctrl Pts',(5.99990801397928,-9.83463312599759,-1.46730846004701));
#44325=CARTESIAN_POINT('Ctrl Pts',(5.99991561449138,-9.82251772060994,-1.48406637309734));
#44326=CARTESIAN_POINT('Ctrl Pts',(5.99991855526553,-9.81783005346036,-1.49055030953925));
#44327=CARTESIAN_POINT('Ctrl Pts',(5.99992663423283,-9.81306236424672,-1.49728724114274));
#44328=CARTESIAN_POINT('Ctrl Pts',(5.99993199795079,-9.80844193835796,-1.50398256147571));
#44329=CARTESIAN_POINT('Ctrl Pts',(5.99993742991546,-9.80376272322492,-1.51076307153622));
#44330=CARTESIAN_POINT('Ctrl Pts',(5.99993980443271,-9.79923474176042,-1.5175006375891));
#44331=CARTESIAN_POINT('Ctrl Pts',(5.99994481678224,-9.79505843631892,-1.52385025354702));
#44332=CARTESIAN_POINT('Ctrl Pts',(5.99994564462708,-9.79436867338557,-1.5248989626968));
#44333=CARTESIAN_POINT('Ctrl Pts',(5.99994657878526,-9.79368842452149,-1.52593701198677));
#44334=CARTESIAN_POINT('Ctrl Pts',(5.99994768557723,-9.79301850146117,-1.52696276047398));
#44335=CARTESIAN_POINT('Ctrl Pts',(5.99997440659629,-9.77684470615519,-1.55172716559746));
#44336=CARTESIAN_POINT('Ctrl Pts',(5.99996041292407,-9.76199870702985,-1.57678838130543));
#44337=CARTESIAN_POINT('Ctrl Pts',(5.99993581405304,-9.74841451382906,-1.60209969757037));
#44338=CARTESIAN_POINT('Ctrl Pts',(5.9999133458294,-9.73600692445224,-1.62521865753805));
#44339=CARTESIAN_POINT('Ctrl Pts',(5.99988325061035,-9.72465152383613,-1.64854730625723));
#44340=CARTESIAN_POINT('Ctrl Pts',(5.99986690142854,-9.71432348654574,-1.67207885292539));
#44341=CARTESIAN_POINT('Ctrl Pts',(5.9998499952577,-9.70364359045972,-1.6964120796647));
#44342=CARTESIAN_POINT('Ctrl Pts',(5.99984921018281,-9.6940616097742,-1.72096348561248));
#44343=CARTESIAN_POINT('Ctrl Pts',(5.99986989539589,-9.6855862564238,-1.7457479612625));
#44344=CARTESIAN_POINT('Ctrl Pts',(5.99988995086758,-9.6773689270412,-1.76977789742815));
#44345=CARTESIAN_POINT('Ctrl Pts',(5.99993074885979,-9.67019227989532,-1.79402798208124));
#44346=CARTESIAN_POINT('Ctrl Pts',(5.99996386685918,-9.66409962585232,-1.81851012398838));
#44347=CARTESIAN_POINT('Ctrl Pts',(5.99998358101823,-9.66047285029037,-1.833083614186));
#44348=CARTESIAN_POINT('Ctrl Pts',(5.99999988542516,-9.65723085510648,-1.84773922258285));
#44349=CARTESIAN_POINT('Ctrl Pts',(5.9999998883105,-9.65438772860653,-1.86247691714912));
#44350=CARTESIAN_POINT('Ctrl Pts',(5.99998684676694,-10.0933419068472,-1.2110347738228));
#44351=CARTESIAN_POINT('Ctrl Pts',(5.99998426938999,-10.0961503515468,-1.22746145677463));
#44352=CARTESIAN_POINT('Ctrl Pts',(5.99923948339792,-10.0995808523923,-1.24481847430359));
#44353=CARTESIAN_POINT('Ctrl Pts',(5.99754684899445,-10.1037210615654,-1.26300200081039));
#44354=CARTESIAN_POINT('Ctrl Pts',(5.9968763249387,-10.1053611734765,-1.27020526450167));
#44355=CARTESIAN_POINT('Ctrl Pts',(5.99605684860915,-10.107112741282,-1.27753773151475));
#44356=CARTESIAN_POINT('Ctrl Pts',(5.99507466942231,-10.1089815685309,-1.28499086684201));
#44357=CARTESIAN_POINT('Ctrl Pts',(5.99262347430917,-10.1136455445967,-1.30359143294694));
#44358=CARTESIAN_POINT('Ctrl Pts',(5.98915863196479,-10.119039980799,-1.32294760085419));
#44359=CARTESIAN_POINT('Ctrl Pts',(5.98451505832419,-10.1252388252198,-1.34289325113992));
#44360=CARTESIAN_POINT('Ctrl Pts',(5.98028205895253,-10.1308895818501,-1.36107535218136));
#44361=CARTESIAN_POINT('Ctrl Pts',(5.97506991267794,-10.1372086565094,-1.379747387453));
#44362=CARTESIAN_POINT('Ctrl Pts',(5.96874928910461,-10.144252797769,-1.3987369167749));
#44363=CARTESIAN_POINT('Ctrl Pts',(5.96715206381112,-10.1460328564073,-1.40353558200036));
#44364=CARTESIAN_POINT('Ctrl Pts',(5.96548401521494,-10.147859224561,-1.4083542693434));
#44365=CARTESIAN_POINT('Ctrl Pts',(5.96374296268477,-10.1497328399762,-1.41318965844888));
#44366=CARTESIAN_POINT('Ctrl Pts',(5.96325809545566,-10.1502546247581,-1.41453627015452));
#44367=CARTESIAN_POINT('Ctrl Pts',(5.9627675659131,-10.1507800739942,-1.41588417576981));
#44368=CARTESIAN_POINT('Ctrl Pts',(5.96227134381333,-10.1513092015444,-1.4172333118891));
#44369=CARTESIAN_POINT('Ctrl Pts',(5.95760675368347,-10.1562831096983,-1.42991546979536));
#44370=CARTESIAN_POINT('Ctrl Pts',(5.9524390259647,-10.1615821167091,-1.44270716308485));
#44371=CARTESIAN_POINT('Ctrl Pts',(5.94674392266645,-10.1672172490246,-1.45555037537036));
#44372=CARTESIAN_POINT('Ctrl Pts',(5.94389637101732,-10.1700348151824,-1.46197198151312));
#44373=CARTESIAN_POINT('Ctrl Pts',(5.94091693215639,-10.1729364220193,-1.46840644352367));
#44374=CARTESIAN_POINT('Ctrl Pts',(5.93780276751921,-10.1759233538012,-1.47484536375715));
#44375=CARTESIAN_POINT('Ctrl Pts',(5.93624568520062,-10.1774168196921,-1.47806482387389));
#44376=CARTESIAN_POINT('Ctrl Pts',(5.93465491803602,-10.1789316175185,-1.48128539676445));
#44377=CARTESIAN_POINT('Ctrl Pts',(5.93303010738351,-10.1804679076617,-1.4845059837072));
#44378=CARTESIAN_POINT('Ctrl Pts',(5.93196067779295,-10.1814790741852,-1.48662573284243));
#44379=CARTESIAN_POINT('Ctrl Pts',(5.93060067674035,-10.1827593132383,-1.48928202609314));
#44380=CARTESIAN_POINT('Ctrl Pts',(5.92949260106467,-10.1837965823635,-1.4914137818749));
#44381=CARTESIAN_POINT('Ctrl Pts',(5.9289171501412,-10.1843352617056,-1.49252085502897));
#44382=CARTESIAN_POINT('Ctrl Pts',(5.92841059870599,-10.1848080231713,-1.4934870775402));
#44383=CARTESIAN_POINT('Ctrl Pts',(5.92805317832642,-10.1851414168011,-1.49416665862601));
#44384=CARTESIAN_POINT('Ctrl Pts',(5.92203018796046,-10.1907595257142,-1.50561846878198));
#44385=CARTESIAN_POINT('Ctrl Pts',(5.91521672355695,-10.19699388167,-1.51774083623431));
#44386=CARTESIAN_POINT('Ctrl Pts',(5.90747417723844,-10.2039017430124,-1.53037783789015));
#44387=CARTESIAN_POINT('Ctrl Pts',(5.90656459425261,-10.2047132684314,-1.53186241431051));
#44388=CARTESIAN_POINT('Ctrl Pts',(5.90564218022057,-10.2055340931858,-1.5333540344392));
#44389=CARTESIAN_POINT('Ctrl Pts',(5.90470670386827,-10.2063643133579,-1.53485239646646));
#44390=CARTESIAN_POINT('Ctrl Pts',(5.89691024349106,-10.2132835461743,-1.54734006667594));
#44391=CARTESIAN_POINT('Ctrl Pts',(5.88820589338057,-10.2208555536035,-1.56029993766635));
#44392=CARTESIAN_POINT('Ctrl Pts',(5.87847600952666,-10.229129372186,-1.57354685685025));
#44393=CARTESIAN_POINT('Ctrl Pts',(5.8695253575908,-10.2367405699583,-1.58573287721985));
#44394=CARTESIAN_POINT('Ctrl Pts',(5.85970668664249,-10.2449456918696,-1.59816197806437));
#44395=CARTESIAN_POINT('Ctrl Pts',(5.84893607357442,-10.2537808325076,-1.61064804237114));
#44396=CARTESIAN_POINT('Ctrl Pts',(5.84055528470297,-10.2606555988621,-1.62036365169894));
#44397=CARTESIAN_POINT('Ctrl Pts',(5.83159823346717,-10.2679117770402,-1.63011310189377));
#44398=CARTESIAN_POINT('Ctrl Pts',(5.82203000190611,-10.2755653475831,-1.63978717038512));
#44399=CARTESIAN_POINT('Ctrl Pts',(5.81023610680679,-10.2849992129262,-1.65171152111205));
#44400=CARTESIAN_POINT('Ctrl Pts',(5.7975122424402,-10.2950373199467,-1.66352224698458));
#44401=CARTESIAN_POINT('Ctrl Pts',(5.78382720703097,-10.3056961993029,-1.67500097984752));
#44402=CARTESIAN_POINT('Ctrl Pts',(5.77101414445683,-10.3156759241686,-1.68574831940832));
#44403=CARTESIAN_POINT('Ctrl Pts',(5.75735837270392,-10.3261997944818,-1.6962048619838));
#44404=CARTESIAN_POINT('Ctrl Pts',(5.74285647658939,-10.3372754895292,-1.70615098188076));
#44405=CARTESIAN_POINT('Ctrl Pts',(5.73954258787944,-10.3398064427564,-1.7084238111835));
#44406=CARTESIAN_POINT('Ctrl Pts',(5.73618461711692,-10.3423661872688,-1.71066980157742));
#44407=CARTESIAN_POINT('Ctrl Pts',(5.73278271249385,-10.3449547711923,-1.7128859870255));
#44408=CARTESIAN_POINT('Ctrl Pts',(5.99928507441619,-19.6591035773105,-0.0581387038097093));
#44409=CARTESIAN_POINT('Ctrl Pts',(5.99928507441619,-19.6322147488868,-0.0775484860915536));
#44410=CARTESIAN_POINT('Ctrl Pts',(5.99928507441619,-19.2058449769004,-0.38207282190903));
#44411=CARTESIAN_POINT('Ctrl Pts',(5.99928507441619,-18.3334658087218,-0.906210204715289));
#44412=CARTESIAN_POINT('Ctrl Pts',(5.99928507441619,-16.9710147391481,-1.46998745478167));
#44413=CARTESIAN_POINT('Ctrl Pts',(5.99928507441619,-15.5398213819416,-1.82605993958607));
#44414=CARTESIAN_POINT('Ctrl Pts',(5.99928507441619,-14.0709556091875,-1.9661845044543));
#44415=CARTESIAN_POINT('Ctrl Pts',(5.99928507441619,-12.5966799711141,-1.88736698540332));
#44416=CARTESIAN_POINT('Ctrl Pts',(5.99928507441619,-11.2335282355129,-1.60731118852257));
#44417=CARTESIAN_POINT('Ctrl Pts',(5.99928507441619,-10.3852024002489,-1.308971212486));
#44418=CARTESIAN_POINT('Ctrl Pts',(5.99928507441619,-10.0105704181296,-1.15061620805415));
#44419=CARTESIAN_POINT('Ctrl Pts',(6.0106662077061,-19.7703827345453,-0.212268579484425));
#44420=CARTESIAN_POINT('Ctrl Pts',(6.0106662077061,-19.7429754823504,-0.232052356751892));
#44421=CARTESIAN_POINT('Ctrl Pts',(6.0106662077061,-19.308392033223,-0.542440795747545));
#44422=CARTESIAN_POINT('Ctrl Pts',(6.0106662077061,-18.4193939491244,-1.0765722015714));
#44423=CARTESIAN_POINT('Ctrl Pts',(6.0106662077061,-17.0306058173753,-1.65124564686108));
#44424=CARTESIAN_POINT('Ctrl Pts',(6.0106662077061,-15.5720774343996,-2.01411525356481));
#44425=CARTESIAN_POINT('Ctrl Pts',(6.0106662077061,-14.0748737875543,-2.15695124058169));
#44426=CARTESIAN_POINT('Ctrl Pts',(6.0106662077061,-12.5723725487962,-2.07661671511421));
#44427=CARTESIAN_POINT('Ctrl Pts',(6.0106662077061,-11.1829429890494,-1.79116790615583));
#44428=CARTESIAN_POINT('Ctrl Pts',(6.0106662077061,-10.3184089964746,-1.48712752681436));
#44429=CARTESIAN_POINT('Ctrl Pts',(6.0106662077061,-9.93655135940431,-1.32571656146796));
#44430=CARTESIAN_POINT('Ctrl Pts',(5.90294096085745,-19.862565198381,-0.339948120237213));
#44431=CARTESIAN_POINT('Ctrl Pts',(5.90294096085745,-19.8347284894849,-0.360041710955224));
#44432=CARTESIAN_POINT('Ctrl Pts',(5.90294096085745,-19.3933409180546,-0.675287910315859));
#44433=CARTESIAN_POINT('Ctrl Pts',(5.90294096085745,-18.4905759017301,-1.21769825793309));
#44434=CARTESIAN_POINT('Ctrl Pts',(5.90294096085745,-17.0799704293154,-1.80139799481888));
#44435=CARTESIAN_POINT('Ctrl Pts',(5.90294096085745,-15.5987980033129,-2.1698982646174));
#44436=CARTESIAN_POINT('Ctrl Pts',(5.90294096085745,-14.0781195646156,-2.31498036474823));
#44437=CARTESIAN_POINT('Ctrl Pts',(5.90294096085745,-12.5522365400888,-2.23338916738684));
#44438=CARTESIAN_POINT('Ctrl Pts',(5.90294096085745,-11.1410387118318,-1.94347284489393));
#44439=CARTESIAN_POINT('Ctrl Pts',(5.90294096085745,-10.2630780550711,-1.63471031241584));
#44440=CARTESIAN_POINT('Ctrl Pts',(5.90294096085745,-9.87523476270989,-1.47076782172808));
#44441=CARTESIAN_POINT('Ctrl Pts',(5.72069737671822,-19.8963286151593,-0.386712953469083));
#44442=CARTESIAN_POINT('Ctrl Pts',(5.72069737671822,-19.8683346103358,-0.406920018701532));
#44443=CARTESIAN_POINT('Ctrl Pts',(5.72069737671822,-19.4244549117969,-0.723945456553586));
#44444=CARTESIAN_POINT('Ctrl Pts',(5.72069737671822,-18.5166475191755,-1.26938810934469));
#44445=CARTESIAN_POINT('Ctrl Pts',(5.72069737671822,-17.0980510695729,-1.85639388115812));
#44446=CARTESIAN_POINT('Ctrl Pts',(5.72069737671822,-15.6085848723892,-2.2269564784001));
#44447=CARTESIAN_POINT('Ctrl Pts',(5.72069737671822,-14.0793083864286,-2.37286125618635));
#44448=CARTESIAN_POINT('Ctrl Pts',(5.72069737671822,-12.5448613797185,-2.29080978107595));
#44449=CARTESIAN_POINT('Ctrl Pts',(5.72069737671822,-11.1256905477962,-1.99925715472402));
#44450=CARTESIAN_POINT('Ctrl Pts',(5.72069737671822,-10.2428121437751,-1.68876505223976));
#44451=CARTESIAN_POINT('Ctrl Pts',(5.72069737671822,-9.85277650196055,-1.52389534674733));
#44452=CARTESIAN_POINT('',(6.,-19.5919343770476,-0.135488060647564));
#44453=CARTESIAN_POINT('Ctrl Pts',(5.99999999999966,-19.5919343770476,-0.135488060647564));
#44454=CARTESIAN_POINT('Ctrl Pts',(5.99999999999966,-19.4672328514344,-0.223609559568266));
#44455=CARTESIAN_POINT('Ctrl Pts',(6.00000000003739,-19.3409290917707,-0.308575891732745));
#44456=CARTESIAN_POINT('Ctrl Pts',(5.99999999795214,-19.2129690542321,-0.390478611967978));
#44457=CARTESIAN_POINT('Ctrl Pts',(5.99999999585997,-19.0845844257286,-0.472653097948809));
#44458=CARTESIAN_POINT('Ctrl Pts',(5.99999999148602,-18.9545321024225,-0.551743827842384));
#44459=CARTESIAN_POINT('Ctrl Pts',(5.99999999087342,-18.8227280871197,-0.627799835747431));
#44460=CARTESIAN_POINT('Ctrl Pts',(5.99999999026181,-18.6911389312267,-0.703731861473865));
#44461=CARTESIAN_POINT('Ctrl Pts',(5.99999999695614,-18.5578033768638,-0.77663926113671));
#44462=CARTESIAN_POINT('Ctrl Pts',(5.99999999953305,-18.4226147447749,-0.846524436286946));
#44463=CARTESIAN_POINT('Ctrl Pts',(5.99999999982096,-18.4075107787358,-0.85433236581324));
#44464=CARTESIAN_POINT('Ctrl Pts',(5.99999999999967,-18.3923836616462,-0.862102520704987));
#44465=CARTESIAN_POINT('Ctrl Pts',(5.99999999999967,-18.3772332302815,-0.869834866403388));
#44466=CARTESIAN_POINT('Ctrl Pts',(5.99999999999967,-18.3604562921101,-0.87839733453245));
#44467=CARTESIAN_POINT('Ctrl Pts',(5.99999999977963,-18.3436511842488,-0.886914343334167));
#44468=CARTESIAN_POINT('Ctrl Pts',(5.99999999940194,-18.32681838664,-0.895385513523014));
#44469=CARTESIAN_POINT('Ctrl Pts',(5.99999999572685,-18.1630285952216,-0.977813356508454));
#44470=CARTESIAN_POINT('Ctrl Pts',(5.99999998184218,-17.9966147415131,-1.05589757934824));
#44471=CARTESIAN_POINT('Ctrl Pts',(5.99999998033312,-17.8280085898849,-1.1293841227804));
#44472=CARTESIAN_POINT('Ctrl Pts',(5.99999997882264,-17.6592457266025,-1.20293896857085));
#44473=CARTESIAN_POINT('Ctrl Pts',(5.99999998731013,-17.4882868866805,-1.27188737333842));
#44474=CARTESIAN_POINT('Ctrl Pts',(5.99999999411993,-17.3155904515192,-1.33602010545033));
#44475=CARTESIAN_POINT('Ctrl Pts',(5.99999999739302,-17.2325847521993,-1.36684519036461));
#44476=CARTESIAN_POINT('Ctrl Pts',(5.99999999999966,-17.1491779727451,-1.39655845354114));
#44477=CARTESIAN_POINT('Ctrl Pts',(5.99999999999966,-17.0654226749711,-1.42514061332152));
#44478=CARTESIAN_POINT('Ctrl Pts',(5.99999999999966,-17.0325873369324,-1.43634593290379));
#44479=CARTESIAN_POINT('Ctrl Pts',(5.99999999960401,-16.9996980274663,-1.44737619951995));
#44480=CARTESIAN_POINT('Ctrl Pts',(5.99999999898846,-16.9667557482006,-1.45823114416469));
#44481=CARTESIAN_POINT('Ctrl Pts',(5.99999999507825,-16.757495451753,-1.527185356955));
#44482=CARTESIAN_POINT('Ctrl Pts',(5.99999998615646,-16.5460993317685,-1.5890690609484));
#44483=CARTESIAN_POINT('Ctrl Pts',(5.99999998771982,-16.332868561363,-1.64383881309663));
#44484=CARTESIAN_POINT('Ctrl Pts',(5.99999998928318,-16.1196377909574,-1.69860856524486));
#44485=CARTESIAN_POINT('Ctrl Pts',(5.99999999999966,-15.9045717674932,-1.74626453331427));
#44486=CARTESIAN_POINT('Ctrl Pts',(5.99999999999966,-15.68795707336,-1.78671132790344));
#44487=CARTESIAN_POINT('Ctrl Pts',(5.99999999999966,-15.6384076362316,-1.79596331292486));
#44488=CARTESIAN_POINT('Ctrl Pts',(5.9999999993466,-15.5887774796856,-1.80484067673141));
#44489=CARTESIAN_POINT('Ctrl Pts',(5.99999999845562,-15.5390744582055,-1.81334105408883));
#44490=CARTESIAN_POINT('Ctrl Pts',(5.99999999449748,-15.318269498527,-1.85110385851732));
#44491=CARTESIAN_POINT('Ctrl Pts',(5.99999998895124,-15.0960256116076,-1.88142252412455));
#44492=CARTESIAN_POINT('Ctrl Pts',(5.99999999115148,-14.8730323063916,-1.90421165291904));
#44493=CARTESIAN_POINT('Ctrl Pts',(5.99999999312717,-14.6727973227676,-1.92467496156659));
#44494=CARTESIAN_POINT('Ctrl Pts',(5.99999999999966,-14.4719585640787,-1.93906784227255));
#44495=CARTESIAN_POINT('Ctrl Pts',(5.99999999999966,-14.2710197611708,-1.94736399681091));
#44496=CARTESIAN_POINT('Ctrl Pts',(5.99999999999966,-14.2042169245834,-1.9501220835911));
#44497=CARTESIAN_POINT('Ctrl Pts',(5.99999999913623,-14.1374034485751,-1.95220396613166));
#44498=CARTESIAN_POINT('Ctrl Pts',(5.99999999780774,-14.0705875841289,-1.95360920069132));
#44499=CARTESIAN_POINT('Ctrl Pts',(5.99999999336888,-13.8473363769314,-1.95830449745114));
#44500=CARTESIAN_POINT('Ctrl Pts',(5.99999998477716,-13.6240582050389,-1.95544949150961));
#44501=CARTESIAN_POINT('Ctrl Pts',(5.99999998688347,-13.4010835092815,-1.94504172700609));
#44502=CARTESIAN_POINT('Ctrl Pts',(5.99999998862997,-13.2161992305184,-1.93641190456264));
#44503=CARTESIAN_POINT('Ctrl Pts',(5.99999999999966,-13.0315234335482,-1.92258841196678));
#44504=CARTESIAN_POINT('Ctrl Pts',(5.99999999999966,-12.8472489165034,-1.90354302704818));
#44505=CARTESIAN_POINT('Ctrl Pts',(5.99999999999966,-12.7639712033068,-1.89493599809809));
#44506=CARTESIAN_POINT('Ctrl Pts',(5.99999999683364,-12.6807722730351,-1.88527335009052));
#44507=CARTESIAN_POINT('Ctrl Pts',(5.99999999319098,-12.5976982773605,-1.87455629001131));
#44508=CARTESIAN_POINT('Ctrl Pts',(5.99999998466696,-12.4033004224575,-1.84947776244868));
#44509=CARTESIAN_POINT('Ctrl Pts',(5.99999997595983,-12.2095874450291,-1.81862158500248));
#44510=CARTESIAN_POINT('Ctrl Pts',(5.99999997954449,-12.0171122800012,-1.78211795983844));
#44511=CARTESIAN_POINT('Ctrl Pts',(5.99999998312914,-11.8246371149733,-1.7456143346744));
#44512=CARTESIAN_POINT('Ctrl Pts',(5.99999999999966,-11.6334002754345,-1.70346341636846));
#44513=CARTESIAN_POINT('Ctrl Pts',(5.99999999999966,-11.4439400773904,-1.65585042832456));
#44514=CARTESIAN_POINT('Ctrl Pts',(5.99999999999966,-11.3471401948288,-1.6315237797797));
#44515=CARTESIAN_POINT('Ctrl Pts',(5.99999999545176,-11.2508153992569,-1.60575152809878));
#44516=CARTESIAN_POINT('Ctrl Pts',(5.999999993073,-11.1549313534934,-1.5785357340368));
#44517=CARTESIAN_POINT('Ctrl Pts',(5.9999999894094,-11.0072572292376,-1.53661980816997));
#44518=CARTESIAN_POINT('Ctrl Pts',(5.9999999903115,-10.8606278293027,-1.49128219580575));
#44519=CARTESIAN_POINT('Ctrl Pts',(5.99999999276227,-10.7149545825572,-1.44250806010649));
#44520=CARTESIAN_POINT('Ctrl Pts',(5.99999999520009,-10.5700511250866,-1.39399166429694));
#44521=CARTESIAN_POINT('Ctrl Pts',(5.99999999786769,-10.4260933029596,-1.34207482786142));
#44522=CARTESIAN_POINT('Ctrl Pts',(5.99999999875682,-10.2830101379701,-1.28669419616467));
#44523=CARTESIAN_POINT('Ctrl Pts',(5.99999999915075,-10.2196170517512,-1.26215777246824));
#44524=CARTESIAN_POINT('Ctrl Pts',(5.99999999931868,-10.1563959085591,-1.23694079652416));
#44525=CARTESIAN_POINT('Ctrl Pts',(5.9999999993144,-10.09334190697,-1.2110347753893));
#44526=CARTESIAN_POINT('',(5.73644276520434,-19.8089520716699,-0.442549441855225));
#44527=CARTESIAN_POINT('Origin',(5.6,-19.5919343769637,-0.135488060672991));
#44528=CARTESIAN_POINT('Ctrl Pts',(5.73644276397732,-19.8089520717783,-0.442549442641763));
#44529=CARTESIAN_POINT('Ctrl Pts',(5.73708792252315,-19.4467189750557,-0.69823621872471));
#44530=CARTESIAN_POINT('Ctrl Pts',(5.7376256311114,-19.0680989321009,-0.930502816120376));
#44531=CARTESIAN_POINT('Ctrl Pts',(5.73805595543272,-18.6765903412666,-1.13733215216818));
#44532=CARTESIAN_POINT('Ctrl Pts',(5.73812189842541,-18.6165954795657,-1.16902672465618));
#44533=CARTESIAN_POINT('Ctrl Pts',(5.73818531973857,-18.556297873286,-1.20012401087123));
#44534=CARTESIAN_POINT('Ctrl Pts',(5.73824621957922,-18.4957100153502,-1.23061680204324));
#44535=CARTESIAN_POINT('Ctrl Pts',(5.73865147695443,-18.0925287259873,-1.43353077325557));
#44536=CARTESIAN_POINT('Ctrl Pts',(5.73894508021586,-17.6764985474971,-1.60967514468296));
#44537=CARTESIAN_POINT('Ctrl Pts',(5.73912707517464,-17.2512541404434,-1.75776137787843));
#44538=CARTESIAN_POINT('Ctrl Pts',(5.73915087505913,-17.1956439859834,-1.7771269431035));
#44539=CARTESIAN_POINT('Ctrl Pts',(5.73917276624537,-17.1398761856756,-1.79601269644437));
#44540=CARTESIAN_POINT('Ctrl Pts',(5.7391927487951,-17.0839588053956,-1.81441577480908));
#44541=CARTESIAN_POINT('Ctrl Pts',(5.73934700449672,-16.6523034438383,-1.95647871490941));
#44542=CARTESIAN_POINT('Ctrl Pts',(5.73938752580933,-16.2117387040006,-2.06977798720686));
#44543=CARTESIAN_POINT('Ctrl Pts',(5.7393143196508,-15.7661080919655,-2.15355053910136));
#44544=CARTESIAN_POINT('Ctrl Pts',(5.73930536900858,-15.7116225097048,-2.16379309458155));
#44545=CARTESIAN_POINT('Ctrl Pts',(5.73929471820266,-15.6570611342258,-2.17359426297402));
#44546=CARTESIAN_POINT('Ctrl Pts',(5.73928236720583,-15.6024309377374,-2.18295265701575));
#44547=CARTESIAN_POINT('Ctrl Pts',(5.73918135677838,-15.1556476072041,-2.25948861564609));
#44548=CARTESIAN_POINT('Ctrl Pts',(5.73896663207976,-14.7042654992233,-2.30640975727857));
#44549=CARTESIAN_POINT('Ctrl Pts',(5.73863815775707,-14.2522673186949,-2.32359669154592));
#44550=CARTESIAN_POINT('Ctrl Pts',(5.73859603594245,-14.1943054560695,-2.3258006533446));
#44551=CARTESIAN_POINT('Ctrl Pts',(5.73855204356702,-14.1363333925184,-2.32751565966289));
#44552=CARTESIAN_POINT('Ctrl Pts',(5.73850618051795,-14.0783594649322,-2.32874145708037));
#44553=CARTESIAN_POINT('Ctrl Pts',(5.73815298603535,-13.6318982772197,-2.33818140696285));
#44554=CARTESIAN_POINT('Ctrl Pts',(5.73768885011018,-13.1853304843906,-2.31860861075337));
#44555=CARTESIAN_POINT('Ctrl Pts',(5.73711370893976,-12.7423972722186,-2.27028161284945));
#44556=CARTESIAN_POINT('Ctrl Pts',(5.73703020877366,-12.6780913266681,-2.2632654009005));
#44557=CARTESIAN_POINT('Ctrl Pts',(5.73694436871282,-12.613861905765,-2.25564310254086));
#44558=CARTESIAN_POINT('Ctrl Pts',(5.73685618856742,-12.5497203746937,-2.24741549855154));
#44559=CARTESIAN_POINT('Ctrl Pts',(5.73622838727498,-12.0930627459389,-2.18883881562326));
#44560=CARTESIAN_POINT('Ctrl Pts',(5.73548197177282,-11.64086407108,-2.09958206443846));
#44561=CARTESIAN_POINT('Ctrl Pts',(5.73461687538872,-11.1970132530861,-1.98082802790191));
#44562=CARTESIAN_POINT('Ctrl Pts',(5.73452248333111,-11.1485839765889,-1.96787058400987));
#44563=CARTESIAN_POINT('Ctrl Pts',(5.73442667835076,-11.1002540362984,-1.95456194727603));
#44564=CARTESIAN_POINT('Ctrl Pts',(5.73432946037475,-11.0520284489647,-1.94090364135816));
#44565=CARTESIAN_POINT('Ctrl Pts',(5.73384874378987,-10.8135659690821,-1.87336701442942));
#44566=CARTESIAN_POINT('Ctrl Pts',(5.7333334786831,-10.5776553353801,-1.79728101389105));
#44567=CARTESIAN_POINT('Ctrl Pts',(5.7327836581836,-10.3449538542818,-1.71288850780721));
#44568=CARTESIAN_POINT('Ctrl Pts',(5.99999999997498,-19.5919300856734,0.135488304642552));
#44569=CARTESIAN_POINT('Ctrl Pts',(5.99999999997498,-19.5922326969623,0.0451632714407379));
#44570=CARTESIAN_POINT('Ctrl Pts',(5.99999999997498,-19.5922327064356,-0.0451632753777587));
#44571=CARTESIAN_POINT('Ctrl Pts',(5.99999999997498,-19.5919299350173,-0.135488872440526));
#44572=CARTESIAN_POINT('Ctrl Pts',(6.00000263487348,-19.829340627416,0.136284098535467));
#44573=CARTESIAN_POINT('Ctrl Pts',(6.00000263487349,-19.8296450131427,0.0454285037125645));
#44574=CARTESIAN_POINT('Ctrl Pts',(6.00000263487349,-19.8296450228323,-0.0454285076490772));
#44575=CARTESIAN_POINT('Ctrl Pts',(6.00000263487349,-19.8293404729368,-0.136284669416119));
#44576=CARTESIAN_POINT('Ctrl Pts',(5.83074066842648,-19.9958175555659,0.136842124817994));
#44577=CARTESIAN_POINT('Ctrl Pts',(5.8307406684265,-19.9961231855639,0.0456144897823355));
#44578=CARTESIAN_POINT('Ctrl Pts',(5.83074066842656,-19.9961231954074,-0.0456144937216663));
#44579=CARTESIAN_POINT('Ctrl Pts',(5.83074066842658,-19.9958173984086,-0.136842697865391));
#44580=CARTESIAN_POINT('Ctrl Pts',(5.59336110044015,-19.9918771871017,0.136828916806682));
#44581=CARTESIAN_POINT('Ctrl Pts',(5.59336110044031,-19.9921827876479,0.0456100876475798));
#44582=CARTESIAN_POINT('Ctrl Pts',(5.59336110044072,-19.9921827974882,-0.0456100915888983));
#44583=CARTESIAN_POINT('Ctrl Pts',(5.59336110044085,-19.9918770300065,-0.136829489802511));
#44584=CARTESIAN_POINT('',(5.99999999995608,-19.5919320087386,0.13548105287313));
#44585=CARTESIAN_POINT('',(5.59336167790261,-19.9918770519493,0.1368286131514));
#44586=CARTESIAN_POINT('Origin',(5.6,-19.5919343769583,0.135488060981343));
#44587=CARTESIAN_POINT('',(5.59336169562602,-19.9918770422853,-0.136828655448461));
#44588=CARTESIAN_POINT('Origin',(5.59336169592167,-15.0909939730293,-0.0604595362332659));
#44589=CARTESIAN_POINT('Origin',(5.6,-19.5919343771351,-0.13548806067611));
#44590=CARTESIAN_POINT('Ctrl Pts',(5.99999999999155,-19.5919320204748,0.13547755313224));
#44591=CARTESIAN_POINT('Ctrl Pts',(5.9999999999916,-19.592033064815,0.105317242942897));
#44592=CARTESIAN_POINT('Ctrl Pts',(5.99999999999962,-19.5921021554889,0.0751629221398726));
#44593=CARTESIAN_POINT('Ctrl Pts',(5.99999999999962,-19.5921363906274,0.0450478998554133));
#44594=CARTESIAN_POINT('Ctrl Pts',(5.99999999999962,-19.5921706257659,0.0149328775709451));
#44595=CARTESIAN_POINT('Ctrl Pts',(5.99999999999962,-19.592170005369,-0.0151428461949581));
#44596=CARTESIAN_POINT('Ctrl Pts',(5.99999999999962,-19.592136154094,-0.0452268828020266));
#44597=CARTESIAN_POINT('Ctrl Pts',(5.99999999999962,-19.5921023028189,-0.0753109194090861));
#44598=CARTESIAN_POINT('Ctrl Pts',(5.99999999999962,-19.5920352206656,-0.105403268857311));
#44599=CARTESIAN_POINT('Ctrl Pts',(5.99999999999962,-19.5919343770476,-0.135488060647564));
#44600=CARTESIAN_POINT('Origin',(5.6,-19.5919343769637,-0.135488060672991));
#44601=CARTESIAN_POINT('Origin',(5.600000004205,-19.5919343763234,-0.135488059062013));
#44602=CARTESIAN_POINT('Ctrl Pts',(-5.69266360647973,-19.9935541771414,
-0.0765565325209773));
#44603=CARTESIAN_POINT('Ctrl Pts',(-5.6578995530005,-19.9929007298199,-0.0929913866614558));
#44604=CARTESIAN_POINT('Ctrl Pts',(-5.54372467194083,-19.9908049362471,
-0.146471463308));
#44605=CARTESIAN_POINT('Ctrl Pts',(-5.34116840847122,-19.987350077468,-0.238479594457668));
#44606=CARTESIAN_POINT('Ctrl Pts',(-5.07576710978616,-19.983202471478,-0.353603245841893));
#44607=CARTESIAN_POINT('Ctrl Pts',(-4.78281267364433,-19.9789916798394,
-0.474026331255006));
#44608=CARTESIAN_POINT('Ctrl Pts',(-4.45929925449721,-19.9747248164902,
-0.598868153552744));
#44609=CARTESIAN_POINT('Ctrl Pts',(-4.10061014600622,-19.9704190336396,
-0.727254430583034));
#44610=CARTESIAN_POINT('Ctrl Pts',(-3.70134367776404,-19.9661195472229,
-0.857717930438492));
#44611=CARTESIAN_POINT('Ctrl Pts',(-3.25667261673587,-19.9619191732372,
-0.987522036063985));
#44612=CARTESIAN_POINT('Ctrl Pts',(-2.76260093160989,-19.9579588248915,
-1.11253953923502));
#44613=CARTESIAN_POINT('Ctrl Pts',(-2.21454168290653,-19.9544128020434,
-1.22755651364308));
#44614=CARTESIAN_POINT('Ctrl Pts',(-1.60546929114103,-19.9514859205532,
-1.32618245506953));
#44615=CARTESIAN_POINT('Ctrl Pts',(-0.938933076131297,-19.949459711508,
-1.39845731726721));
#44616=CARTESIAN_POINT('Ctrl Pts',(-0.23664535309699,-19.9485854307057,
-1.43362310534642));
#44617=CARTESIAN_POINT('Ctrl Pts',(0.4642466792577,-19.9487493934321,-1.4264266824266));
#44618=CARTESIAN_POINT('Ctrl Pts',(1.12888137961817,-19.9499401109169,-1.38089562429621));
#44619=CARTESIAN_POINT('Ctrl Pts',(1.73416986117937,-19.9520478855029,-1.3069947786214));
#44620=CARTESIAN_POINT('Ctrl Pts',(2.27382162043129,-19.9547877467897,-1.21535248098602));
#44621=CARTESIAN_POINT('Ctrl Pts',(2.75209716617804,-19.9579163581483,-1.11403336275034));
#44622=CARTESIAN_POINT('Ctrl Pts',(3.17956622801571,-19.9612850210495,-1.00747931862904));
#44623=CARTESIAN_POINT('Ctrl Pts',(3.56235593972046,-19.9647716235928,-0.8992296013094));
#44624=CARTESIAN_POINT('Ctrl Pts',(3.90389825972422,-19.9682668684595,-0.792406671009068));
#44625=CARTESIAN_POINT('Ctrl Pts',(4.20699235679262,-19.9716806547345,-0.689549337621442));
#44626=CARTESIAN_POINT('Ctrl Pts',(4.47553242579083,-19.9749594786553,-0.592113806854402));
#44627=CARTESIAN_POINT('Ctrl Pts',(4.71438132200868,-19.978087085808,-0.500492678804996));
#44628=CARTESIAN_POINT('Ctrl Pts',(4.92834984087647,-19.9810702155991,-0.41446474837091));
#44629=CARTESIAN_POINT('Ctrl Pts',(5.12118003508217,-19.983920132778,-0.333744232114557));
#44630=CARTESIAN_POINT('Ctrl Pts',(5.29544654744959,-19.9866446715028,-0.258197188744821));
#44631=CARTESIAN_POINT('Ctrl Pts',(5.45302073834614,-19.9892496568072,-0.18776958817749));
#44632=CARTESIAN_POINT('Ctrl Pts',(5.58355273456747,-19.9915337709002,-0.127837493099847));
#44633=CARTESIAN_POINT('Ctrl Pts',(5.66171486337773,-19.9929726011947,-0.0911864449715727));
#44634=CARTESIAN_POINT('Ctrl Pts',(5.692637247095,-19.9935542262535,-0.0765617004061338));
#44635=CARTESIAN_POINT('Ctrl Pts',(-5.75649789773431,-19.9991160246718,
-0.213743948047012));
#44636=CARTESIAN_POINT('Ctrl Pts',(-5.72140176446517,-19.9983763933301,
-0.230336779007504));
#44637=CARTESIAN_POINT('Ctrl Pts',(-5.6061363574476,-19.9959936786861,-0.284330788506753));
#44638=CARTESIAN_POINT('Ctrl Pts',(-5.40164108897797,-19.99200518302,-0.377224041508724));
#44639=CARTESIAN_POINT('Ctrl Pts',(-5.1336693786725,-19.9871042033416,-0.493465170018192));
#44640=CARTESIAN_POINT('Ctrl Pts',(-4.83782308796822,-19.982028337394,-0.615074766632991));
#44641=CARTESIAN_POINT('Ctrl Pts',(-4.51104023764979,-19.9767961134772,
-0.741169298308892));
#44642=CARTESIAN_POINT('Ctrl Pts',(-4.14862925030658,-19.9714345889302,
-0.870870253872186));
#44643=CARTESIAN_POINT('Ctrl Pts',(-3.7451010284537,-19.9660004924145,-1.00269864832984));
#44644=CARTESIAN_POINT('Ctrl Pts',(-3.29554242555684,-19.9606068553778,
-1.13389062270015));
#44645=CARTESIAN_POINT('Ctrl Pts',(-2.7958791388129,-19.9554270637761,-1.26027308336245));
#44646=CARTESIAN_POINT('Ctrl Pts',(-2.24144276789872,-19.9506811305415,
-1.37656929671114));
#44647=CARTESIAN_POINT('Ctrl Pts',(-1.6251068839532,-19.9466381361631,-1.47630757617145));
#44648=CARTESIAN_POINT('Ctrl Pts',(-0.950466599309452,-19.9437069324571,
-1.54940294776633));
#44649=CARTESIAN_POINT('Ctrl Pts',(-0.239549742799721,-19.9423158121451,
-1.58496415386577));
#44650=CARTESIAN_POINT('Ctrl Pts',(0.469949066288936,-19.9425954820282,
-1.57768764486034));
#44651=CARTESIAN_POINT('Ctrl Pts',(1.14273524885353,-19.9444157720885,-1.53164185334408));
#44652=CARTESIAN_POINT('Ctrl Pts',(1.7553509886388,-19.9474228366483,-1.4569028237362));
#44653=CARTESIAN_POINT('Ctrl Pts',(2.30141447279339,-19.9511844635576,-1.36422916038421));
#44654=CARTESIAN_POINT('Ctrl Pts',(2.78524782072098,-19.9553661337753,-1.26178440856533));
#44655=CARTESIAN_POINT('Ctrl Pts',(3.2175668220097,-19.9597796002856,-1.15406529307948));
#44656=CARTESIAN_POINT('Ctrl Pts',(3.60459389090943,-19.9642748189524,-1.04465245493347));
#44657=CARTESIAN_POINT('Ctrl Pts',(3.94982589636675,-19.9687199844506,-0.936702115595601));
#44658=CARTESIAN_POINT('Ctrl Pts',(4.25611894267221,-19.97300856616,-0.832778034999717));
#44659=CARTESIAN_POINT('Ctrl Pts',(4.52743270510596,-19.9770800474319,-0.734348454396371));
#44660=CARTESIAN_POINT('Ctrl Pts',(4.76870079203887,-19.9809191981262,-0.64180654650571));
#44661=CARTESIAN_POINT('Ctrl Pts',(4.98479925050148,-19.9845374733531,-0.554925572284122));
#44662=CARTESIAN_POINT('Ctrl Pts',(5.17952065874217,-19.9879503114012,-0.47341384725153));
#44663=CARTESIAN_POINT('Ctrl Pts',(5.35547601561356,-19.9911683754546,-0.39713317740571));
#44664=CARTESIAN_POINT('Ctrl Pts',(5.51456435191784,-19.9942009298587,-0.326026136389495));
#44665=CARTESIAN_POINT('Ctrl Pts',(5.64634486806084,-19.9968224547552,-0.265517744872236));
#44666=CARTESIAN_POINT('Ctrl Pts',(5.72525346105499,-19.9984580797953,-0.228514505250355));
#44667=CARTESIAN_POINT('Ctrl Pts',(5.75647083566732,-19.999118312624,-0.213749311958633));
#44668=CARTESIAN_POINT('Ctrl Pts',(-5.81361929054906,-19.9261291309016,
-0.33332743564323));
#44669=CARTESIAN_POINT('Ctrl Pts',(-5.77819666234262,-19.9253136755351,
-0.350029910484856));
#44670=CARTESIAN_POINT('Ctrl Pts',(-5.66186327713482,-19.9226787667006,
-0.404375005602182));
#44671=CARTESIAN_POINT('Ctrl Pts',(-5.45549017824741,-19.9182225720687,
-0.497841767049385));
#44672=CARTESIAN_POINT('Ctrl Pts',(-5.18505475622245,-19.9126637158777,
-0.614753500436186));
#44673=CARTESIAN_POINT('Ctrl Pts',(-4.88646290762062,-19.9068351818877,
-0.737031525938342));
#44674=CARTESIAN_POINT('Ctrl Pts',(-4.55660702641851,-19.9007662575288,
-0.863795521452588));
#44675=CARTESIAN_POINT('Ctrl Pts',(-4.19073575184427,-19.8944934655263,
-0.994167366746355));
#44676=CARTESIAN_POINT('Ctrl Pts',(-3.78329193486844,-19.8880843570324,
-1.12666201965898));
#44677=CARTESIAN_POINT('Ctrl Pts',(-3.32929912805282,-19.8816701335577,
-1.25850001195665));
#44678=CARTESIAN_POINT('Ctrl Pts',(-2.82462928254054,-19.8754524902486,
-1.38548279361662));
#44679=CARTESIAN_POINT('Ctrl Pts',(-2.26455890682294,-19.8696904124827,
-1.50230118360881));
#44680=CARTESIAN_POINT('Ctrl Pts',(-1.64189026826602,-19.8647068292226,
-1.60244613802217));
#44681=CARTESIAN_POINT('Ctrl Pts',(-0.960272299876233,-19.8610163311095,
-1.6757919689123));
#44682=CARTESIAN_POINT('Ctrl Pts',(-0.242005517629495,-19.8591930557594,
-1.71142835480064));
#44683=CARTESIAN_POINT('Ctrl Pts',(0.474779168951458,-19.85956938191,-1.70414269385846));
#44684=CARTESIAN_POINT('Ctrl Pts',(1.15453262843177,-19.8619165859985,-1.65797498745275));
#44685=CARTESIAN_POINT('Ctrl Pts',(1.77347554177536,-19.86567899107,-1.58296511398592));
#44686=CARTESIAN_POINT('Ctrl Pts',(2.32514101758377,-19.8703024011944,-1.48990602506843));
#44687=CARTESIAN_POINT('Ctrl Pts',(2.81388750100801,-19.8753761019103,-1.38699980286476));
#44688=CARTESIAN_POINT('Ctrl Pts',(3.25054379792609,-19.880678426273,-1.27877109361568));
#44689=CARTESIAN_POINT('Ctrl Pts',(3.64140302971636,-19.8860353147015,-1.1688235090255));
#44690=CARTESIAN_POINT('Ctrl Pts',(3.99000761186061,-19.8912952372146,-1.06033298708642));
#44691=CARTESIAN_POINT('Ctrl Pts',(4.29925370235094,-19.8963369129699,-0.955878719607947));
#44692=CARTESIAN_POINT('Ctrl Pts',(4.57315108204409,-19.9010930802668,-0.856937659179218));
#44693=CARTESIAN_POINT('Ctrl Pts',(4.81669094406161,-19.905548736309,-0.763905192229798));
#44694=CARTESIAN_POINT('Ctrl Pts',(5.03480427220289,-19.9097188605832,-0.676552771581171));
#44695=CARTESIAN_POINT('Ctrl Pts',(5.23132679680547,-19.9136220551603,-0.59458595913314));
#44696=CARTESIAN_POINT('Ctrl Pts',(5.40890088270857,-19.91727106624,-0.517864337069929));
#44697=CARTESIAN_POINT('Ctrl Pts',(5.56945003295899,-19.9206778466155,-0.446329088409351));
#44698=CARTESIAN_POINT('Ctrl Pts',(5.70244415132626,-19.9235953792304,-0.385439711430928));
#44699=CARTESIAN_POINT('Ctrl Pts',(5.7820841767363,-19.9254039957874,-0.348195793130167));
#44700=CARTESIAN_POINT('Ctrl Pts',(5.81359177736081,-19.9261333785129,-0.333334173054417));
#44701=CARTESIAN_POINT('Ctrl Pts',(-5.84786851513962,-19.7956125204352,
-0.401492745344046));
#44702=CARTESIAN_POINT('Ctrl Pts',(-5.81221747993369,-19.7947530449905,
-0.418225664741117));
#44703=CARTESIAN_POINT('Ctrl Pts',(-5.69514122740039,-19.791971991235,-0.472660196859671));
#44704=CARTESIAN_POINT('Ctrl Pts',(-5.48748337881077,-19.7872462977438,
-0.566227652874011));
#44705=CARTESIAN_POINT('Ctrl Pts',(-5.2153886925705,-19.781311093658,-0.68317497857044));
#44706=CARTESIAN_POINT('Ctrl Pts',(-4.91497503518046,-19.7750551206435,
-0.805416130630983));
#44707=CARTESIAN_POINT('Ctrl Pts',(-4.58311256625854,-19.7685147237548,
-0.932079108994651));
#44708=CARTESIAN_POINT('Ctrl Pts',(-4.21502210732507,-19.7617327707534,
-1.06229067382155));
#44709=CARTESIAN_POINT('Ctrl Pts',(-3.80511703616425,-19.7547838809892,
-1.19456711399924));
#44710=CARTESIAN_POINT('Ctrl Pts',(-3.34839805974144,-19.7478102400708,
-1.32612935869123));
#44711=CARTESIAN_POINT('Ctrl Pts',(-2.84072303534511,-19.7410296838559,
-1.4527809575621));
#44712=CARTESIAN_POINT('Ctrl Pts',(-2.27735525004778,-19.734722413695,-1.56921970799552));
#44713=CARTESIAN_POINT('Ctrl Pts',(-1.65107529416229,-19.7292395749277,
-1.6689534337654));
#44714=CARTESIAN_POINT('Ctrl Pts',(-0.965578662808645,-19.725150041307,
-1.74191112574034));
#44715=CARTESIAN_POINT('Ctrl Pts',(-0.243318637187852,-19.7231014047023,
-1.77728251315008));
#44716=CARTESIAN_POINT('Ctrl Pts',(0.477371881719029,-19.7235280256043,
-1.77006092556454));
#44717=CARTESIAN_POINT('Ctrl Pts',(1.16093897371515,-19.7261505983202,-1.72419699779472));
#44718=CARTESIAN_POINT('Ctrl Pts',(1.78342015357474,-19.7303109488223,-1.64955795707234));
#44719=CARTESIAN_POINT('Ctrl Pts',(2.33829376637848,-19.7353926172284,-1.55686585596026));
#44720=CARTESIAN_POINT('Ctrl Pts',(2.82991911146498,-19.740945210087,-1.45429027277005));
#44721=CARTESIAN_POINT('Ctrl Pts',(3.2691730799956,-19.7467292140027,-1.34634906850792));
#44722=CARTESIAN_POINT('Ctrl Pts',(3.66237499389563,-19.752557259858,-1.23664397669946));
#44723=CARTESIAN_POINT('Ctrl Pts',(4.01308062613083,-19.7582664543786,-1.12835107947497));
#44724=CARTESIAN_POINT('Ctrl Pts',(4.324198027549,-19.7637266189471,-1.02405114962652));
#44725=CARTESIAN_POINT('Ctrl Pts',(4.59975757565947,-19.7688659250237,-0.925224072311745));
#44726=CARTESIAN_POINT('Ctrl Pts',(4.84477861694369,-19.7736687391877,-0.832268454398782));
#44727=CARTESIAN_POINT('Ctrl Pts',(5.06422123234029,-19.7781513802583,-0.744958162908533));
#44728=CARTESIAN_POINT('Ctrl Pts',(5.26194473317568,-19.7823337120554,-0.662999920489588));
#44729=CARTESIAN_POINT('Ctrl Pts',(5.44060899256178,-19.7862292306473,-0.586253735975595));
#44730=CARTESIAN_POINT('Ctrl Pts',(5.60215186593309,-19.7898510677042,-0.514661792941206));
#44731=CARTESIAN_POINT('Ctrl Pts',(5.73598088940997,-19.7929394945044,-0.453693877884493));
#44732=CARTESIAN_POINT('Ctrl Pts',(5.81613009557532,-19.7948483759911,-0.416388525266093));
#44733=CARTESIAN_POINT('Ctrl Pts',(5.8478409291635,-19.79561789436,-0.401501639466543));
#44734=CARTESIAN_POINT('',(-5.593361696257,-19.9918770425327,-0.136828655009776));
#44735=CARTESIAN_POINT('Ctrl Pts',(-5.593361696257,-19.9918770425327,-0.136828655009776));
#44736=CARTESIAN_POINT('Ctrl Pts',(-5.53987020056264,-19.9909059753986,
-0.161652254976759));
#44737=CARTESIAN_POINT('Ctrl Pts',(-5.479349726203,-19.9898406677287,-0.189279917712342));
#44738=CARTESIAN_POINT('Ctrl Pts',(-5.37802554666591,-19.9881259346619,
-0.234797771553107));
#44739=CARTESIAN_POINT('Ctrl Pts',(-5.34249357548727,-19.9875348396451,
-0.250641374196676));
#44740=CARTESIAN_POINT('Ctrl Pts',(-5.2865597517199,-19.9866219206319,-0.275323558975893));
#44741=CARTESIAN_POINT('Ctrl Pts',(-5.25793387308637,-19.9861588948391,
-0.287893099482891));
#44742=CARTESIAN_POINT('Ctrl Pts',(-5.22831954432805,-19.985686638106,-0.300781885343407));
#44743=CARTESIAN_POINT('Ctrl Pts',(-5.20835700290589,-19.9853698241558,
-0.309442305333269));
#44744=CARTESIAN_POINT('Ctrl Pts',(-5.19631311251836,-19.9851797336765,
-0.314648127603555));
#44745=CARTESIAN_POINT('Ctrl Pts',(-5.12207990283231,-19.9840128909541,
-0.346642302652193));
#44746=CARTESIAN_POINT('Ctrl Pts',(-5.04939710257819,-19.9829026197028,
-0.377391298242854));
#44747=CARTESIAN_POINT('Ctrl Pts',(-4.93032631473058,-19.9811479246296,
-0.426585798090019));
#44748=CARTESIAN_POINT('Ctrl Pts',(-4.88896162087032,-19.9805481587181,
-0.443491790520733));
#44749=CARTESIAN_POINT('Ctrl Pts',(-4.8244029332133,-19.9796290973292,-0.469528375465107));
#44750=CARTESIAN_POINT('Ctrl Pts',(-4.79149567766814,-19.9791647189891,
-0.482715712402016));
#44751=CARTESIAN_POINT('Ctrl Pts',(-4.75200503402798,-19.9786151662145,
-0.498374697482097));
#44752=CARTESIAN_POINT('Ctrl Pts',(-4.73484500557417,-19.9783780583391,
-0.50514176176339));
#44753=CARTESIAN_POINT('Ctrl Pts',(-4.72335266062857,-19.9782196434084,
-0.509665304276756));
#44754=CARTESIAN_POINT('Ctrl Pts',(-4.71643686245319,-19.9781245780082,
-0.51238154988444));
#44755=CARTESIAN_POINT('Ctrl Pts',(-4.56282068320486,-19.9760172189209,
-0.572619677228507));
#44756=CARTESIAN_POINT('Ctrl Pts',(-4.38688909346539,-19.9737322566863,
-0.638684826646137));
#44757=CARTESIAN_POINT('Ctrl Pts',(-4.08253603951726,-19.9701218617751,
-0.744793257689181));
#44758=CARTESIAN_POINT('Ctrl Pts',(-3.97434240997806,-19.9688883655198,
-0.781293850177061));
#44759=CARTESIAN_POINT('Ctrl Pts',(-3.80193804833453,-19.9670227815378,
-0.836868705234022));
#44760=CARTESIAN_POINT('Ctrl Pts',(-3.71320738817908,-19.9660862577162,
-0.864859033956662));
#44761=CARTESIAN_POINT('Ctrl Pts',(-3.60526344583045,-19.964994870515,-0.89764772607499));
#44762=CARTESIAN_POINT('Ctrl Pts',(-3.55018526494765,-19.9644505593352,
-0.914045544112392));
#44763=CARTESIAN_POINT('Ctrl Pts',(-3.52634328534606,-19.9642176976363,
-0.921070682546635));
#44764=CARTESIAN_POINT('Ctrl Pts',(-3.51039595562554,-19.9640625620639,
-0.925753187407788));
#44765=CARTESIAN_POINT('Ctrl Pts',(-3.50119799341242,-19.9639734865516,
-0.928443254817963));
#44766=CARTESIAN_POINT('Ctrl Pts',(-3.27586137135579,-19.9617989531766,
-0.994142053109484));
#44767=CARTESIAN_POINT('Ctrl Pts',(-3.02941181863928,-19.9596442378471,
-1.06010677386181));
#44768=CARTESIAN_POINT('Ctrl Pts',(-2.61782551984484,-19.9566053802805,
-1.15486737579028));
#44769=CARTESIAN_POINT('Ctrl Pts',(-2.47364475862675,-19.9556253433564,
-1.18573178195283));
#44770=CARTESIAN_POINT('Ctrl Pts',(-2.24689562436969,-19.9542426642482,
-1.2297975138448));
#44771=CARTESIAN_POINT('Ctrl Pts',(-2.16956624754569,-19.9537963634296,
-1.244113003799));
#44772=CARTESIAN_POINT('Ctrl Pts',(-2.01141482975437,-19.9529394759166,
-1.27179246316136));
#44773=CARTESIAN_POINT('Ctrl Pts',(-1.93261264247602,-19.9525384232272,
-1.2848437335703));
#44774=CARTESIAN_POINT('Ctrl Pts',(-1.50967150883639,-19.9505433693017,
-1.35031376335494));
#44775=CARTESIAN_POINT('Ctrl Pts',(-1.15506197268932,-19.9493582218701,
-1.39106252074058));
#44776=CARTESIAN_POINT('Ctrl Pts',(-0.598762724615647,-19.9483492700185,
-1.42765146731114));
#44777=CARTESIAN_POINT('Ctrl Pts',(-0.409265484615582,-19.9481398188074,
-1.43576259964849));
#44778=CARTESIAN_POINT('Ctrl Pts',(-0.118923388652217,-19.9480099636445,
-1.44097617568032));
#44779=CARTESIAN_POINT('Ctrl Pts',(-0.0211266506705514,-19.9479967667065,
-1.44155574198219));
#44780=CARTESIAN_POINT('Ctrl Pts',(0.127092515292763,-19.9480204726378,
-1.44059056689962));
#44781=CARTESIAN_POINT('Ctrl Pts',(0.201583113022127,-19.948043564824,-1.43964942808039));
#44782=CARTESIAN_POINT('Ctrl Pts',(0.276645232873043,-19.9480847522935,
-1.43800298297456));
#44783=CARTESIAN_POINT('Ctrl Pts',(0.326813651022889,-19.9481163609107,
-1.43674672693249));
#44784=CARTESIAN_POINT('Ctrl Pts',(0.353716444626537,-19.9481356343534,
-1.43598444819588));
#44785=CARTESIAN_POINT('Ctrl Pts',(0.752470687267383,-19.9484522622495,
-1.42352583710267));
#44786=CARTESIAN_POINT('Ctrl Pts',(1.10888528711956,-19.94924020033,-1.39466314562183));
#44787=CARTESIAN_POINT('Ctrl Pts',(1.61518192059489,-19.9510623368019,-1.3331689588221));
#44788=CARTESIAN_POINT('Ctrl Pts',(1.86124892075682,-19.9521291255488,-1.29787744892242));
#44789=CARTESIAN_POINT('Ctrl Pts',(2.13593478360488,-19.9535986471434,-1.25040494578588));
#44790=CARTESIAN_POINT('Ctrl Pts',(2.25100180253815,-19.9542710478476,-1.2288842616072));
#44791=CARTESIAN_POINT('Ctrl Pts',(2.32712303877902,-19.954728184487,-1.21429513010396));
#44792=CARTESIAN_POINT('Ctrl Pts',(2.36664298291456,-19.9549722906808,-1.20652715275755));
#44793=CARTESIAN_POINT('Ctrl Pts',(2.68808813071481,-19.9570066067568,-1.14195559351965));
#44794=CARTESIAN_POINT('Ctrl Pts',(2.94934760456572,-19.9590245821492,-1.07929220022979));
#44795=CARTESIAN_POINT('Ctrl Pts',(3.30453249571811,-19.9621129152685,-0.984801908720499));
#44796=CARTESIAN_POINT('Ctrl Pts',(3.41681007283158,-19.9631531096153,-0.953206328513377));
#44797=CARTESIAN_POINT('Ctrl Pts',(3.57605035859579,-19.964703024329,-0.906426490572821));
#44798=CARTESIAN_POINT('Ctrl Pts',(3.6533764815014,-19.965475443408,-0.883188111121659));
#44799=CARTESIAN_POINT('Ctrl Pts',(3.73957575659907,-19.966366921966,-0.856488313231046));
#44800=CARTESIAN_POINT('Ctrl Pts',(3.77565804557831,-19.9667463830614,-0.845148104339534));
#44801=CARTESIAN_POINT('Ctrl Pts',(3.79952173656643,-19.9669987212599,-0.837612313145826));
#44802=CARTESIAN_POINT('Ctrl Pts',(3.80961452999613,-19.9671059351478,-0.834412391154652));
#44803=CARTESIAN_POINT('Ctrl Pts',(4.03884499603919,-19.9695563463032,-0.761336544705132));
#44804=CARTESIAN_POINT('Ctrl Pts',(4.23284563458667,-19.9718571567274,-0.69355479857008));
#44805=CARTESIAN_POINT('Ctrl Pts',(4.49122806875653,-19.9751161272079,-0.598760536622438));
#44806=CARTESIAN_POINT('Ctrl Pts',(4.5719191262046,-19.9761713988021,-0.568286225150129));
#44807=CARTESIAN_POINT('Ctrl Pts',(4.68480108146387,-19.9776910507615,-0.524711922251623));
#44808=CARTESIAN_POINT('Ctrl Pts',(4.73920340136529,-19.9784351075424,-0.50345661051287));
#44809=CARTESIAN_POINT('Ctrl Pts',(4.79910512355925,-19.9792722874665,-0.479661705607389));
#44810=CARTESIAN_POINT('Ctrl Pts',(4.82401279356573,-19.9796241229337,-0.469684812447406));
#44811=CARTESIAN_POINT('Ctrl Pts',(4.84044801875936,-19.9798570968037,-0.463083263109677));
#44812=CARTESIAN_POINT('Ctrl Pts',(4.84692845458122,-19.9799492057087,-0.460474746581707));
#44813=CARTESIAN_POINT('Ctrl Pts',(4.93422806898291,-19.9811954511744,-0.425211237863346));
#44814=CARTESIAN_POINT('Ctrl Pts',(5.00665608368955,-19.9822655538964,-0.395187232802343));
#44815=CARTESIAN_POINT('Ctrl Pts',(5.10754064194054,-19.9837976839523,-0.352644522552055));
#44816=CARTESIAN_POINT('Ctrl Pts',(5.15604355511379,-19.9845455683222,-0.331992751655454));
#44817=CARTESIAN_POINT('Ctrl Pts',(5.20923639673284,-19.9853831869685,-0.309054215570777));
#44818=CARTESIAN_POINT('Ctrl Pts',(5.2313060666232,-19.9857343668377,-0.299475845519313));
#44819=CARTESIAN_POINT('Ctrl Pts',(5.24585756605408,-19.9859667178632,-0.29314682790016));
#44820=CARTESIAN_POINT('Ctrl Pts',(5.251989654479,-19.9860649191825,-0.290474904973647));
#44821=CARTESIAN_POINT('Ctrl Pts',(5.39099848893191,-19.9883000550751,-0.229750246669846));
#44822=CARTESIAN_POINT('Ctrl Pts',(5.5020635061168,-19.9902196450197,-0.179197068989747));
#44823=CARTESIAN_POINT('Ctrl Pts',(5.593361696298,-19.9918770423739,-0.136828655184827));
#44824=CARTESIAN_POINT('',(-5.73644346265456,-19.808951158735,-0.442548130349197));
#44825=CARTESIAN_POINT('Origin',(-5.599999999997,-19.5919343769627,-0.135488060674723));
#44826=CARTESIAN_POINT('Ctrl Pts',(-5.73644387762025,-19.8089519016918,
-0.442549068003315));
#44827=CARTESIAN_POINT('Ctrl Pts',(-5.73644352459178,-19.8089518942983,
-0.442549230096899));
#44828=CARTESIAN_POINT('Ctrl Pts',(-5.73644317156308,-19.8089518869049,
-0.442549392190579));
#44829=CARTESIAN_POINT('Ctrl Pts',(-5.73644281853413,-19.8089518795114,
-0.442549554284354));
#44830=CARTESIAN_POINT('Ctrl Pts',(-5.67992322800445,-19.8077681932076,
-0.468500609840852));
#44831=CARTESIAN_POINT('Ctrl Pts',(-5.61717096311638,-19.8064997639747,
-0.496914357267869));
#44832=CARTESIAN_POINT('Ctrl Pts',(-5.54808344604347,-19.8051527722357,
-0.527556343709489));
#44833=CARTESIAN_POINT('Ctrl Pts',(-5.52951991964327,-19.8047908411986,
-0.535789717093907));
#44834=CARTESIAN_POINT('Ctrl Pts',(-5.51049891108683,-19.8044231966611,
-0.544183691954582));
#44835=CARTESIAN_POINT('Ctrl Pts',(-5.49101823034769,-19.8040498532496,
-0.552733116195771));
#44836=CARTESIAN_POINT('Ctrl Pts',(-5.42195695738163,-19.802726307548,-0.583041816858224));
#44837=CARTESIAN_POINT('Ctrl Pts',(-5.34711975453104,-19.8013309991599,
-0.615307999901524));
#44838=CARTESIAN_POINT('Ctrl Pts',(-5.26639707370599,-19.7998745194251,
-0.649265632063439));
#44839=CARTESIAN_POINT('Ctrl Pts',(-5.25084851317281,-19.7995939766694,
-0.655806449264208));
#44840=CARTESIAN_POINT('Ctrl Pts',(-5.23508154960726,-19.7993111671559,
-0.662409872904726));
#44841=CARTESIAN_POINT('Ctrl Pts',(-5.21909533754653,-19.7990261703001,
-0.669073785702921));
#44842=CARTESIAN_POINT('Ctrl Pts',(-5.19132318127546,-19.7985310575625,
-0.680650713802282));
#44843=CARTESIAN_POINT('Ctrl Pts',(-5.16288932753674,-19.7980293405181,
-0.692410241756752));
#44844=CARTESIAN_POINT('Ctrl Pts',(-5.13378929916158,-19.7975215543759,
-0.70434063927198));
#44845=CARTESIAN_POINT('Ctrl Pts',(-5.06602552723238,-19.7963390983355,
-0.732122355695892));
#44846=CARTESIAN_POINT('Ctrl Pts',(-4.99464964026495,-19.7951236537926,
-0.760832113190979));
#44847=CARTESIAN_POINT('Ctrl Pts',(-4.91960196679892,-19.7938827764332,
-0.790306636991108));
#44848=CARTESIAN_POINT('Ctrl Pts',(-4.82891093456434,-19.7923832436242,
-0.825924996156716));
#44849=CARTESIAN_POINT('Ctrl Pts',(-4.73285787622835,-19.7908464468696,
-0.862661733594464));
#44850=CARTESIAN_POINT('Ctrl Pts',(-4.63133263561869,-19.789288958625,-0.900183444709471));
#44851=CARTESIAN_POINT('Ctrl Pts',(-4.61738480421122,-19.789074986382,-0.905338285984501));
#44852=CARTESIAN_POINT('Ctrl Pts',(-4.60333368087305,-19.7888606286327,
-0.910507863030616));
#44853=CARTESIAN_POINT('Ctrl Pts',(-4.58917897112926,-19.7886459332474,
-0.91569123384208));
#44854=CARTESIAN_POINT('Ctrl Pts',(-4.5569989083199,-19.7881578334482,-0.927475382107651));
#44855=CARTESIAN_POINT('Ctrl Pts',(-4.52428345175846,-19.7876679863891,
-0.939330860040537));
#44856=CARTESIAN_POINT('Ctrl Pts',(-4.49102921787,-19.7871769688327,-0.951246233153467));
#44857=CARTESIAN_POINT('Ctrl Pts',(-4.45061974413422,-19.7865803001162,
-0.965725410706443));
#44858=CARTESIAN_POINT('Ctrl Pts',(-4.40941469472378,-19.7859819008893,
-0.980293065109979));
#44859=CARTESIAN_POINT('Ctrl Pts',(-4.36740795073453,-19.7853828769608,
-0.994927609811942));
#44860=CARTESIAN_POINT('Ctrl Pts',(-4.34640457873991,-19.7850833649966,
-1.00224488216292));
#44861=CARTESIAN_POINT('Ctrl Pts',(-4.3252007791973,-19.7847836891736,-1.00957886551706));
#44862=CARTESIAN_POINT('Ctrl Pts',(-4.30379578735247,-19.7844840053655,
-1.01692674026769));
#44863=CARTESIAN_POINT('Ctrl Pts',(-4.29309329143005,-19.7843341634614,
-1.02060067764301));
#44864=CARTESIAN_POINT('Ctrl Pts',(-4.28234049717896,-19.7841843190688,
-1.02427808712802));
#44865=CARTESIAN_POINT('Ctrl Pts',(-4.27153730830466,-19.7840344905978,
-1.02795861025227));
#44866=CARTESIAN_POINT('Ctrl Pts',(-4.26343491664894,-19.7839221192445,
-1.03071900259545));
#44867=CARTESIAN_POINT('Ctrl Pts',(-4.25530417799723,-19.7838097568063,
-1.03348114629917));
#44868=CARTESIAN_POINT('Ctrl Pts',(-4.24714505165301,-19.7836974110832,
-1.03624488840223));
#44869=CARTESIAN_POINT('Ctrl Pts',(-4.24442534287161,-19.7836599625088,
-1.03716613576992));
#44870=CARTESIAN_POINT('Ctrl Pts',(-4.24040571674569,-19.7836047034882,
-1.03852596299984));
#44871=CARTESIAN_POINT('Ctrl Pts',(-4.2389764612492,-19.7835850712593,-1.03900915753671));
#44872=CARTESIAN_POINT('Ctrl Pts',(-4.23363824302541,-19.7835117455856,
-1.0408138718713));
#44873=CARTESIAN_POINT('Ctrl Pts',(-4.22827574141502,-19.7834382142521,
-1.0426233946655));
#44874=CARTESIAN_POINT('Ctrl Pts',(-4.22288893010133,-19.7833644814854,
-1.04443764064879));
#44875=CARTESIAN_POINT('Ctrl Pts',(-4.14210743949879,-19.7822587730341,
-1.07164436579935));
#44876=CARTESIAN_POINT('Ctrl Pts',(-4.05585946314527,-19.7811075327797,
-1.09991742926328));
#44877=CARTESIAN_POINT('Ctrl Pts',(-3.96405509253658,-19.7799263357334,
-1.12894321402821));
#44878=CARTESIAN_POINT('Ctrl Pts',(-3.91582494302358,-19.7793057845574,
-1.14419213877616));
#44879=CARTESIAN_POINT('Ctrl Pts',(-3.86606114192558,-19.7786770117211,
-1.15964798280796));
#44880=CARTESIAN_POINT('Ctrl Pts',(-3.81475024023462,-19.7780426029928,
-1.17525948392769));
#44881=CARTESIAN_POINT('Ctrl Pts',(-3.7199189720691,-19.7768701078258,-1.20411219164403));
#44882=CARTESIAN_POINT('Ctrl Pts',(-3.61980308476554,-19.7756781932112,
-1.23349960388482));
#44883=CARTESIAN_POINT('Ctrl Pts',(-3.51432014675643,-19.7744851328542,
-1.26306109037886));
#44884=CARTESIAN_POINT('Ctrl Pts',(-3.46379574875574,-19.7739136787645,
-1.27722050172355));
#44885=CARTESIAN_POINT('Ctrl Pts',(-3.41204003840321,-19.7733420037037,
-1.29141910527109));
#44886=CARTESIAN_POINT('Ctrl Pts',(-3.35904414017396,-19.7727723575387,
-1.30561300663643));
#44887=CARTESIAN_POINT('Ctrl Pts',(-3.24837095335384,-19.7715827455394,
-1.33525462702593));
#44888=CARTESIAN_POINT('Ctrl Pts',(-3.13228852468873,-19.770401775826,-1.36487935655462));
#44889=CARTESIAN_POINT('Ctrl Pts',(-3.01072522401274,-19.7692520420384,
-1.39404936396976));
#44890=CARTESIAN_POINT('Ctrl Pts',(-2.96856990915526,-19.7688533412006,
-1.4041648415863));
#44891=CARTESIAN_POINT('Ctrl Pts',(-2.92501779804032,-19.7684516366423,
-1.41439774391956));
#44892=CARTESIAN_POINT('Ctrl Pts',(-2.88137003129703,-19.7680601552081,
-1.42441922738617));
#44893=CARTESIAN_POINT('Ctrl Pts',(-2.87181245808014,-19.7679744323235,
-1.42661363661076));
#44894=CARTESIAN_POINT('Ctrl Pts',(-2.86225034694103,-19.7678891900111,
-1.42879810081594));
#44895=CARTESIAN_POINT('Ctrl Pts',(-2.85269743997054,-19.7678045507344,
-1.43096949490122));
#44896=CARTESIAN_POINT('Ctrl Pts',(-2.83187074692257,-19.7676200250983,
-1.43570344219496));
#44897=CARTESIAN_POINT('Ctrl Pts',(-2.81108776110388,-19.7674383746355,
-1.44037508987938));
#44898=CARTESIAN_POINT('Ctrl Pts',(-2.79049137151887,-19.7672607679526,
-1.44495405126276));
#44899=CARTESIAN_POINT('Ctrl Pts',(-2.6196981206351,-19.7657879844525,-1.48292457503392));
#44900=CARTESIAN_POINT('Ctrl Pts',(-2.45356651026147,-19.7645069952526,
-1.51636436532049));
#44901=CARTESIAN_POINT('Ctrl Pts',(-2.29233862831246,-19.7633934519586,
-1.54579440365611));
#44902=CARTESIAN_POINT('Ctrl Pts',(-2.12998975108742,-19.7622721663513,
-1.57542906499829));
#44903=CARTESIAN_POINT('Ctrl Pts',(-1.97261303665365,-19.7613206253537,
-1.60099901719817));
#44904=CARTESIAN_POINT('Ctrl Pts',(-1.82041652058115,-19.7605131854738,
-1.62304689261556));
#44905=CARTESIAN_POINT('Ctrl Pts',(-1.76985268919714,-19.7602449319356,
-1.63037179783514));
#44906=CARTESIAN_POINT('Ctrl Pts',(-1.71986020171909,-19.7599925807726,
-1.63730784898285));
#44907=CARTESIAN_POINT('Ctrl Pts',(-1.67044548267176,-19.7597551865412,
-1.64387459616671));
#44908=CARTESIAN_POINT('Ctrl Pts',(-1.52120349901276,-19.7590382101689,
-1.66370743939237));
#44909=CARTESIAN_POINT('Ctrl Pts',(-1.37723517551391,-19.7584576260427,
-1.6801737259978));
#44910=CARTESIAN_POINT('Ctrl Pts',(-1.23869613188679,-19.757987037978,-1.69381367693242));
#44911=CARTESIAN_POINT('Ctrl Pts',(-1.14905168103962,-19.7576825345865,
-1.70263967918495));
#44912=CARTESIAN_POINT('Ctrl Pts',(-1.06167946637608,-19.7574240937746,
-1.71028177339375));
#44913=CARTESIAN_POINT('Ctrl Pts',(-0.976611993859875,-19.7572047093365,
-1.71687997626486));
#44914=CARTESIAN_POINT('Ctrl Pts',(-0.844717359987299,-19.756864560167,
-1.72711029728134));
#44915=CARTESIAN_POINT('Ctrl Pts',(-0.718364957082741,-19.7566182850543,
-1.73483337531946));
#44916=CARTESIAN_POINT('Ctrl Pts',(-0.597648913556363,-19.756441381481,
-1.74055570107211));
#44917=CARTESIAN_POINT('Ctrl Pts',(-0.48095024269112,-19.7562703651746,
-1.74608759053837));
#44918=CARTESIAN_POINT('Ctrl Pts',(-0.369518421291674,-19.7561641579339,
-1.74974956680164));
#44919=CARTESIAN_POINT('Ctrl Pts',(-0.263409266590326,-19.7561013445667,
-1.75196333668237));
#44920=CARTESIAN_POINT('Ctrl Pts',(-0.255798651790982,-19.756096839316,
-1.75212211798511));
#44921=CARTESIAN_POINT('Ctrl Pts',(-0.248215408177043,-19.7560925576963,
-1.75227343376927));
#44922=CARTESIAN_POINT('Ctrl Pts',(-0.240659551508548,-19.7560884920149,
-1.75241743246341));
#44923=CARTESIAN_POINT('Ctrl Pts',(-0.202148470861223,-19.7560677698397,
-1.75315137244754));
#44924=CARTESIAN_POINT('Ctrl Pts',(-0.164348875388144,-19.7560526530864,
-1.75369529114276));
#44925=CARTESIAN_POINT('Ctrl Pts',(-0.127262578344625,-19.7560420066296,
-1.75406887712268));
#44926=CARTESIAN_POINT('Ctrl Pts',(-0.105081272439121,-19.7560356389862,
-1.7542923188131));
#44927=CARTESIAN_POINT('Ctrl Pts',(-0.0831551352012425,-19.7560308625404,
-1.75445481924016));
#44928=CARTESIAN_POINT('Ctrl Pts',(-0.0614844746947158,-19.7560274564565,
-1.7545604529612));
#44929=CARTESIAN_POINT('Ctrl Pts',(-0.0416881516813964,-19.7560243449713,
-1.75465695021666));
#44930=CARTESIAN_POINT('Ctrl Pts',(-0.0231003093163219,-19.7560224629351,
-1.75470532598937));
#44931=CARTESIAN_POINT('Ctrl Pts',(-0.0029935776222741,-19.7560213813544,
-1.75471055955774));
#44932=CARTESIAN_POINT('Ctrl Pts',(-0.00108985029600973,-19.7560212789491,
-1.75471105507771));
#44933=CARTESIAN_POINT('Ctrl Pts',(0.000827493160234799,-19.7560211858688,
-1.75471112543437));
#44934=CARTESIAN_POINT('Ctrl Pts',(0.00276076763666115,-19.7560211031285,
-1.75471075018705));
#44935=CARTESIAN_POINT('Ctrl Pts',(0.115380441349963,-19.7560162832307,
-1.75468889078143));
#44936=CARTESIAN_POINT('Ctrl Pts',(0.233554088058695,-19.7560516460445,
-1.75316472129386));
#44937=CARTESIAN_POINT('Ctrl Pts',(0.35722758239336,-19.7561526828529,-1.74966567156876));
#44938=CARTESIAN_POINT('Ctrl Pts',(0.400683612468718,-19.7561881848706,
-1.74843618572859));
#44939=CARTESIAN_POINT('Ctrl Pts',(0.444818431363851,-19.756231813793,-1.74696248033964));
#44940=CARTESIAN_POINT('Ctrl Pts',(0.489628808892576,-19.756284734668,-1.74522279165275));
#44941=CARTESIAN_POINT('Ctrl Pts',(0.616894590528152,-19.7564350350423,
-1.74028190847459));
#44942=CARTESIAN_POINT('Ctrl Pts',(0.749612277410095,-19.7566602638825,
-1.73319794676817));
#44943=CARTESIAN_POINT('Ctrl Pts',(0.887682915219207,-19.756985291486,-1.72346286287803));
#44944=CARTESIAN_POINT('Ctrl Pts',(0.982201834953153,-19.7572077954047,
-1.71679852332389));
#44945=CARTESIAN_POINT('Ctrl Pts',(1.0792286314599,-19.7574770829128,-1.70889105456743));
#44946=CARTESIAN_POINT('Ctrl Pts',(1.1787205097217,-19.7578012083461,-1.69956860986377));
#44947=CARTESIAN_POINT('Ctrl Pts',(1.32351032467892,-19.7582729057581,-1.68600172312716));
#44948=CARTESIAN_POINT('Ctrl Pts',(1.47352295597801,-19.7588607225255,-1.66943864957755));
#44949=CARTESIAN_POINT('Ctrl Pts',(1.62859652258685,-19.7595906934866,-1.64934494633714));
#44950=CARTESIAN_POINT('Ctrl Pts',(1.68654895278824,-19.7598634904055,-1.64183574306032));
#44951=CARTESIAN_POINT('Ctrl Pts',(1.74520771954632,-19.7601561426315,-1.63383324635661));
#44952=CARTESIAN_POINT('Ctrl Pts',(1.80456261864638,-19.7604700126065,-1.62530885106478));
#44953=CARTESIAN_POINT('Ctrl Pts',(1.96229922867042,-19.7613041271716,-1.60265513189035));
#44954=CARTESIAN_POINT('Ctrl Pts',(2.12495580523365,-19.7622881347575,-1.57631599568825));
#44955=CARTESIAN_POINT('Ctrl Pts',(2.29231727829962,-19.7634467629545,-1.54576502076645));
#44956=CARTESIAN_POINT('Ctrl Pts',(2.31269526472841,-19.7635878378939,-1.54204512429961));
#44957=CARTESIAN_POINT('Ctrl Pts',(2.33314294078153,-19.7637315009022,-1.53826277673018));
#44958=CARTESIAN_POINT('Ctrl Pts',(2.3536598645813,-19.7638777958942,-1.53441702176428));
#44959=CARTESIAN_POINT('Ctrl Pts',(2.36243866162264,-19.7639403927072,-1.53277149718927));
#44960=CARTESIAN_POINT('Ctrl Pts',(2.37123013652142,-19.7640034713866,-1.53111436384921));
#44961=CARTESIAN_POINT('Ctrl Pts',(2.38003425591168,-19.7640670353362,-1.52944554910264));
#44962=CARTESIAN_POINT('Ctrl Pts',(2.44797134134356,-19.7645575272622,-1.5165681215051));
#44963=CARTESIAN_POINT('Ctrl Pts',(2.51666144909491,-19.7650769166499,-1.50299512176215));
#44964=CARTESIAN_POINT('Ctrl Pts',(2.58608847144018,-19.7656267527821,-1.48869322497577));
#44965=CARTESIAN_POINT('Ctrl Pts',(2.62080198261281,-19.7659016708482,-1.48154227658258));
#44966=CARTESIAN_POINT('Ctrl Pts',(2.65569972199575,-19.7661841992526,-1.47420910177566));
#44967=CARTESIAN_POINT('Ctrl Pts',(2.69077952007956,-19.7664745298379,-1.46668955142345));
#44968=CARTESIAN_POINT('Ctrl Pts',(2.70831941912146,-19.7666196951305,-1.46292977624734));
#44969=CARTESIAN_POINT('Ctrl Pts',(2.72590483281955,-19.7667668109062,-1.45912340708514));
#44970=CARTESIAN_POINT('Ctrl Pts',(2.74353548471427,-19.7669159007815,-1.45526992577017));
#44971=CARTESIAN_POINT('Ctrl Pts',(2.75886023000185,-19.7670454912457,-1.45192043988757));
#44972=CARTESIAN_POINT('Ctrl Pts',(2.7756378903939,-19.7671887562763,-1.44822069089754));
#44973=CARTESIAN_POINT('Ctrl Pts',(2.79016868314641,-19.7673139548209,-1.44499062909974));
#44974=CARTESIAN_POINT('Ctrl Pts',(2.79235512412055,-19.7673327933821,-1.4445046033485));
#44975=CARTESIAN_POINT('Ctrl Pts',(2.79449071570788,-19.7673512181178,-1.44402930676067));
#44976=CARTESIAN_POINT('Ctrl Pts',(2.79656287568912,-19.7673691161307,-1.44356762735337));
#44977=CARTESIAN_POINT('Ctrl Pts',(2.81155194714093,-19.7674985822905,-1.44022804658432));
#44978=CARTESIAN_POINT('Ctrl Pts',(2.82653495595638,-19.7676293154915,-1.43686280029191));
#44979=CARTESIAN_POINT('Ctrl Pts',(2.84151182044054,-19.7677613100067,-1.43347196866226));
#44980=CARTESIAN_POINT('Ctrl Pts',(2.98776197929538,-19.7690502459406,-1.40036025392311));
#44981=CARTESIAN_POINT('Ctrl Pts',(3.1334262372296,-19.7704594601723,-1.36480881552503));
#44982=CARTESIAN_POINT('Ctrl Pts',(3.27843755210209,-19.7719832405925,-1.32690025755523));
#44983=CARTESIAN_POINT('Ctrl Pts',(3.40982752551187,-19.7733638878136,-1.29255256249409));
#44984=CARTESIAN_POINT('Ctrl Pts',(3.54068146012917,-19.7748385888251,-1.25626977173964));
#44985=CARTESIAN_POINT('Ctrl Pts',(3.67095575809886,-19.7764027584285,-1.21811749018528));
#44986=CARTESIAN_POINT('Ctrl Pts',(3.78813027867816,-19.7778096424128,-1.18380162458624));
#44987=CARTESIAN_POINT('Ctrl Pts',(3.90483587261737,-19.7792889066611,-1.14797333960089));
#44988=CARTESIAN_POINT('Ctrl Pts',(4.02104510454438,-19.7808368957976,-1.11068244027831));
#44989=CARTESIAN_POINT('Ctrl Pts',(4.12468783511056,-19.7822174902506,-1.07742406168849));
#44990=CARTESIAN_POINT('Ctrl Pts',(4.22793574927265,-19.7836527500369,-1.04300229081));
#44991=CARTESIAN_POINT('Ctrl Pts',(4.33077217731849,-19.785139809244,-1.00745340168723));
#44992=CARTESIAN_POINT('Ctrl Pts',(4.42240217239439,-19.7864648185856,-0.975778395104719));
#44993=CARTESIAN_POINT('Ctrl Pts',(4.51370547672763,-19.787830953176,-0.943208537633732));
#44994=CARTESIAN_POINT('Ctrl Pts',(4.60467210497002,-19.7892359781879,-0.909769871237187));
#44995=CARTESIAN_POINT('Ctrl Pts',(4.68609298330715,-19.7904935643242,-0.879840152602627));
#44996=CARTESIAN_POINT('Ctrl Pts',(4.76724413735086,-19.7917823072661,-0.849214398468669));
#44997=CARTESIAN_POINT('Ctrl Pts',(4.84811962990798,-19.7931004999907,-0.817911356901049));
#44998=CARTESIAN_POINT('Ctrl Pts',(4.92104264859151,-19.7942890750416,-0.789686338259283));
#44999=CARTESIAN_POINT('Ctrl Pts',(4.9937415516435,-19.7955015932102,-0.760910679207981));
#45000=CARTESIAN_POINT('Ctrl Pts',(5.0662128614275,-19.7967368734856,-0.731597969779734));
#45001=CARTESIAN_POINT('Ctrl Pts',(5.13211260417619,-19.7978601407842,-0.704943283720578));
#45002=CARTESIAN_POINT('Ctrl Pts',(5.19782415727909,-19.7990022294067,-0.677844529277353));
#45003=CARTESIAN_POINT('Ctrl Pts',(5.26334554179462,-19.8001626395314,-0.650311508810309));
#45004=CARTESIAN_POINT('Ctrl Pts',(5.32292696860345,-19.8012178506114,-0.62527454330793));
#45005=CARTESIAN_POINT('Ctrl Pts',(5.38235114344313,-19.8022882117576,-0.59987848116738));
#45006=CARTESIAN_POINT('Ctrl Pts',(5.44161694959551,-19.8033743444023,-0.574129876715982));
#45007=CARTESIAN_POINT('Ctrl Pts',(5.495383784581,-19.8043597003516,-0.550770353636422));
#45008=CARTESIAN_POINT('Ctrl Pts',(5.54902027518269,-19.8053580364628,-0.527120674053056));
#45009=CARTESIAN_POINT('Ctrl Pts',(5.60252556055007,-19.8063718996398,-0.503184259300562));
#45010=CARTESIAN_POINT('Ctrl Pts',(5.64725681504635,-19.8072195050956,-0.483173042601675));
#45011=CARTESIAN_POINT('Ctrl Pts',(5.69189636725406,-19.8080779619371,-0.462961418909218));
#45012=CARTESIAN_POINT('Ctrl Pts',(5.73644276371317,-19.8089520713582,-0.442549442047294));
#45013=CARTESIAN_POINT('Ctrl Pts',(-5.843530256023,-19.9729833896359,-0.27559175820976));
#45014=CARTESIAN_POINT('Ctrl Pts',(-3.895686837349,-19.9313480702727,-1.19822011532892));
#45015=CARTESIAN_POINT('Ctrl Pts',(0.0001633689864733,-19.8897495499701,
-2.12096425758541));
#45016=CARTESIAN_POINT('Ctrl Pts',(3.896013575322,-19.9313515592134,-1.19814272318624));
#45017=CARTESIAN_POINT('Ctrl Pts',(5.844020362983,-19.9729938661567,-0.275359601183318));
#45018=CARTESIAN_POINT('Ctrl Pts',(-5.843530256023,-19.2592936008182,-0.803935998277621));
#45019=CARTESIAN_POINT('Ctrl Pts',(-3.895686837349,-19.2409365935521,-1.65690450594922));
#45020=CARTESIAN_POINT('Ctrl Pts',(0.0001633689864733,-19.2238044947448,
-2.51235948357542));
#45021=CARTESIAN_POINT('Ctrl Pts',(3.896013575322,-19.2409380304522,-1.65683275746512));
#45022=CARTESIAN_POINT('Ctrl Pts',(5.844020362983,-19.2592982199189,-0.803721369480543));
#45023=CARTESIAN_POINT('Ctrl Pts',(-5.843530256023,-17.6858136333434,-1.6793983649399));
#45024=CARTESIAN_POINT('Ctrl Pts',(-3.895686837349,-17.747795448815,-2.42360806358736));
#45025=CARTESIAN_POINT('Ctrl Pts',(0.0001633689864733,-17.809230949477,
-3.16660341450187));
#45026=CARTESIAN_POINT('Ctrl Pts',(3.896013575322,-17.7477902961142,-2.4235457472868));
#45027=CARTESIAN_POINT('Ctrl Pts',(5.844020362983,-17.6857980371155,-1.67921110261911));
#45028=CARTESIAN_POINT('Ctrl Pts',(-5.843530256023,-15.0614254644282,-2.34071387947306));
#45029=CARTESIAN_POINT('Ctrl Pts',(-3.895686837349,-15.2991206306984,-3.03320174206706));
#45030=CARTESIAN_POINT('Ctrl Pts',(0.0001633689864732,-15.5368877409607,
-3.72636654307133));
#45031=CARTESIAN_POINT('Ctrl Pts',(3.896013575322,-15.2991006887591,-3.03314360513899));
#45032=CARTESIAN_POINT('Ctrl Pts',(5.844020362983,-15.0613656542058,-2.34053963171711));
#45033=CARTESIAN_POINT('Ctrl Pts',(-5.843530256023,-12.4568668146763,-2.30089092035602));
#45034=CARTESIAN_POINT('Ctrl Pts',(-3.895686837349,-12.8710914025805,-3.06727952800882));
#45035=CARTESIAN_POINT('Ctrl Pts',(0.0001633689864735,-13.2856266664931,
-3.83244208505026));
#45036=CARTESIAN_POINT('Ctrl Pts',(3.896013575322,-12.8710566347918,-3.06721535250531));
#45037=CARTESIAN_POINT('Ctrl Pts',(5.844020362983,-12.4567625851234,-2.30069807725729));
#45038=CARTESIAN_POINT('Ctrl Pts',(-5.843530256023,-10.8186332244494,-1.86224588936189));
#45039=CARTESIAN_POINT('Ctrl Pts',(-3.895686837349,-11.3231463541034,-2.74792371556351));
#45040=CARTESIAN_POINT('Ctrl Pts',(0.0001633689864728,-11.8270563158389,
-3.6358578364456));
#45041=CARTESIAN_POINT('Ctrl Pts',(3.896013575322,-11.3231040903104,-2.74784924300041));
#45042=CARTESIAN_POINT('Ctrl Pts',(5.844020362983,-10.8185062759584,-1.86202303005818));
#45043=CARTESIAN_POINT('Ctrl Pts',(-5.843530256023,-10.0864076157968,-1.57296479340504));
#45044=CARTESIAN_POINT('Ctrl Pts',(-3.895686837349,-10.6220745328126,-2.52887436203661));
#45045=CARTESIAN_POINT('Ctrl Pts',(0.0001633689864728,-11.1575431674059,
-3.48561319739018));
#45046=CARTESIAN_POINT('Ctrl Pts',(3.896013575322,-10.6220296221396,-2.52879411870404));
#45047=CARTESIAN_POINT('Ctrl Pts',(5.844020362983,-10.0862728282186,-1.57272426197469));
#45048=CARTESIAN_POINT('',(-5.73278762856495,-10.3449531567002,-1.71289048058869));
#45049=CARTESIAN_POINT('Ctrl Pts',(-5.73644356953966,-19.8089503607358,
-0.442546999711169));
#45050=CARTESIAN_POINT('Ctrl Pts',(-5.73766037023715,-19.13018257123,-0.921733298671357));
#45051=CARTESIAN_POINT('Ctrl Pts',(-5.73849618481613,-18.393846050701,-1.31839021829628));
#45052=CARTESIAN_POINT('Ctrl Pts',(-5.73940756699886,-16.8491829909953,
-1.92343296233218));
#45053=CARTESIAN_POINT('Ctrl Pts',(-5.73948313453522,-16.0408992766055,
-2.13191056314112));
#45054=CARTESIAN_POINT('Ctrl Pts',(-5.73887402245753,-14.4000963331593,
-2.35028699763758));
#45055=CARTESIAN_POINT('Ctrl Pts',(-5.73818934284347,-13.5675419989661,
-2.35984313733086));
#45056=CARTESIAN_POINT('Ctrl Pts',(-5.73605973646493,-11.9265541666401,
-2.1816928390157));
#45057=CARTESIAN_POINT('Ctrl Pts',(-5.73461480970045,-11.1182366089558,
-1.99332811374448));
#45058=CARTESIAN_POINT('Ctrl Pts',(-5.732787734897,-10.344953053782,-1.71289076302532));
#45059=CARTESIAN_POINT('Ctrl Pts',(5.73278688084627,-10.3449507251019,-1.71289711530792));
#45060=CARTESIAN_POINT('Ctrl Pts',(5.37888843777514,-10.4448706571245,-1.88173932877861));
#45061=CARTESIAN_POINT('Ctrl Pts',(5.01595919747795,-10.5336950032638,-2.03742942677716));
#45062=CARTESIAN_POINT('Ctrl Pts',(4.64561269144281,-10.6118287908983,-2.1782223594122));
#45063=CARTESIAN_POINT('Ctrl Pts',(4.37133529018088,-10.6696944163975,-2.28249314109879));
#45064=CARTESIAN_POINT('Ctrl Pts',(4.09298964122314,-10.7216962259158,-2.37858913369378));
#45065=CARTESIAN_POINT('Ctrl Pts',(3.81123116921486,-10.7680223059877,-2.46581531638881));
#45066=CARTESIAN_POINT('Ctrl Pts',(3.57206776142054,-10.8073450035477,-2.53985501057632));
#45067=CARTESIAN_POINT('Ctrl Pts',(3.33044540604648,-10.8425781621285,-2.60750319913259));
#45068=CARTESIAN_POINT('Ctrl Pts',(3.08676494767327,-10.8738590874902,-2.6683687069462));
#45069=CARTESIAN_POINT('Ctrl Pts',(3.04336539559371,-10.8794302283129,-2.67920886948463));
#45070=CARTESIAN_POINT('Ctrl Pts',(2.99990056110183,-10.8848760740909,-2.68983400144025));
#45071=CARTESIAN_POINT('Ctrl Pts',(2.95637270868366,-10.8901974957882,-2.70024205336848));
#45072=CARTESIAN_POINT('Ctrl Pts',(2.75799589931633,-10.9144497067053,-2.74767642052765));
#45073=CARTESIAN_POINT('Ctrl Pts',(2.55830648556141,-10.9361785450978,-2.79061684543243));
#45074=CARTESIAN_POINT('Ctrl Pts',(2.35757129153615,-10.9553635756561,-2.82884755089333));
#45075=CARTESIAN_POINT('Ctrl Pts',(2.16366743985199,-10.9738957086884,-2.86577720379982));
#45076=CARTESIAN_POINT('Ctrl Pts',(1.96878777590427,-10.9900542072394,-2.89831218497539));
#45077=CARTESIAN_POINT('Ctrl Pts',(1.77317279899638,-11.0038443119457,-2.92629994189379));
#45078=CARTESIAN_POINT('Ctrl Pts',(1.58064315056598,-11.0174169128421,-2.95384626316751));
#45079=CARTESIAN_POINT('Ctrl Pts',(1.38740120163293,-11.0286951687085,-2.97698752542344));
#45080=CARTESIAN_POINT('Ctrl Pts',(1.19367625025074,-11.0377081848305,-2.99562128171204));
#45081=CARTESIAN_POINT('Ctrl Pts',(0.99541937006976,-11.0469320480686,-3.01469094910115));
#45082=CARTESIAN_POINT('Ctrl Pts',(0.796656624754899,-11.0537832045303,
-3.02903930284969));
#45083=CARTESIAN_POINT('Ctrl Pts',(0.597633784091129,-11.058320922494,-3.03860683125552));
#45084=CARTESIAN_POINT('Ctrl Pts',(0.408899185061013,-11.0626240686934,
-3.04767977801561));
#45085=CARTESIAN_POINT('Ctrl Pts',(0.219930686263253,-11.0648468971938,
-3.05245361771812));
#45086=CARTESIAN_POINT('Ctrl Pts',(0.0309378795019422,-11.0650651874903,
-3.05292291655167));
#45087=CARTESIAN_POINT('Ctrl Pts',(0.0206355625289282,-11.0650770868629,
-3.0529484988234));
#45088=CARTESIAN_POINT('Ctrl Pts',(0.010333173324214,-11.0650830359869,
-3.05296130133743));
#45089=CARTESIAN_POINT('Ctrl Pts',(3.07458380650083E-5,-11.0650830493252,
-3.05296132714325));
#45090=CARTESIAN_POINT('Ctrl Pts',(2.04972257753908E-5,-11.0650830493385,
-3.05296132716893));
#45091=CARTESIAN_POINT('Ctrl Pts',(1.02486135232418E-5,-11.0650830493459,
-3.05296132718195));
#45092=CARTESIAN_POINT('Ctrl Pts',(1.30820925200369E-12,-11.0650830493474,
-3.05296132718234));
#45093=CARTESIAN_POINT('Ctrl Pts',(-0.189346238011998,-11.0650830774452,
-3.05296133427582));
#45094=CARTESIAN_POINT('Ctrl Pts',(-0.378679741028174,-11.0630759761256,
-3.04864178284235));
#45095=CARTESIAN_POINT('Ctrl Pts',(-0.56778974481848,-11.0589841641667,
-3.04000565563741));
#45096=CARTESIAN_POINT('Ctrl Pts',(-0.769206894826438,-11.0546260599597,
-3.0308074953399));
#45097=CARTESIAN_POINT('Ctrl Pts',(-0.970370508673635,-11.0479028812665,
-3.01671229737493));
#45098=CARTESIAN_POINT('Ctrl Pts',(-1.17102593691553,-11.0387518606635,
-2.99777927914873));
#45099=CARTESIAN_POINT('Ctrl Pts',(-1.36677015451404,-11.0298248189988,
-2.97930966249326));
#45100=CARTESIAN_POINT('Ctrl Pts',(-1.56203075861168,-11.0185875790368,
-2.95623660831183));
#45101=CARTESIAN_POINT('Ctrl Pts',(-1.75657134412065,-11.0050092503527,
-2.9286641524004));
#45102=CARTESIAN_POINT('Ctrl Pts',(-1.95843344700961,-10.9909199024939,
-2.90005400959892));
#45103=CARTESIAN_POINT('Ctrl Pts',(-2.15952031581612,-10.9743099252187,
-2.86659942061579));
#45104=CARTESIAN_POINT('Ctrl Pts',(-2.35956783707536,-10.95517321442,-2.82846728755689));
#45105=CARTESIAN_POINT('Ctrl Pts',(-2.55961535833459,-10.9360365036213,
-2.79033515449799));
#45106=CARTESIAN_POINT('Ctrl Pts',(-2.75862353204654,-10.9143732358628,
-2.74752581297736));
#45107=CARTESIAN_POINT('Ctrl Pts',(-2.95632824474637,-10.8902036689342,
-2.70025289298462));
#45108=CARTESIAN_POINT('Ctrl Pts',(-3.19895907619652,-10.8605418463119,
-2.64223774642446));
#45109=CARTESIAN_POINT('Ctrl Pts',(-3.4396322657691,-10.8270117264881,-2.57747376778623));
#45110=CARTESIAN_POINT('Ctrl Pts',(-3.67795557690252,-10.7894741500217,
-2.50633569808409));
#45111=CARTESIAN_POINT('Ctrl Pts',(-3.96305364831295,-10.7445692239988,
-2.42123564480148));
#45112=CARTESIAN_POINT('Ctrl Pts',(-4.24478892074166,-10.6939295124197,
-2.32701475039204));
#45113=CARTESIAN_POINT('Ctrl Pts',(-4.52248991688278,-10.6373573471668,
-2.22437826455121));
#45114=CARTESIAN_POINT('Ctrl Pts',(-4.88935807875883,-10.5626203942278,
-2.08878617296681));
#45115=CARTESIAN_POINT('Ctrl Pts',(-5.24918529793651,-10.4775301564684,
-1.93851281801485));
#45116=CARTESIAN_POINT('Ctrl Pts',(-5.60042336716264,-10.3816929767705,
-1.77523602709409));
#45117=CARTESIAN_POINT('Ctrl Pts',(-5.64468291353218,-10.3696165235885,
-1.7546615013465));
#45118=CARTESIAN_POINT('Ctrl Pts',(-5.68880607668191,-10.3573694769593,
-1.73388045298063));
#45119=CARTESIAN_POINT('Ctrl Pts',(-5.73278975886993,-10.3449510884867,
-1.71289616972921));
#45120=CARTESIAN_POINT('Ctrl Pts',(5.84410998923895,-10.3323727011903,-1.66672064035875));
#45121=CARTESIAN_POINT('Ctrl Pts',(5.36057054894098,-10.479094582877,-1.90463347330094));
#45122=CARTESIAN_POINT('Ctrl Pts',(4.31408846255943,-10.7396037440786,-2.34942232840999));
#45123=CARTESIAN_POINT('Ctrl Pts',(2.64209705711627,-10.9963179139186,-2.82821487492597));
#45124=CARTESIAN_POINT('Ctrl Pts',(0.886920055989066,-11.1223996222838,
-3.07899637167777));
#45125=CARTESIAN_POINT('Ctrl Pts',(-0.875886341835384,-11.1227843119789,
-3.07977938393283));
#45126=CARTESIAN_POINT('Ctrl Pts',(-2.63119909167307,-10.9975191925275,
-2.83055183922051));
#45127=CARTESIAN_POINT('Ctrl Pts',(-4.30720311490177,-10.741126078388,-2.35211597616156));
#45128=CARTESIAN_POINT('Ctrl Pts',(-5.35738264311282,-10.4800665124644,
-1.90620695928531));
#45129=CARTESIAN_POINT('Ctrl Pts',(-5.8442271457114,-10.3323372091642,-1.66666302689571));
#45130=CARTESIAN_POINT('Ctrl Pts',(5.72541417918007,-10.0514442779705,-1.59501843129042));
#45131=CARTESIAN_POINT('Ctrl Pts',(5.25159834165599,-10.1957394661812,-1.82634278489692));
#45132=CARTESIAN_POINT('Ctrl Pts',(4.2261913450166,-10.4520386787258,-2.25899782340991));
#45133=CARTESIAN_POINT('Ctrl Pts',(2.58809547397256,-10.7047345563918,-2.72492011022138));
#45134=CARTESIAN_POINT('Ctrl Pts',(0.868755502373261,-10.8288843404259,
-2.96899426302417));
#45135=CARTESIAN_POINT('Ctrl Pts',(-0.857947639815771,-10.8292631798881,
-2.96975634944105));
#45136=CARTESIAN_POINT('Ctrl Pts',(-2.57741930712446,-10.705917294703,-2.72719450177864));
#45137=CARTESIAN_POINT('Ctrl Pts',(-4.21944479726212,-10.453536763772,-2.26161858227183));
#45138=CARTESIAN_POINT('Ctrl Pts',(-5.24847453496336,-10.1966953253984,
-1.82787271391779));
#45139=CARTESIAN_POINT('Ctrl Pts',(-5.72552897853899,-10.0514093727704,
-1.59496241647954));
#45140=CARTESIAN_POINT('Ctrl Pts',(5.71947389187913,-9.77852708496778,-1.74874490072951));
#45141=CARTESIAN_POINT('Ctrl Pts',(5.2470321869844,-9.921413239911,-1.97762113018203));
#45142=CARTESIAN_POINT('Ctrl Pts',(4.22431639454507,-10.1753945595949,-2.4060661741839));
#45143=CARTESIAN_POINT('Ctrl Pts',(2.5884933514872,-10.426209475828,-2.86836631045969));
#45144=CARTESIAN_POINT('Ctrl Pts',(0.869223760158633,-10.5496122855385,
-3.11097295137889));
#45145=CARTESIAN_POINT('Ctrl Pts',(-0.858411199827123,-10.5499890570998,
-3.11173099225105));
#45146=CARTESIAN_POINT('Ctrl Pts',(-2.57782411118657,-10.4273844882945,
-2.87062553047234));
#45147=CARTESIAN_POINT('Ctrl Pts',(-4.21758631945515,-10.1768799198358,
-2.40866315092365));
#45148=CARTESIAN_POINT('Ctrl Pts',(-5.24391750487453,-9.92235978674762,
-1.97913477439047));
#45149=CARTESIAN_POINT('Ctrl Pts',(-5.71958836908387,-9.77849251905957,
-1.74868947153473));
#45150=CARTESIAN_POINT('Ctrl Pts',(5.83013871823063,-9.69045696047479,-2.02829469174308));
#45151=CARTESIAN_POINT('Ctrl Pts',(5.34983126658624,-9.83386472624641,-2.26044942827995));
#45152=CARTESIAN_POINT('Ctrl Pts',(4.30967893787492,-10.0889220899972,-2.69533619417949));
#45153=CARTESIAN_POINT('Ctrl Pts',(2.64303317634597,-10.3412121496862,-3.16560929890304));
#45154=CARTESIAN_POINT('Ctrl Pts',(0.888021522624684,-10.4655369409606,
-3.41293915743986));
#45155=CARTESIAN_POINT('Ctrl Pts',(-0.876976757826566,-10.4659167668583,
-3.41371265444607));
#45156=CARTESIAN_POINT('Ctrl Pts',(-2.63215150136536,-10.3423952567662,
-3.16791057917455));
#45157=CARTESIAN_POINT('Ctrl Pts',(-4.30283233414894,-10.0904144949512,
-2.69797390537513));
#45158=CARTESIAN_POINT('Ctrl Pts',(-5.34666482197009,-9.83481475265889,
-2.26198461166413));
#45159=CARTESIAN_POINT('Ctrl Pts',(-5.8302551169916,-9.6904222664813,-2.02823845567536));
#45160=CARTESIAN_POINT('',(-5.72001850098467,-9.72697711277114,-2.05943260735066));
#45161=CARTESIAN_POINT('Origin',(-5.89877516387283,-10.1838115204741,-2.15616245823881));
#45162=CARTESIAN_POINT('Ctrl Pts',(5.72001565651808,-9.72697714714131,-2.05943442901332));
#45163=CARTESIAN_POINT('Ctrl Pts',(5.52235085864605,-9.7844910448374,-2.15308157960336));
#45164=CARTESIAN_POINT('Ctrl Pts',(5.32001672263882,-9.83893941594344,-2.2434991590881));
#45165=CARTESIAN_POINT('Ctrl Pts',(5.11307319479122,-9.89023368154803,-2.33012652189619));
#45166=CARTESIAN_POINT('Ctrl Pts',(4.91024846415452,-9.94050703734063,-2.41502974022856));
#45167=CARTESIAN_POINT('Ctrl Pts',(4.70299587527167,-9.98775055604259,-2.49629215637547));
#45168=CARTESIAN_POINT('Ctrl Pts',(4.49139522432464,-10.0318777162878,-2.57334139085351));
#45169=CARTESIAN_POINT('Ctrl Pts',(4.46219526166272,-10.0379670710501,-2.58397384760551));
#45170=CARTESIAN_POINT('Ctrl Pts',(4.43291253856575,-10.0439970772018,-2.59452600233919));
#45171=CARTESIAN_POINT('Ctrl Pts',(4.40354730271865,-10.0499675032233,-2.60499628183089));
#45172=CARTESIAN_POINT('Ctrl Pts',(4.37976748661062,-10.0548023233356,-2.61347506000958));
#45173=CARTESIAN_POINT('Ctrl Pts',(4.35593367343142,-10.0595979810214,-2.62190037307499));
#45174=CARTESIAN_POINT('Ctrl Pts',(4.332045973406,-10.0643543153132,-2.63027154851775));
#45175=CARTESIAN_POINT('Ctrl Pts',(4.12525023380215,-10.1055298854443,-2.70274078646022));
#45176=CARTESIAN_POINT('Ctrl Pts',(3.91441507757712,-10.1437589609266,-2.77115658712805));
#45177=CARTESIAN_POINT('Ctrl Pts',(3.69967486042235,-10.1789388853645,-2.83506100053878));
#45178=CARTESIAN_POINT('Ctrl Pts',(3.57990205462159,-10.1985607257148,-2.87070411852882));
#45179=CARTESIAN_POINT('Ctrl Pts',(3.45891509144413,-10.2172332521504,-2.9049447655403));
#45180=CARTESIAN_POINT('Ctrl Pts',(3.33674283377924,-10.2349335320187,-2.93770859495658));
#45181=CARTESIAN_POINT('Ctrl Pts',(3.27565670494679,-10.2437836719529,-2.95409050966471));
#45182=CARTESIAN_POINT('Ctrl Pts',(3.21427424700828,-10.2523907260036,-2.97010321289942));
#45183=CARTESIAN_POINT('Ctrl Pts',(3.15259957222235,-10.2607514410604,-2.98573783030413));
#45184=CARTESIAN_POINT('Ctrl Pts',(3.11638891678785,-10.2656602139588,-2.99491728273994));
#45185=CARTESIAN_POINT('Ctrl Pts',(3.07933300787028,-10.2705825379318,-3.00415159974981));
#45186=CARTESIAN_POINT('Ctrl Pts',(3.04274299872612,-10.2753423983666,-3.01310965170823));
#45187=CARTESIAN_POINT('Ctrl Pts',(3.01701221065459,-10.2786896224576,-3.01940912366429));
#45188=CARTESIAN_POINT('Ctrl Pts',(2.99151215360445,-10.2819570769124,-3.02557289989933));
#45189=CARTESIAN_POINT('Ctrl Pts',(2.96670303692837,-10.2850912093338,-3.0314985776476));
#45190=CARTESIAN_POINT('Ctrl Pts',(2.85030963482703,-10.2997951723937,-3.05929923665065));
#45191=CARTESIAN_POINT('Ctrl Pts',(2.73340197420777,-10.3135879903048,-3.08554917027159));
#45192=CARTESIAN_POINT('Ctrl Pts',(2.61601284445959,-10.3264799707405,-3.11020526841202));
#45193=CARTESIAN_POINT('Ctrl Pts',(2.35525340215346,-10.3551172528793,-3.1649744826854));
#45194=CARTESIAN_POINT('Ctrl Pts',(2.09211887583113,-10.3793110921927,-3.21188228216435));
#45195=CARTESIAN_POINT('Ctrl Pts',(1.8270977264198,-10.3991227910425,-3.25060580697337));
#45196=CARTESIAN_POINT('Ctrl Pts',(1.56723131899066,-10.4185491463224,-3.28857614744417));
#45197=CARTESIAN_POINT('Ctrl Pts',(1.30555044492713,-10.4337620611484,-3.31867769380861));
#45198=CARTESIAN_POINT('Ctrl Pts',(1.04251007652366,-10.4447978734305,-3.34056109478048));
#45199=CARTESIAN_POINT('Ctrl Pts',(0.985615250304729,-10.4471848858339,
-3.34529440740063));
#45200=CARTESIAN_POINT('Ctrl Pts',(0.928656816677235,-10.4493763974219,
-3.34964306254167));
#45201=CARTESIAN_POINT('Ctrl Pts',(0.871639381436839,-10.4513726478619,
-3.35360322592787));
#45202=CARTESIAN_POINT('Ctrl Pts',(0.606372392652728,-10.4606599709564,
-3.37202742568577));
#45203=CARTESIAN_POINT('Ctrl Pts',(0.339827581630843,-10.4657227545967,
-3.38204643130129));
#45204=CARTESIAN_POINT('Ctrl Pts',(0.0725412991722131,-10.4664986079721,
-3.38358403303145));
#45205=CARTESIAN_POINT('Ctrl Pts',(0.0484382047896898,-10.4665685721579,
-3.38372268945363));
#45206=CARTESIAN_POINT('Ctrl Pts',(0.0243290882578963,-10.4666036600148,
-3.38379234520509));
#45207=CARTESIAN_POINT('Ctrl Pts',(0.000214347814518571,-10.4666038166003,
-3.38379292606275));
#45208=CARTESIAN_POINT('Ctrl Pts',(-0.260553342450019,-10.4666055098569,
-3.38379920723792));
#45209=CARTESIAN_POINT('Ctrl Pts',(-0.520633949551103,-10.4625144980462,
-3.3757628994388));
#45210=CARTESIAN_POINT('Ctrl Pts',(-0.779551934798321,-10.4544007225929,
-3.35973491714526));
#45211=CARTESIAN_POINT('Ctrl Pts',(-0.806643725132065,-10.4535517406144,
-3.35805783497827));
#45212=CARTESIAN_POINT('Ctrl Pts',(-0.833722790373814,-10.452658694736,
-3.35629321491924));
#45213=CARTESIAN_POINT('Ctrl Pts',(-0.860788587592884,-10.4517216503606,
-3.35444108617536));
#45214=CARTESIAN_POINT('Ctrl Pts',(-1.07488422032283,-10.4443094501276,
-3.33979039356473));
#45215=CARTESIAN_POINT('Ctrl Pts',(-1.28814982980102,-10.434145049339,-3.31966611688754));
#45216=CARTESIAN_POINT('Ctrl Pts',(-1.50035118319147,-10.4212166860301,
-3.29424753095549));
#45217=CARTESIAN_POINT('Ctrl Pts',(-1.74805547483542,-10.4061253069018,
-3.26457621773205));
#45218=CARTESIAN_POINT('Ctrl Pts',(-1.99429862023719,-10.3872816790159,
-3.22765205927763));
#45219=CARTESIAN_POINT('Ctrl Pts',(-2.238704824599,-10.3646346324663,-3.18377136192204));
#45220=CARTESIAN_POINT('Ctrl Pts',(-2.36090792677991,-10.3533111091916,
-3.16183101324425));
#45221=CARTESIAN_POINT('Ctrl Pts',(-2.48265212251779,-10.3410357106285,
-3.13815307827137));
#45222=CARTESIAN_POINT('Ctrl Pts',(-2.60389237049849,-10.3277960057427,
-3.11278377543351));
#45223=CARTESIAN_POINT('Ctrl Pts',(-2.60428195105617,-10.3277534626788,
-3.1127022564057));
#45224=CARTESIAN_POINT('Ctrl Pts',(-2.60467152641047,-10.3277109096566,
-3.11262071991405));
#45225=CARTESIAN_POINT('Ctrl Pts',(-2.6050610965595,-10.3276683466758,-3.11253916595973));
#45226=CARTESIAN_POINT('Ctrl Pts',(-2.66529003077652,-10.3210879580644,
-3.09993063380649));
#45227=CARTESIAN_POINT('Ctrl Pts',(-2.72539454793682,-10.3142695391852,
-3.08690471014164));
#45228=CARTESIAN_POINT('Ctrl Pts',(-2.7853693764555,-10.3072116618264,-3.07346790953369));
#45229=CARTESIAN_POINT('Ctrl Pts',(-2.82091266841363,-10.3030289037967,
-3.06550476668215));
#45230=CARTESIAN_POINT('Ctrl Pts',(-2.85565628250159,-10.2988530195494,
-3.05757010167284));
#45231=CARTESIAN_POINT('Ctrl Pts',(-2.89093226624542,-10.2945248100442,
-3.04936312181237));
#45232=CARTESIAN_POINT('Ctrl Pts',(-2.91556507117471,-10.2915024722065,
-3.04363228421391));
#45233=CARTESIAN_POINT('Ctrl Pts',(-2.94045720811709,-10.2884053612001,
-3.03776780035864));
#45234=CARTESIAN_POINT('Ctrl Pts',(-2.96605816588864,-10.2851718529285,
-3.03165480338706));
#45235=CARTESIAN_POINT('Ctrl Pts',(-3.20039906137285,-10.2555736156018,
-2.97569888184707));
#45236=CARTESIAN_POINT('Ctrl Pts',(-3.43065223281089,-10.2224787982665,
-2.91412948280924));
#45237=CARTESIAN_POINT('Ctrl Pts',(-3.65662486529341,-10.1860042939441,
-2.84757563479633));
#45238=CARTESIAN_POINT('Ctrl Pts',(-3.88259749777593,-10.1495297896217,
-2.78102178678342));
#45239=CARTESIAN_POINT('Ctrl Pts',(-4.10428974370387,-10.1096756491821,
-2.70948313380135));
#45240=CARTESIAN_POINT('Ctrl Pts',(-4.32153106765576,-10.0665548789947,
-2.63353231928838));
#45241=CARTESIAN_POINT('Ctrl Pts',(-4.53975694790682,-10.0232386817811,
-2.55723728917454));
#45242=CARTESIAN_POINT('Ctrl Pts',(-4.75349214138674,-9.97662627109529,
-2.47648978122073));
#45243=CARTESIAN_POINT('Ctrl Pts',(-4.96264794993634,-9.92683360298108,
-2.39182310253517));
#45244=CARTESIAN_POINT('Ctrl Pts',(-5.1769245871331,-9.8758218450263,-2.30508350243911));
#45245=CARTESIAN_POINT('Ctrl Pts',(-5.38639491591567,-9.82147223720818,
-2.21423036493514));
#45246=CARTESIAN_POINT('Ctrl Pts',(-5.59097678902522,-9.76390332624704,
-2.11978463387151));
#45247=CARTESIAN_POINT('Ctrl Pts',(-5.63420911728029,-9.75173783954908,
-2.09982632189806));
#45248=CARTESIAN_POINT('Ctrl Pts',(-5.67722318912536,-9.73942856815475,
-2.0797073988229));
#45249=CARTESIAN_POINT('Ctrl Pts',(-5.72001829824668,-9.72697659463366,
-2.05943249764344));
#45250=CARTESIAN_POINT('Ctrl Pts',(-5.71222662189986,-10.3742949004598,
-1.73071937901633));
#45251=CARTESIAN_POINT('Ctrl Pts',(-5.71815984095385,-10.3724589996086,
-1.7282869964701));
#45252=CARTESIAN_POINT('Ctrl Pts',(-5.76567964049473,-10.3578830041957,
-1.70774113544913));
#45253=CARTESIAN_POINT('Ctrl Pts',(-5.85049323787678,-10.3338145218821,
-1.65484483353384));
#45254=CARTESIAN_POINT('Ctrl Pts',(-5.948215668862,-10.3109877388706,-1.55199932393069));
#45255=CARTESIAN_POINT('Ctrl Pts',(-6.01635745652966,-10.3007577513163,
-1.43124311968169));
#45256=CARTESIAN_POINT('Ctrl Pts',(-6.04741510867493,-10.3028711449483,
-1.31838657229349));
#45257=CARTESIAN_POINT('Ctrl Pts',(-6.0513323381477,-10.309530687115,-1.25061757017122));
#45258=CARTESIAN_POINT('Ctrl Pts',(-6.05059138821606,-10.3129418468683,
-1.22449919891673));
#45259=CARTESIAN_POINT('Ctrl Pts',(-5.59627044501229,-10.0908844432555,
-1.65483230450451));
#45260=CARTESIAN_POINT('Ctrl Pts',(-5.60180878284993,-10.0891580404173,
-1.65259441346381));
#45261=CARTESIAN_POINT('Ctrl Pts',(-5.64617398194355,-10.0754418826971,
-1.63369069961307));
#45262=CARTESIAN_POINT('Ctrl Pts',(-5.72546143917485,-10.0526570805557,
-1.58500246675733));
#45263=CARTESIAN_POINT('Ctrl Pts',(-5.81681904905107,-10.0308016578564,
-1.49039287045747));
#45264=CARTESIAN_POINT('Ctrl Pts',(-5.88036941811923,-10.0207355017336,
-1.37963866786923));
#45265=CARTESIAN_POINT('Ctrl Pts',(-5.90916535585768,-10.0223138650847,
-1.27675997058527));
#45266=CARTESIAN_POINT('Ctrl Pts',(-5.91275807104277,-10.0282885033146,
-1.21550396072571));
#45267=CARTESIAN_POINT('Ctrl Pts',(-5.91207749740188,-10.0313688521514,
-1.19199294725519));
#45268=CARTESIAN_POINT('Ctrl Pts',(-5.57929439471514,-9.81899473911404,
-1.81393819386833));
#45269=CARTESIAN_POINT('Ctrl Pts',(-5.58716647012282,-9.81658670486357,
-1.81078351792171));
#45270=CARTESIAN_POINT('Ctrl Pts',(-5.6501538878883,-9.79750079182511,-1.78417128597669));
#45271=CARTESIAN_POINT('Ctrl Pts',(-5.76178553763288,-9.76641565551527,
-1.71622516352867));
#45272=CARTESIAN_POINT('Ctrl Pts',(-5.89038954782538,-9.73728669160811,
-1.58467249327706));
#45273=CARTESIAN_POINT('Ctrl Pts',(-5.98122469506971,-9.72430629345384,
-1.42882521019155));
#45274=CARTESIAN_POINT('Ctrl Pts',(-6.02390479158533,-9.72723646949882,
-1.27974174396812));
#45275=CARTESIAN_POINT('Ctrl Pts',(-6.02958496996387,-9.73632704949079,
-1.18718217071838));
#45276=CARTESIAN_POINT('Ctrl Pts',(-6.02851816949953,-9.7410542982751,-1.15093231856939));
#45277=CARTESIAN_POINT('Ctrl Pts',(-5.67241100352444,-9.73660671891414,
-2.10388493024505));
#45278=CARTESIAN_POINT('Ctrl Pts',(-5.68381775092394,-9.73317212551118,
-2.09930232818442));
#45279=CARTESIAN_POINT('Ctrl Pts',(-5.77501394452402,-9.70600195136843,
-2.06067697444542));
#45280=CARTESIAN_POINT('Ctrl Pts',(-5.93568733722006,-9.66246593541034,
-1.96261338233826));
#45281=CARTESIAN_POINT('Ctrl Pts',(-6.12076716020052,-9.62257985011687,
-1.77312190199155));
#45282=CARTESIAN_POINT('Ctrl Pts',(-6.25290243570567,-9.60551482359818,
-1.54660477105814));
#45283=CARTESIAN_POINT('Ctrl Pts',(-6.31652387643652,-9.61079874693495,
-1.32537995208573));
#45284=CARTESIAN_POINT('Ctrl Pts',(-6.32533702444869,-9.62476639236188,
-1.18419183869603));
#45285=CARTESIAN_POINT('Ctrl Pts',(-6.32369022138811,-9.63204017725459,
-1.12819590352899));
#45286=CARTESIAN_POINT('',(-5.99998760030264,-10.0933467246824,-1.2110347037336));
#45287=CARTESIAN_POINT('',(-5.99999999751865,-9.65438795558276,-1.86247663369286));
#45288=CARTESIAN_POINT('Ctrl Pts',(-5.99998760030264,-10.0933467246824,
-1.2110347037336));
#45289=CARTESIAN_POINT('Ctrl Pts',(-5.99998607316774,-10.0742396970364,
-1.22560749002239));
#45290=CARTESIAN_POINT('Ctrl Pts',(-5.99998812583008,-10.0554931562148,
-1.24050908229297));
#45291=CARTESIAN_POINT('Ctrl Pts',(-6.00000075483295,-10.0372227691589,
-1.25574669535911));
#45292=CARTESIAN_POINT('Ctrl Pts',(-6.0000066757416,-10.0286569865797,-1.26289060972449));
#45293=CARTESIAN_POINT('Ctrl Pts',(-6.00001433938093,-10.0201958451556,
-1.27010784300164));
#45294=CARTESIAN_POINT('Ctrl Pts',(-6.00002217201098,-10.0118507476806,
-1.27739604002589));
#45295=CARTESIAN_POINT('Ctrl Pts',(-6.00003978018608,-9.99309051815821,
-1.29378030029239));
#45296=CARTESIAN_POINT('Ctrl Pts',(-6.00006006509509,-9.97491795491863,
-1.31052619883873));
#45297=CARTESIAN_POINT('Ctrl Pts',(-6.00008124713978,-9.95743900268535,
-1.32757773999911));
#45298=CARTESIAN_POINT('Ctrl Pts',(-6.0000957515782,-9.94547026264922,-1.33925380963076));
#45299=CARTESIAN_POINT('Ctrl Pts',(-6.00010993220736,-9.93382646569235,
-1.35107215192216));
#45300=CARTESIAN_POINT('Ctrl Pts',(-6.00011973283796,-9.92253515906925,
-1.36300284494533));
#45301=CARTESIAN_POINT('Ctrl Pts',(-6.00013439162104,-9.90564677491764,
-1.38084755802381));
#45302=CARTESIAN_POINT('Ctrl Pts',(-6.0001381190075,-9.88954895530081,-1.3989450314351));
#45303=CARTESIAN_POINT('Ctrl Pts',(-6.00012272533991,-9.87430471235906,
-1.41716232741016));
#45304=CARTESIAN_POINT('Ctrl Pts',(-6.00011846686318,-9.87008757219817,
-1.42220192765615));
#45305=CARTESIAN_POINT('Ctrl Pts',(-6.00011283313294,-9.86593553105825,
-1.42725050321475));
#45306=CARTESIAN_POINT('Ctrl Pts',(-6.00010589287417,-9.86184939866626,
-1.4323048409796));
#45307=CARTESIAN_POINT('Ctrl Pts',(-6.00010021774545,-9.85850812162791,
-1.43643783058878));
#45308=CARTESIAN_POINT('Ctrl Pts',(-6.00009367301605,-9.85521090958835,
-1.44057467085351));
#45309=CARTESIAN_POINT('Ctrl Pts',(-6.00008646895637,-9.85195805011668,
-1.44471365554858));
#45310=CARTESIAN_POINT('Ctrl Pts',(-6.00006816383533,-9.84369271237293,
-1.45523058894793));
#45311=CARTESIAN_POINT('Ctrl Pts',(-6.00005083454579,-9.83559537668922,
-1.46590386806272));
#45312=CARTESIAN_POINT('Ctrl Pts',(-6.00003062833731,-9.82781143086467,
-1.47654974030866));
#45313=CARTESIAN_POINT('Ctrl Pts',(-6.00001023986008,-9.81995727047922,
-1.48729164293069));
#45314=CARTESIAN_POINT('Ctrl Pts',(-5.99998647027655,-9.81242254560712,
-1.49800526520946));
#45315=CARTESIAN_POINT('Ctrl Pts',(-5.99996841664569,-9.80532177884617,
-1.5084628178353));
#45316=CARTESIAN_POINT('Ctrl Pts',(-5.9999575812154,-9.80106003981939,-1.51473923299587));
#45317=CARTESIAN_POINT('Ctrl Pts',(-5.99994910272377,-9.79695390267551,
-1.52092267040456));
#45318=CARTESIAN_POINT('Ctrl Pts',(-5.99994799710813,-9.79302171041628,
-1.52695840218962));
#45319=CARTESIAN_POINT('Ctrl Pts',(-5.99994410063521,-9.77916365692028,
-1.54822986819403));
#45320=CARTESIAN_POINT('Ctrl Pts',(-5.99996403848016,-9.76602534233863,
-1.57001276505637));
#45321=CARTESIAN_POINT('Ctrl Pts',(-5.99998999688529,-9.75374482436451,
-1.59221790778169));
#45322=CARTESIAN_POINT('Ctrl Pts',(-6.00001580522397,-9.74153530049751,
-1.61429468179451));
#45323=CARTESIAN_POINT('Ctrl Pts',(-6.00004684830186,-9.73017447649929,
-1.63678831739194));
#45324=CARTESIAN_POINT('Ctrl Pts',(-6.00006726238211,-9.71976949444447,
-1.65956840215017));
#45325=CARTESIAN_POINT('Ctrl Pts',(-6.00006992719727,-9.71841124789831,
-1.6625420710408));
#45326=CARTESIAN_POINT('Ctrl Pts',(-6.00007242162838,-9.71706923986762,
-1.66552056836441));
#45327=CARTESIAN_POINT('Ctrl Pts',(-6.00007472171134,-9.71574366257339,
-1.66850355851029));
#45328=CARTESIAN_POINT('Ctrl Pts',(-6.00009235696659,-9.70558016221269,
-1.69137481736148));
#45329=CARTESIAN_POINT('Ctrl Pts',(-6.00009751347439,-9.69638600040425,
-1.71451258302224));
#45330=CARTESIAN_POINT('Ctrl Pts',(-6.00008872575521,-9.68822341677773,
-1.73775334468263));
#45331=CARTESIAN_POINT('Ctrl Pts',(-6.00007982866157,-9.67995923929784,
-1.76128336751823));
#45332=CARTESIAN_POINT('Ctrl Pts',(-6.0000562406674,-9.67275278597893,-1.78491795340221));
#45333=CARTESIAN_POINT('Ctrl Pts',(-6.00003365310932,-9.66662223367053,
-1.80846626086191));
#45334=CARTESIAN_POINT('Ctrl Pts',(-6.00001630640013,-9.66191411481669,
-1.82655080280035));
#45335=CARTESIAN_POINT('Ctrl Pts',(-5.99999991734079,-9.6578395448413,-1.84458389836406));
#45336=CARTESIAN_POINT('Ctrl Pts',(-5.99999992038511,-9.65438777104218,
-1.86247659809221));
#45337=CARTESIAN_POINT('Ctrl Pts',(-5.72001867922522,-9.72697756829748,
-2.0594327038003));
#45338=CARTESIAN_POINT('Ctrl Pts',(-5.77222801794758,-9.71178780265897,
-2.03468832666118));
#45339=CARTESIAN_POINT('Ctrl Pts',(-5.82158476387888,-9.69822399312625,
-2.00571488891083));
#45340=CARTESIAN_POINT('Ctrl Pts',(-5.86823437671508,-9.68614875469511,
-1.97285223877799));
#45341=CARTESIAN_POINT('Ctrl Pts',(-5.91488398955128,-9.67407351626397,
-1.93998958864516));
#45342=CARTESIAN_POINT('Ctrl Pts',(-5.95882664449167,-9.6634872700105,-1.90323780725514));
#45343=CARTESIAN_POINT('Ctrl Pts',(-6.00000007205025,-9.65438813918026,
-1.8624766691116));
#45344=CARTESIAN_POINT('Ctrl Pts',(-5.73278528549769,-10.3449554307779,
-1.71288422662173));
#45345=CARTESIAN_POINT('Ctrl Pts',(-5.74758703926587,-10.3336956641858,
-1.70324286602081));
#45346=CARTESIAN_POINT('Ctrl Pts',(-5.76154733999022,-10.3229876482558,
-1.69304521941782));
#45347=CARTESIAN_POINT('Ctrl Pts',(-5.77466527474165,-10.312824454024,-1.68252036580709));
#45348=CARTESIAN_POINT('Ctrl Pts',(-5.78865529222855,-10.3019856087545,
-1.67129581797611));
#45349=CARTESIAN_POINT('Ctrl Pts',(-5.80168737233449,-10.2917664779376,
-1.65969882280271));
#45350=CARTESIAN_POINT('Ctrl Pts',(-5.81378838674191,-10.2821515626752,
-1.64795566811796));
#45351=CARTESIAN_POINT('Ctrl Pts',(-5.81702433828646,-10.2795804228643,
-1.64481541241207));
#45352=CARTESIAN_POINT('Ctrl Pts',(-5.82019384896885,-10.2770524509315,
-1.64166444950863));
#45353=CARTESIAN_POINT('Ctrl Pts',(-5.82329771974396,-10.2745672670514,
-1.63850657699136));
#45354=CARTESIAN_POINT('Ctrl Pts',(-5.8355361489205,-10.2647682937338,-1.62605522126444));
#45355=CARTESIAN_POINT('Ctrl Pts',(-5.84675316302517,-10.2556347018213,
-1.61350107932942));
#45356=CARTESIAN_POINT('Ctrl Pts',(-5.85702788756751,-10.2471307840155,
-1.60107214140025));
#45357=CARTESIAN_POINT('Ctrl Pts',(-5.86787652332103,-10.2381518662477,
-1.58794896521767));
#45358=CARTESIAN_POINT('Ctrl Pts',(-5.87767498429896,-10.2298749456108,
-1.57496478366363));
#45359=CARTESIAN_POINT('Ctrl Pts',(-5.88652865659392,-10.2222552746475,
-1.56232703905979));
#45360=CARTESIAN_POINT('Ctrl Pts',(-5.89063581815402,-10.2187205583582,
-1.55646447072499));
#45361=CARTESIAN_POINT('Ctrl Pts',(-5.89453980742874,-10.2153272436063,
-1.5506756773578));
#45362=CARTESIAN_POINT('Ctrl Pts',(-5.89825174144949,-10.2120707033626,
-1.54497772837812));
#45363=CARTESIAN_POINT('Ctrl Pts',(-5.90079700827138,-10.2098376992763,
-1.54107065448895));
#45364=CARTESIAN_POINT('Ctrl Pts',(-5.90325198131623,-10.2076690021697,
-1.5372062485125));
#45365=CARTESIAN_POINT('Ctrl Pts',(-5.90562031314519,-10.2055631001007,
-1.53338947434416));
#45366=CARTESIAN_POINT('Ctrl Pts',(-5.90870165683338,-10.2028231934842,
-1.52842361911682));
#45367=CARTESIAN_POINT('Ctrl Pts',(-5.91163635921931,-10.2001895742701,
-1.52353845169898));
#45368=CARTESIAN_POINT('Ctrl Pts',(-5.91443325305649,-10.1976585839042,
-1.5187447557545));
#45369=CARTESIAN_POINT('Ctrl Pts',(-5.91690655130083,-10.1954204245772,
-1.51450568181975));
#45370=CARTESIAN_POINT('Ctrl Pts',(-5.91927202264034,-10.193262552503,-1.5103382089865));
#45371=CARTESIAN_POINT('Ctrl Pts',(-5.92153571922348,-10.19118246343,-1.50624882670116));
#45372=CARTESIAN_POINT('Ctrl Pts',(-5.92266756751504,-10.1901424188935,
-1.50420413555849));
#45373=CARTESIAN_POINT('Ctrl Pts',(-5.92377396493195,-10.1891218219138,
-1.50217896241016));
#45374=CARTESIAN_POINT('Ctrl Pts',(-5.92485564717634,-10.1881203718994,
-1.50017406310495));
#45375=CARTESIAN_POINT('Ctrl Pts',(-5.92560719767657,-10.1874245665803,
-1.49878106337368));
#45376=CARTESIAN_POINT('Ctrl Pts',(-5.92602433317219,-10.1870369676126,
-1.49800196274449));
#45377=CARTESIAN_POINT('Ctrl Pts',(-5.92678068430343,-10.1863338258392,
-1.49657861446054));
#45378=CARTESIAN_POINT('Ctrl Pts',(-5.92711292480898,-10.1860249584777,
-1.49595338375233));
#45379=CARTESIAN_POINT('Ctrl Pts',(-5.92751030725292,-10.1856553325483,
-1.49520362583492));
#45380=CARTESIAN_POINT('Ctrl Pts',(-5.92802726401371,-10.1851731662489,
-1.49422091618995));
#45381=CARTESIAN_POINT('Ctrl Pts',(-5.93805899290194,-10.1758165585765,
-1.47515108775915));
#45382=CARTESIAN_POINT('Ctrl Pts',(-5.94688316212083,-10.167219859019,-1.45604567430618));
#45383=CARTESIAN_POINT('Ctrl Pts',(-5.95457617719396,-10.1593487697172,
-1.43711977445761));
#45384=CARTESIAN_POINT('Ctrl Pts',(-5.95804238262117,-10.1558023302267,
-1.42859242124872));
#45385=CARTESIAN_POINT('Ctrl Pts',(-5.96127901274585,-10.1524031576502,
-1.42010076683425));
#45386=CARTESIAN_POINT('Ctrl Pts',(-5.96429344506242,-10.1491478826819,
-1.41166115255928));
#45387=CARTESIAN_POINT('Ctrl Pts',(-5.97111461924745,-10.1417817204174,
-1.39256366653919));
#45388=CARTESIAN_POINT('Ctrl Pts',(-5.97679899638919,-10.1351521056581,
-1.37373632694532));
#45389=CARTESIAN_POINT('Ctrl Pts',(-5.9814779356399,-10.1292018249404,-1.35536282981741));
#45390=CARTESIAN_POINT('Ctrl Pts',(-5.98645891671279,-10.1228674328817,
-1.33580325946756));
#45391=CARTESIAN_POINT('Ctrl Pts',(-5.99030000768087,-10.1173030384771,
-1.31675774988199));
#45392=CARTESIAN_POINT('Ctrl Pts',(-5.99315258066888,-10.1124410972658,
-1.29838967202608));
#45393=CARTESIAN_POINT('Ctrl Pts',(-5.99393040688752,-10.1111153659476,
-1.29338115073585));
#45394=CARTESIAN_POINT('Ctrl Pts',(-5.99463471835723,-10.1098418656255,
-1.28842269455032));
#45395=CARTESIAN_POINT('Ctrl Pts',(-5.99526856528322,-10.1086192284365,
-1.28351696554966));
#45396=CARTESIAN_POINT('Ctrl Pts',(-5.99769622385822,-10.1039364800718,
-1.26472783115988));
#45397=CARTESIAN_POINT('Ctrl Pts',(-5.99909225943474,-10.0999991328637,
-1.24671594303783));
#45398=CARTESIAN_POINT('Ctrl Pts',(-5.99967114898183,-10.0967163116773,
-1.22960239785998));
#45399=CARTESIAN_POINT('Ctrl Pts',(-5.99988467765173,-10.0955054132512,
-1.22328991120778));
#45400=CARTESIAN_POINT('Ctrl Pts',(-5.99998680318323,-10.0943836490406,
-1.21709917912635));
#45401=CARTESIAN_POINT('Ctrl Pts',(-5.99998760030264,-10.0933467246824,
-1.2110347037336));
#45402=CARTESIAN_POINT('Ctrl Pts',(-5.72202416445507,-19.896080483841,-0.38635213055219));
#45403=CARTESIAN_POINT('Ctrl Pts',(-5.72274509910989,-19.5069873331202,
-0.666957234194769));
#45404=CARTESIAN_POINT('Ctrl Pts',(-5.72404064479545,-18.6535903875356,
-1.1961908244877));
#45405=CARTESIAN_POINT('Ctrl Pts',(-5.72530480851401,-17.2528827365553,
-1.80439821707277));
#45406=CARTESIAN_POINT('Ctrl Pts',(-5.72546472270845,-15.736565475542,-2.2042607128638));
#45407=CARTESIAN_POINT('Ctrl Pts',(-5.72471296068136,-14.1774181352031,
-2.37060073454058));
#45408=CARTESIAN_POINT('Ctrl Pts',(-5.72306515483269,-12.6107756304975,
-2.29992921776468));
#45409=CARTESIAN_POINT('Ctrl Pts',(-5.72038844431872,-11.1578233703468,
-2.00976160017932));
#45410=CARTESIAN_POINT('Ctrl Pts',(-5.7182968342637,-10.2528022212897,-1.69379809018474));
#45411=CARTESIAN_POINT('Ctrl Pts',(-5.71724124700401,-9.85241025758025,
-1.52490681965617));
#45412=CARTESIAN_POINT('Ctrl Pts',(-5.90060823215151,-19.8625946053881,
-0.339971041473725));
#45413=CARTESIAN_POINT('Ctrl Pts',(-5.90122084670813,-19.4754696620329,
-0.618738138938865));
#45414=CARTESIAN_POINT('Ctrl Pts',(-5.9023204460776,-18.6265003299919,-1.14450141769569));
#45415=CARTESIAN_POINT('Ctrl Pts',(-5.90338936516232,-17.2335638027759,
-1.74868173897509));
#45416=CARTESIAN_POINT('Ctrl Pts',(-5.90352454452386,-15.7258613601765,
-2.14619370052648));
#45417=CARTESIAN_POINT('Ctrl Pts',(-5.90288894892118,-14.1756858957418,
-2.31193403433321));
#45418=CARTESIAN_POINT('Ctrl Pts',(-5.901494071418,-12.6178346891394,-2.24244445825396));
#45419=CARTESIAN_POINT('Ctrl Pts',(-5.89921767773962,-11.1727295931907,
-1.95513745678009));
#45420=CARTESIAN_POINT('Ctrl Pts',(-5.89743434113683,-10.2722519885276,
-1.64180928578988));
#45421=CARTESIAN_POINT('Ctrl Pts',(-5.89652835820574,-9.87381091535684,
-1.47428053681659));
#45422=CARTESIAN_POINT('Ctrl Pts',(-6.00788367329973,-19.772514726196,-0.215201886826365));
#45423=CARTESIAN_POINT('Ctrl Pts',(-6.00820500171987,-19.3910981597869,
-0.489597435763965));
#45424=CARTESIAN_POINT('Ctrl Pts',(-6.00878012268355,-18.5546160874628,
-1.00717322647165));
#45425=CARTESIAN_POINT('Ctrl Pts',(-6.00933405165869,-17.182687364822,-1.60184063753912));
#45426=CARTESIAN_POINT('Ctrl Pts',(-6.00940405655402,-15.6976641614973,
-1.99332436904445));
#45427=CARTESIAN_POINT('Ctrl Pts',(-6.00907475857469,-14.1710484293059,
-2.15676410330651));
#45428=CARTESIAN_POINT('Ctrl Pts',(-6.00834991091154,-12.6365876990538,
-2.08880850537947));
#45429=CARTESIAN_POINT('Ctrl Pts',(-6.00715353710836,-11.2131204160208,
-1.80660613510079));
#45430=CARTESIAN_POINT('Ctrl Pts',(-6.00621053085834,-10.3258101505897,
-1.49852045391835));
#45431=CARTESIAN_POINT('Ctrl Pts',(-6.00572389292896,-9.93320084529256,
-1.33378507160552));
#45432=CARTESIAN_POINT('Ctrl Pts',(-5.99961011528539,-19.662775821354,-0.0632031012907194));
#45433=CARTESIAN_POINT('Ctrl Pts',(-5.999576626112,-19.2884675084672,-0.332486393375608));
#45434=CARTESIAN_POINT('Ctrl Pts',(-5.99951378747744,-18.4674126509003,
-0.840515375700035));
#45435=CARTESIAN_POINT('Ctrl Pts',(-5.99944414651886,-17.1211147651734,
-1.42408546730994));
#45436=CARTESIAN_POINT('Ctrl Pts',(-5.99943526138757,-15.6635358355136,
-1.8083351975207));
#45437=CARTESIAN_POINT('Ctrl Pts',(-5.9994767984071,-14.165407226967,-1.96871625381771));
#45438=CARTESIAN_POINT('Ctrl Pts',(-5.99956434621717,-12.659345301581,-1.90201657891025));
#45439=CARTESIAN_POINT('Ctrl Pts',(-5.99968486264664,-11.2624348032458,
-1.6250680610208));
#45440=CARTESIAN_POINT('Ctrl Pts',(-5.99976969499778,-10.3915173827786,
-1.32268120907084));
#45441=CARTESIAN_POINT('Ctrl Pts',(-5.99980021247357,-10.0062299524239,
-1.1610240938064));
#45442=CARTESIAN_POINT('',(-5.99999988467789,-19.5919337295697,-0.135483989339417));
#45443=CARTESIAN_POINT('Origin',(-5.59998164341111,-19.5919273324348,-0.135474139643786));
#45444=CARTESIAN_POINT('Ctrl Pts',(-6.,-19.5919320859662,-0.135483413483151));
#45445=CARTESIAN_POINT('Ctrl Pts',(-6.,-19.2032417091454,-0.410171487578889));
#45446=CARTESIAN_POINT('Ctrl Pts',(-6.,-18.7991432008221,-0.654503377429215));
#45447=CARTESIAN_POINT('Ctrl Pts',(-6.,-18.3770565087312,-0.869913253532343));
#45448=CARTESIAN_POINT('Ctrl Pts',(-6.,-17.9549695181175,-1.08532328198508));
#45449=CARTESIAN_POINT('Ctrl Pts',(-6.,-17.5148943182916,-1.27181125578016));
#45450=CARTESIAN_POINT('Ctrl Pts',(-6.,-17.0647735489823,-1.42538958558456));
#45451=CARTESIAN_POINT('Ctrl Pts',(-6.,-16.6146527796733,-1.57896791538885));
#45452=CARTESIAN_POINT('Ctrl Pts',(-6.,-16.1544864408809,-1.69963660120252));
#45453=CARTESIAN_POINT('Ctrl Pts',(-6.,-15.6870767394187,-1.78685625681736));
#45454=CARTESIAN_POINT('Ctrl Pts',(-6.,-15.2196670379562,-1.87407591243227));
#45455=CARTESIAN_POINT('Ctrl Pts',(-6.,-14.7450139738239,-1.9278465378483));
#45456=CARTESIAN_POINT('Ctrl Pts',(-6.,-14.2698875141637,-1.94742220575385));
#45457=CARTESIAN_POINT('Ctrl Pts',(-6.,-13.7947610545038,-1.96699787365938));
#45458=CARTESIAN_POINT('Ctrl Pts',(-6.,-13.3191611993158,-1.95237858405447));
#45459=CARTESIAN_POINT('Ctrl Pts',(-6.,-12.8461741404248,-1.9034307291296));
#45460=CARTESIAN_POINT('Ctrl Pts',(-6.,-12.3731870815335,-1.8544828742047));
#45461=CARTESIAN_POINT('Ctrl Pts',(-6.,-11.902812818939,-1.7712064539598));
#45462=CARTESIAN_POINT('Ctrl Pts',(-6.,-11.4430952346575,-1.65563716855819));
#45463=CARTESIAN_POINT('Ctrl Pts',(-6.,-10.9833776503763,-1.54006788315667));
#45464=CARTESIAN_POINT('Ctrl Pts',(-6.,-10.534316744408,-1.3922057325985));
#45465=CARTESIAN_POINT('Ctrl Pts',(-6.,-10.0933467248347,-1.21103470482109));
#45466=CARTESIAN_POINT('Origin',(-5.599999999997,-19.5919343769627,-0.135488060674723));
#45467=CARTESIAN_POINT('Origin',(-5.6,-19.5919343770088,-0.135488060674804));
#45468=CARTESIAN_POINT('Ctrl Pts',(-6.05109153972374,-10.3133667341249,
1.22786565167224));
#45469=CARTESIAN_POINT('Ctrl Pts',(-6.05168701826986,-10.3097181511851,
1.25641881093765));
#45470=CARTESIAN_POINT('Ctrl Pts',(-6.04650592810586,-10.3031083021162,
1.32768592853605));
#45471=CARTESIAN_POINT('Ctrl Pts',(-6.01133171463065,-10.3019952910507,
1.44465332307405));
#45472=CARTESIAN_POINT('Ctrl Pts',(-5.93768049219332,-10.3139871653149,
1.56711227223071));
#45473=CARTESIAN_POINT('Ctrl Pts',(-5.83457780306427,-10.338943074529,1.66810020812682));
#45474=CARTESIAN_POINT('Ctrl Pts',(-5.75268739346611,-10.3627238857495,
1.71461716070258));
#45475=CARTESIAN_POINT('Ctrl Pts',(-5.71134642253387,-10.3755278527837,
1.73144896239704));
#45476=CARTESIAN_POINT('Ctrl Pts',(-5.91162511589862,-10.0312698687459,
1.19498180009067));
#45477=CARTESIAN_POINT('Ctrl Pts',(-5.91217091556656,-10.0279827855256,
1.22064564700957));
#45478=CARTESIAN_POINT('Ctrl Pts',(-5.90742260833259,-10.0220743811926,
1.28499549547033));
#45479=CARTESIAN_POINT('Ctrl Pts',(-5.87483642927485,-10.0214543387037,
1.39153554130379));
#45480=CARTESIAN_POINT('Ctrl Pts',(-5.80621654839343,-10.0331762556504,
1.50374676368135));
#45481=CARTESIAN_POINT('Ctrl Pts',(-5.7099450100689,-10.0569984449157,1.5965419795219));
#45482=CARTESIAN_POINT('Ctrl Pts',(-5.63351072591731,-10.0794492920087,
1.63929312886841));
#45483=CARTESIAN_POINT('Ctrl Pts',(-5.59497657724959,-10.0914724853859,
1.65475784875777));
#45484=CARTESIAN_POINT('Ctrl Pts',(-6.02845068814037,-9.73989925133785,
1.1553984959079));
#45485=CARTESIAN_POINT('Ctrl Pts',(-6.02930891897681,-9.734848401818,1.19496164129932));
#45486=CARTESIAN_POINT('Ctrl Pts',(-6.02183770779464,-9.72585114962533,
1.29200191301737));
#45487=CARTESIAN_POINT('Ctrl Pts',(-5.97369625583695,-9.72423080924438,
1.44601588767161));
#45488=CARTESIAN_POINT('Ctrl Pts',(-5.87575056987504,-9.7394605190118,1.60373718212841));
#45489=CARTESIAN_POINT('Ctrl Pts',(-5.74020185361633,-9.77133573768165,
1.73283824846435));
#45490=CARTESIAN_POINT('Ctrl Pts',(-5.63231671304093,-9.80212962140831,
1.79269764930981));
#45491=CARTESIAN_POINT('Ctrl Pts',(-5.57746663048118,-9.81892782672867,
1.8145192676118));
#45492=CARTESIAN_POINT('Ctrl Pts',(-6.32476389007387,-9.63080942597427,
1.13513882712025));
#45493=CARTESIAN_POINT('Ctrl Pts',(-6.32609126151429,-9.62302909136911,
1.19625211045084));
#45494=CARTESIAN_POINT('Ctrl Pts',(-6.31453156942281,-9.60918339014722,
1.34409893727426));
#45495=CARTESIAN_POINT('Ctrl Pts',(-6.24291798999123,-9.60572710830813,
1.57227748454183));
#45496=CARTESIAN_POINT('Ctrl Pts',(-6.10056892161608,-9.62593624443112,
1.80134710805399));
#45497=CARTESIAN_POINT('Ctrl Pts',(-5.90545656698247,-9.66975696497354,
1.9873841556488));
#45498=CARTESIAN_POINT('Ctrl Pts',(-5.74989022311378,-9.71308195056143,
2.07397843945383));
#45499=CARTESIAN_POINT('Ctrl Pts',(-5.67032798222648,-9.73707173278376,
2.10570174094662));
#45500=CARTESIAN_POINT('',(-5.73278684135576,-10.3449539124238,1.71288839099263));
#45501=CARTESIAN_POINT('',(-5.72001801994993,-9.72697588660814,2.0594323552405));
#45502=CARTESIAN_POINT('Origin',(-5.89875570320666,-10.183796169743,2.15613415615742));
#45503=CARTESIAN_POINT('',(-5.99999929232988,-9.65439067775597,1.86246363135436));
#45504=CARTESIAN_POINT('Ctrl Pts',(-5.99999893849482,-9.65439067472951,
1.86246363077086));
#45505=CARTESIAN_POINT('Ctrl Pts',(-5.97805268655099,-9.65924092589487,
1.88418829577225));
#45506=CARTESIAN_POINT('Ctrl Pts',(-5.95524919802917,-9.66452973534359,
1.90483819465336));
#45507=CARTESIAN_POINT('Ctrl Pts',(-5.93158556654339,-9.67026253132554,
1.92442749634617));
#45508=CARTESIAN_POINT('Ctrl Pts',(-5.9160574628656,-9.67402439900105,1.93728201987288));
#45509=CARTESIAN_POINT('Ctrl Pts',(-5.90015824989656,-9.67797778998414,
1.94967915132359));
#45510=CARTESIAN_POINT('Ctrl Pts',(-5.88388032252451,-9.68212790070371,
1.96161343442713));
#45511=CARTESIAN_POINT('Ctrl Pts',(-5.87899228981368,-9.68337412059936,
1.96519713183879));
#45512=CARTESIAN_POINT('Ctrl Pts',(-5.87407007591581,-9.684638098141,1.96873903743644));
#45513=CARTESIAN_POINT('Ctrl Pts',(-5.8691134996699,-9.68591996775037,1.97223895502917));
#45514=CARTESIAN_POINT('Ctrl Pts',(-5.84413887119461,-9.69237890546449,
1.98987393878327));
#45515=CARTESIAN_POINT('Ctrl Pts',(-5.8182953080106,-9.69929107464239,2.00644232267157));
#45516=CARTESIAN_POINT('Ctrl Pts',(-5.79155901126676,-9.70667871645196,
2.02188615936239));
#45517=CARTESIAN_POINT('Ctrl Pts',(-5.76839010741707,-9.71308063383048,
2.03526934293446));
#45518=CARTESIAN_POINT('Ctrl Pts',(-5.74455030676941,-9.71983983716558,
2.04780760010186));
#45519=CARTESIAN_POINT('Ctrl Pts',(-5.72001861626288,-9.72697741058235,
2.05943267791248));
#45520=CARTESIAN_POINT('',(-5.99998819251561,-10.0933467209694,1.21103471954976));
#45521=CARTESIAN_POINT('Ctrl Pts',(-5.99998819251561,-10.0933467209694,
1.21103471954976));
#45522=CARTESIAN_POINT('Ctrl Pts',(-5.99998385620494,-10.0704631806786,
1.22848204334355));
#45523=CARTESIAN_POINT('Ctrl Pts',(-5.99998335501883,-10.0483848922226,
1.24627131943011));
#45524=CARTESIAN_POINT('Ctrl Pts',(-5.99998071362119,-10.0271414920569,
1.26441751382506));
#45525=CARTESIAN_POINT('Ctrl Pts',(-5.99997953604353,-10.0176708417291,
1.27250737988019));
#45526=CARTESIAN_POINT('Ctrl Pts',(-5.99997744109942,-10.0083656975942,
1.28066765022114));
#45527=CARTESIAN_POINT('Ctrl Pts',(-5.99997276079776,-9.99922669686015,
1.28889762257333));
#45528=CARTESIAN_POINT('Ctrl Pts',(-5.99995937880447,-9.97309631996056,
1.31242889100122));
#45529=CARTESIAN_POINT('Ctrl Pts',(-5.99992732479033,-9.94832580753097,
1.33652904861389));
#45530=CARTESIAN_POINT('Ctrl Pts',(-5.99991639997273,-9.92486788112492,
1.36119507363657));
#45531=CARTESIAN_POINT('Ctrl Pts',(-5.99990337118461,-9.89689227876561,
1.39061143789123));
#45532=CARTESIAN_POINT('Ctrl Pts',(-5.99990194905953,-9.87082206904309,
1.4208469219927));
#45533=CARTESIAN_POINT('Ctrl Pts',(-5.99990827523113,-9.8466640461254,1.4518882119366));
#45534=CARTESIAN_POINT('Ctrl Pts',(-5.99991044005314,-9.83839714741086,
1.46251057125836));
#45535=CARTESIAN_POINT('Ctrl Pts',(-5.99991349017294,-9.83035412851919,
1.47322774561128));
#45536=CARTESIAN_POINT('Ctrl Pts',(-5.99991818442103,-9.82253532698912,
1.48404251962809));
#45537=CARTESIAN_POINT('Ctrl Pts',(-5.99992099506536,-9.8178538807407,1.49051778096498));
#45538=CARTESIAN_POINT('Ctrl Pts',(-5.99992891243512,-9.8130914911253,1.4972467019501));
#45539=CARTESIAN_POINT('Ctrl Pts',(-5.9999340958716,-9.80847580936703,1.50393435657881));
#45540=CARTESIAN_POINT('Ctrl Pts',(-5.99993934522864,-9.80380142749364,
1.51070706171949));
#45541=CARTESIAN_POINT('Ctrl Pts',(-5.99994151967764,-9.79927770768895,
1.51743718021492));
#45542=CARTESIAN_POINT('Ctrl Pts',(-5.99994633539954,-9.79510546243412,
1.52377937107288));
#45543=CARTESIAN_POINT('Ctrl Pts',(-5.99994714803865,-9.79440140813732,
1.52484959740233));
#45544=CARTESIAN_POINT('Ctrl Pts',(-5.99994807169794,-9.79370727989116,
1.52590869658738));
#45545=CARTESIAN_POINT('Ctrl Pts',(-5.99994917731444,-9.79302394495788,
1.52695491650741));
#45546=CARTESIAN_POINT('Ctrl Pts',(-5.99997543479574,-9.77679530309569,
1.55180177792813));
#45547=CARTESIAN_POINT('Ctrl Pts',(-5.99996041338706,-9.7619038161661,1.57694685829143));
#45548=CARTESIAN_POINT('Ctrl Pts',(-5.99993528590784,-9.74828232671954,
1.60234427928765));
#45549=CARTESIAN_POINT('Ctrl Pts',(-5.99991079530336,-9.73500608410708,
1.62709798366042));
#45550=CARTESIAN_POINT('Ctrl Pts',(-5.99987824956351,-9.7229352977466,1.65209229785361));
#45551=CARTESIAN_POINT('Ctrl Pts',(-5.99986339636884,-9.71204080581989,
1.6773206358393));
#45552=CARTESIAN_POINT('Ctrl Pts',(-5.99985777962819,-9.7079210499701,1.68686074048081));
#45553=CARTESIAN_POINT('Ctrl Pts',(-5.99985454323938,-9.70396991374468,
1.69643460684258));
#45554=CARTESIAN_POINT('Ctrl Pts',(-5.99985429814471,-9.70018741400251,
1.70604274813774));
#45555=CARTESIAN_POINT('Ctrl Pts',(-5.99985368026242,-9.69065175332556,
1.73026481855996));
#45556=CARTESIAN_POINT('Ctrl Pts',(-5.999874605093,-9.68218513529061,1.75470487599331));
#45557=CARTESIAN_POINT('Ctrl Pts',(-5.99990791809376,-9.67481341330724,
1.77937946321238));
#45558=CARTESIAN_POINT('Ctrl Pts',(-5.99994036861482,-9.6676325465567,1.80341522084737));
#45559=CARTESIAN_POINT('Ctrl Pts',(-5.99998501038468,-9.66149118947295,
1.82767449085469));
#45560=CARTESIAN_POINT('Ctrl Pts',(-5.99999646663191,-9.65644537758714,
1.85216368682354));
#45561=CARTESIAN_POINT('Ctrl Pts',(-5.99999807067108,-9.65573889144184,
1.85559252603773));
#45562=CARTESIAN_POINT('Ctrl Pts',(-5.99999895813432,-9.65505392589765,
1.85902584493278));
#45563=CARTESIAN_POINT('Ctrl Pts',(-5.99999893849482,-9.65439067472951,
1.86246363077086));
#45564=CARTESIAN_POINT('Ctrl Pts',(-5.99998819251561,-10.0933467209694,
1.21103471954976));
#45565=CARTESIAN_POINT('Ctrl Pts',(-5.99998402550715,-10.0961384851397,
1.22737632814287));
#45566=CARTESIAN_POINT('Ctrl Pts',(-5.99924438896618,-10.0995471624567,
1.24464108102516));
#45567=CARTESIAN_POINT('Ctrl Pts',(-5.99756998416535,-10.1036582604973,
1.26272592288279));
#45568=CARTESIAN_POINT('Ctrl Pts',(-5.99660204936694,-10.1060347914599,
1.27318035286841));
#45569=CARTESIAN_POINT('Ctrl Pts',(-5.99532147474186,-10.1086461707087,
1.28390802980007));
#45570=CARTESIAN_POINT('Ctrl Pts',(-5.99368665768074,-10.1115100796409,
1.29488167197767));
#45571=CARTESIAN_POINT('Ctrl Pts',(-5.99144878963691,-10.1154304267136,
1.30990326903442));
#45572=CARTESIAN_POINT('Ctrl Pts',(-5.98854666000694,-10.1198241527659,
1.32538674595495));
#45573=CARTESIAN_POINT('Ctrl Pts',(-5.98489855986274,-10.1247279755564,
1.3412469846118));
#45574=CARTESIAN_POINT('Ctrl Pts',(-5.98070306937735,-10.1303676074323,
1.35948702127484));
#45575=CARTESIAN_POINT('Ctrl Pts',(-5.97552128947864,-10.1366817915978,
1.37822691854081));
#45576=CARTESIAN_POINT('Ctrl Pts',(-5.96922654119519,-10.1437264409335,
1.39729514499616));
#45577=CARTESIAN_POINT('Ctrl Pts',(-5.96732685751383,-10.1458524362523,
1.40304971960318));
#45578=CARTESIAN_POINT('Ctrl Pts',(-5.96532577018031,-10.1480449657855,
1.40883384962093));
#45579=CARTESIAN_POINT('Ctrl Pts',(-5.96321966706526,-10.150305591362,1.41464186523372));
#45580=CARTESIAN_POINT('Ctrl Pts',(-5.96201716271702,-10.1515963221273,
1.41795802006921));
#45581=CARTESIAN_POINT('Ctrl Pts',(-5.96078042200169,-10.1529092522677,
1.42128195300577));
#45582=CARTESIAN_POINT('Ctrl Pts',(-5.95950875996098,-10.1542446751975,
1.42461253551312));
#45583=CARTESIAN_POINT('Ctrl Pts',(-5.95597676213336,-10.1579537667138,
1.43386311452248));
#45584=CARTESIAN_POINT('Ctrl Pts',(-5.95217532292998,-10.161836398445,1.4431651786973));
#45585=CARTESIAN_POINT('Ctrl Pts',(-5.94809550841192,-10.1658966382478,
1.45249663410328));
#45586=CARTESIAN_POINT('Ctrl Pts',(-5.94532115205228,-10.1686576834054,
1.45884221244653));
#45587=CARTESIAN_POINT('Ctrl Pts',(-5.94241803296839,-10.1715009005813,
1.46520142973038));
#45588=CARTESIAN_POINT('Ctrl Pts',(-5.93938352102913,-10.1744274340502,
1.47156643417996));
#45589=CARTESIAN_POINT('Ctrl Pts',(-5.93786470710498,-10.1758922033017,
1.47475220427373));
#45590=CARTESIAN_POINT('Ctrl Pts',(-5.93608622095482,-10.177596339097,1.47840532593482));
#45591=CARTESIAN_POINT('Ctrl Pts',(-5.93438240493213,-10.1792142823947,
1.48182159957326));
#45592=CARTESIAN_POINT('Ctrl Pts',(-5.93268208435788,-10.1808289064154,
1.48523086458626));
#45593=CARTESIAN_POINT('Ctrl Pts',(-5.93105726019389,-10.1823572353098,
1.48840473398473));
#45594=CARTESIAN_POINT('Ctrl Pts',(-5.92988309980082,-10.1834582505981,
1.4906706473117));
#45595=CARTESIAN_POINT('Ctrl Pts',(-5.92268037136545,-10.1902122802619,
1.50457058674809));
#45596=CARTESIAN_POINT('Ctrl Pts',(-5.91461871252513,-10.1975738668864,
1.51888678624592));
#45597=CARTESIAN_POINT('Ctrl Pts',(-5.90558148547629,-10.2055918580846,
1.53344585887442));
#45598=CARTESIAN_POINT('Ctrl Pts',(-5.90267790306295,-10.208167968888,1.53812356222416));
#45599=CARTESIAN_POINT('Ctrl Pts',(-5.899673623005,-10.2108118399798,1.54282594880722));
#45600=CARTESIAN_POINT('Ctrl Pts',(-5.89656480451811,-10.2135250963317,
1.54754608499053));
#45601=CARTESIAN_POINT('Ctrl Pts',(-5.8871051820906,-10.2217810883578,1.56190868167757));
#45602=CARTESIAN_POINT('Ctrl Pts',(-5.87667643703934,-10.2306799225328,
1.5764390153283));
#45603=CARTESIAN_POINT('Ctrl Pts',(-5.86519923836702,-10.2402555319518,
1.59093668969711));
#45604=CARTESIAN_POINT('Ctrl Pts',(-5.85453478592901,-10.2491530542592,
1.60440772589525));
#45605=CARTESIAN_POINT('Ctrl Pts',(-5.84296508897445,-10.2586348387852,
1.61785078716441));
#45606=CARTESIAN_POINT('Ctrl Pts',(-5.83043950416598,-10.2687242962313,
1.6310627672712));
#45607=CARTESIAN_POINT('Ctrl Pts',(-5.82324245850783,-10.2745215733257,
1.63865420715343));
#45608=CARTESIAN_POINT('Ctrl Pts',(-5.81573006887528,-10.2805194060275,
1.64616855216329));
#45609=CARTESIAN_POINT('Ctrl Pts',(-5.80789496961468,-10.2867217253361,
1.65355967409042));
#45610=CARTESIAN_POINT('Ctrl Pts',(-5.79492426015451,-10.2969894295546,
1.66579539592531));
#45611=CARTESIAN_POINT('Ctrl Pts',(-5.78106749379734,-10.3078180566375,
1.67769523356719));
#45612=CARTESIAN_POINT('Ctrl Pts',(-5.76632933899584,-10.3192095047188,
1.68905255240334));
#45613=CARTESIAN_POINT('Ctrl Pts',(-5.7556093897998,-10.3274951921976,1.69731341562309));
#45614=CARTESIAN_POINT('Ctrl Pts',(-5.74442358376035,-10.3360784934701,
1.70528659045044));
#45615=CARTESIAN_POINT('Ctrl Pts',(-5.73278287705707,-10.3449577598948,
1.71287781032009));
#45616=CARTESIAN_POINT('Ctrl Pts',(-5.71725917948286,-9.85240188395848,
1.52489732935885));
#45617=CARTESIAN_POINT('Ctrl Pts',(-5.71831476133586,-10.2527968008031,
1.69379032983208));
#45618=CARTESIAN_POINT('Ctrl Pts',(-5.72040635428649,-11.1578213001714,
2.00975542479402));
#45619=CARTESIAN_POINT('Ctrl Pts',(-5.72308302960212,-12.6107763015806,
2.29992344875424));
#45620=CARTESIAN_POINT('Ctrl Pts',(-5.72473081064846,-14.177417972093,2.37059485980144));
#45621=CARTESIAN_POINT('Ctrl Pts',(-5.72548256087693,-15.7365643949578,
2.20425489419934));
#45622=CARTESIAN_POINT('Ctrl Pts',(-5.72532264924983,-17.2528807820375,
1.80439264348976));
#45623=CARTESIAN_POINT('Ctrl Pts',(-5.72405850848059,-18.6535837735938,
1.19618733853812));
#45624=CARTESIAN_POINT('Ctrl Pts',(-5.72276299024073,-19.5069768607809,
0.666956934041539));
#45625=CARTESIAN_POINT('Ctrl Pts',(-5.72204207444442,-19.8960667568706,
0.386354961461413));
#45626=CARTESIAN_POINT('Ctrl Pts',(-5.89585261036639,-9.8737233640862,1.47445851034686));
#45627=CARTESIAN_POINT('Ctrl Pts',(-5.89675914115004,-10.2721745670443,
1.64199409608624));
#45628=CARTESIAN_POINT('Ctrl Pts',(-5.89854359746305,-11.1726722809412,
1.95533375189407));
#45629=CARTESIAN_POINT('Ctrl Pts',(-5.90082144131746,-12.6178091621264,
2.24265196275686));
#45630=CARTESIAN_POINT('Ctrl Pts',(-5.90221723230456,-14.1756921586905,
2.31214594307168));
#45631=CARTESIAN_POINT('Ctrl Pts',(-5.90285324758004,-15.7259000244731,
2.14640349435437));
#45632=CARTESIAN_POINT('Ctrl Pts',(-5.90271797885401,-17.2336335815138,
1.74888303750554));
#45633=CARTESIAN_POINT('Ctrl Pts',(-5.90164835746724,-18.626594283756,1.14468975580972));
#45634=CARTESIAN_POINT('Ctrl Pts',(-5.90054805708195,-19.4755761504201,
0.618916685086739));
#45635=CARTESIAN_POINT('Ctrl Pts',(-5.8999350585698,-19.8627051211047,0.340145838838019));
#45636=CARTESIAN_POINT('Ctrl Pts',(-6.00500261470054,-9.93280259933369,
1.33469847615741));
#45637=CARTESIAN_POINT('Ctrl Pts',(-6.00549199806467,-10.3254530800207,
1.49945394791177));
#45638=CARTESIAN_POINT('Ctrl Pts',(-6.00644049339831,-11.2128530699392,
1.80757571669982));
#45639=CARTESIAN_POINT('Ctrl Pts',(-6.00764392772595,-12.6364651528179,
2.08981216442348));
#45640=CARTESIAN_POINT('Ctrl Pts',(-6.00837315204832,-14.1710787346948,
2.15777783010585));
#45641=CARTESIAN_POINT('Ctrl Pts',(-6.00870445126686,-15.6978483680812,
1.99432307775469));
#45642=CARTESIAN_POINT('Ctrl Pts',(-6.00863402048019,-17.1830197265236,
1.6027999689954));
#45643=CARTESIAN_POINT('Ctrl Pts',(-6.00807672884764,-18.5550818810673,
1.00807203283005));
#45644=CARTESIAN_POINT('Ctrl Pts',(-6.00749818443475,-19.3916421670331,
0.490445507156552));
#45645=CARTESIAN_POINT('Ctrl Pts',(-6.00717495695829,-19.7730930164904,
0.216024270399581));
#45646=CARTESIAN_POINT('Ctrl Pts',(-5.99984758538782,-10.0055962683619,
1.16249500094862));
#45647=CARTESIAN_POINT('Ctrl Pts',(-5.99982148563193,-10.3909492485856,
1.32418019721138));
#45648=CARTESIAN_POINT('Ctrl Pts',(-5.99974542173439,-11.2620102881678,
1.62661749324998));
#45649=CARTESIAN_POINT('Ctrl Pts',(-5.99963615320918,-12.6591509434668,
1.90361155864705));
#45650=CARTESIAN_POINT('Ctrl Pts',(-5.99955554136504,-14.1654554059707,
1.97032198330928));
#45651=CARTESIAN_POINT('Ctrl Pts',(-5.99951717118125,-15.6638272479816,
1.80991481185425));
#45652=CARTESIAN_POINT('Ctrl Pts',(-5.9995253825072,-17.1216405130251,1.42560331832749));
#45653=CARTESIAN_POINT('Ctrl Pts',(-5.99958969901559,-18.4681535226324,
0.841940074435576));
#45654=CARTESIAN_POINT('Ctrl Pts',(-5.99964708911067,-19.2893368186713,
0.333832287822943));
#45655=CARTESIAN_POINT('Ctrl Pts',(-5.99967754848037,-19.6637028813994,
0.0645081662955123));
#45656=CARTESIAN_POINT('',(-5.99999997114735,-19.5919329044497,0.135484571583753));
#45657=CARTESIAN_POINT('Ctrl Pts',(-6.,-10.0933467210045,1.21103472159936));
#45658=CARTESIAN_POINT('Ctrl Pts',(-6.,-10.5343167948856,1.39220577636874));
#45659=CARTESIAN_POINT('Ctrl Pts',(-6.,-10.9833777476598,1.54006792210967));
#45660=CARTESIAN_POINT('Ctrl Pts',(-6.,-11.4430953691779,1.65563720320492));
#45661=CARTESIAN_POINT('Ctrl Pts',(-6.,-11.9028129906963,1.77120648430025));
#45662=CARTESIAN_POINT('Ctrl Pts',(-6.,-12.3731872809587,1.85448290074985));
#45663=CARTESIAN_POINT('Ctrl Pts',(-6.,-12.8461743349553,1.90343074841346));
#45664=CARTESIAN_POINT('Ctrl Pts',(-6.,-13.3191613889517,1.95237859607703));
#45665=CARTESIAN_POINT('Ctrl Pts',(-6.,-13.7947612066823,1.96699787495466));
#45666=CARTESIAN_POINT('Ctrl Pts',(-6.,-14.2698876412527,1.94742220105327));
#45667=CARTESIAN_POINT('Ctrl Pts',(-6.,-14.7450140758233,1.92784652715188));
#45668=CARTESIAN_POINT('Ctrl Pts',(-6.,-15.2196671272337,1.87407590047143));
#45669=CARTESIAN_POINT('Ctrl Pts',(-6.,-15.6870768246027,1.78685624112379));
#45670=CARTESIAN_POINT('Ctrl Pts',(-6.,-16.1544865219714,1.69963658177622));
#45671=CARTESIAN_POINT('Ctrl Pts',(-6.,-16.6146528652989,1.5789678897615));
#45672=CARTESIAN_POINT('Ctrl Pts',(-6.,-17.0647736279836,1.42538955895495));
#45673=CARTESIAN_POINT('Ctrl Pts',(-6.,-17.5148943906687,1.2718112281483));
#45674=CARTESIAN_POINT('Ctrl Pts',(-6.,-17.9549695727112,1.08532325854976));
#45675=CARTESIAN_POINT('Ctrl Pts',(-6.,-18.3770565476116,0.869913233962045));
#45676=CARTESIAN_POINT('Ctrl Pts',(-6.,-18.7991432239094,0.654503361764737));
#45677=CARTESIAN_POINT('Ctrl Pts',(-6.,-19.2032417185164,0.410171475499673));
#45678=CARTESIAN_POINT('Ctrl Pts',(-6.,-19.5919320853514,0.135483412539487));
#45679=CARTESIAN_POINT('',(-5.73644356943,-19.8089505408291,0.442546871815091));
#45680=CARTESIAN_POINT('Origin',(-5.59998163820134,-19.5919264032878,0.13547479132357));
#45681=CARTESIAN_POINT('Ctrl Pts',(-5.732787366965,-10.3449534027376,1.71288979180163));
#45682=CARTESIAN_POINT('Ctrl Pts',(-5.7346148093355,-11.1182357980457,1.9933278196275));
#45683=CARTESIAN_POINT('Ctrl Pts',(-5.73605973905547,-11.926552686004,2.18169252040153));
#45684=CARTESIAN_POINT('Ctrl Pts',(-5.73818934963262,-13.567539631559,2.35984303331276));
#45685=CARTESIAN_POINT('Ctrl Pts',(-5.73887403048981,-14.4000937496392,
2.35028712857065));
#45686=CARTESIAN_POINT('Ctrl Pts',(-5.73948314334139,-16.0408967489411,
2.1319111059007));
#45687=CARTESIAN_POINT('Ctrl Pts',(-5.73940757533578,-16.8491807345991,
1.92343367553535));
#45688=CARTESIAN_POINT('Ctrl Pts',(-5.73849619050221,-18.3938447089082,
1.31839091028631));
#45689=CARTESIAN_POINT('Ctrl Pts',(-5.73766037374166,-19.1301818702781,
0.921733792798441));
#45690=CARTESIAN_POINT('Ctrl Pts',(-5.73644356975375,-19.8089503602323,
0.442546999310109));
#45691=CARTESIAN_POINT('Origin',(-5.599999999997,-19.5919343769573,0.135488060979611));
#45692=CARTESIAN_POINT('',(-5.593361696257,-19.9918770425242,0.136828655319171));
#45693=CARTESIAN_POINT('Origin',(-5.599999999997,-19.5919343769573,0.135488060979611));
#45694=CARTESIAN_POINT('Origin',(-5.6,-19.5919343770044,0.135488060981261));
#45695=CARTESIAN_POINT('Ctrl Pts',(-5.59335880963393,-19.9918769844261,
0.13683170217352));
#45696=CARTESIAN_POINT('Ctrl Pts',(-5.59335897597995,-19.9918902023629,
0.132889263698737));
#45697=CARTESIAN_POINT('Ctrl Pts',(-5.59336249921667,-19.9921701764066,
0.0456108094042422));
#45698=CARTESIAN_POINT('Ctrl Pts',(-5.59336249921666,-19.9921701764069,
-0.0456108090957055));
#45699=CARTESIAN_POINT('Ctrl Pts',(-5.59335897597995,-19.9918902023646,
-0.132889263387482));
#45700=CARTESIAN_POINT('Ctrl Pts',(-5.59335880963393,-19.9918769844279,
-0.136831701864102));
#45701=CARTESIAN_POINT('Ctrl Pts',(-5.83074004395823,-19.9958187405297,
0.136844915099748));
#45702=CARTESIAN_POINT('Ctrl Pts',(-5.83074021193959,-19.9958318610111,
0.132902095574058));
#45703=CARTESIAN_POINT('Ctrl Pts',(-5.83074376981186,-19.9961097709333,
0.0456152065241441));
#45704=CARTESIAN_POINT('Ctrl Pts',(-5.83074376981186,-19.9961097709314,
-0.045615206214134));
#45705=CARTESIAN_POINT('Ctrl Pts',(-5.83074021193959,-19.9958318610128,
-0.132902095265616));
#45706=CARTESIAN_POINT('Ctrl Pts',(-5.83074004395823,-19.9958187405316,
-0.136844914793341));
#45707=CARTESIAN_POINT('Ctrl Pts',(-6.0000034748386,-19.8293408303188,0.136286874323727));
#45708=CARTESIAN_POINT('Ctrl Pts',(-6.00000357357481,-19.829353826502,0.132360134067906));
#45709=CARTESIAN_POINT('Ctrl Pts',(-6.00000566482207,-19.8296291037065,
0.0454292086005623));
#45710=CARTESIAN_POINT('Ctrl Pts',(-6.00000566482207,-19.8296291037088,
-0.0454292082960309));
#45711=CARTESIAN_POINT('Ctrl Pts',(-6.00000357357481,-19.829353826505,-0.132360133764468));
#45712=CARTESIAN_POINT('Ctrl Pts',(-6.0000034748386,-19.8293408303218,-0.136286874022272));
#45713=CARTESIAN_POINT('Ctrl Pts',(-5.9999999999769,-19.5919285123994,0.135491058510803));
#45714=CARTESIAN_POINT('Ctrl Pts',(-5.99999999996753,-19.5919414317201,
0.131587249061451));
#45715=CARTESIAN_POINT('Ctrl Pts',(-5.99999999976693,-19.5922150808804,
0.0451639658275807));
#45716=CARTESIAN_POINT('Ctrl Pts',(-5.99999999976693,-19.5922150808839,
-0.0451639655258958));
#45717=CARTESIAN_POINT('Ctrl Pts',(-5.99999999996752,-19.5919414317231,
-0.131587248762213));
#45718=CARTESIAN_POINT('Ctrl Pts',(-5.9999999999769,-19.5919285124023,-0.135491058213592));
#45719=CARTESIAN_POINT('Origin',(-5.47627985805297,17.2206464622639,-6.06762124375979E-6));
#45720=CARTESIAN_POINT('Ctrl Pts',(-6.00000000001697,-19.5919329102801,
0.135482829560807));
#45721=CARTESIAN_POINT('Ctrl Pts',(-6.00000000001005,-19.5919459863973,
0.131581789353999));
#45722=CARTESIAN_POINT('Ctrl Pts',(-6.00000000000347,-19.5919585088244,
0.127680725310898));
#45723=CARTESIAN_POINT('Ctrl Pts',(-5.9999999999973,-19.5919704756413,0.123779639821488));
#45724=CARTESIAN_POINT('Ctrl Pts',(-5.99999999993208,-19.592097039782,0.0825207541337165));
#45725=CARTESIAN_POINT('Ctrl Pts',(-5.99999999990817,-19.5921614523066,
0.0412594672354874));
#45726=CARTESIAN_POINT('Ctrl Pts',(-5.99999999990817,-19.5921614509454,
-1.42316775524837E-6));
#45727=CARTESIAN_POINT('Ctrl Pts',(-5.99999999990817,-19.5921614495841,
-0.0412621564085699));
#45728=CARTESIAN_POINT('Ctrl Pts',(-5.99999999993208,-19.5920970348271,
-0.082522493401898));
#45729=CARTESIAN_POINT('Ctrl Pts',(-5.9999999999973,-19.5919704760377,-0.123779639519363));
#45730=CARTESIAN_POINT('Ctrl Pts',(-6.00000000000346,-19.5919585091991,
-0.127680732537362));
#45731=CARTESIAN_POINT('Ctrl Pts',(-6.00000000001004,-19.5919459867691,
-0.131581797046985));
#45732=CARTESIAN_POINT('Ctrl Pts',(-6.00000000001697,-19.591932910674,-0.135482830660537));
#45733=CARTESIAN_POINT('Ctrl Pts',(-5.67775659315864,-19.9920104400695,
0.353201969755379));
#45734=CARTESIAN_POINT('Ctrl Pts',(-3.78517106210576,-19.9513454585501,
1.27015806410654));
#45735=CARTESIAN_POINT('Ctrl Pts',(-2.07350540383511E-10,-19.8989940825525,
2.18677316177469));
#45736=CARTESIAN_POINT('Ctrl Pts',(3.7851710616912,-19.9513454585464,1.27015806419779));
#45737=CARTESIAN_POINT('Ctrl Pts',(5.67775659253729,-19.9920104400553,0.353201970057756));
#45738=CARTESIAN_POINT('Ctrl Pts',(-5.67775659315864,-19.9939858021668,
0.127302152333014));
#45739=CARTESIAN_POINT('Ctrl Pts',(-3.78517106210576,-19.9624099274875,
0.457989911116222));
#45740=CARTESIAN_POINT('Ctrl Pts',(-2.07350540383511E-10,-20.07929286279,
0.79322766033635));
#45741=CARTESIAN_POINT('Ctrl Pts',(3.7851710616912,-19.9624099274969,0.457989911150634));
#45742=CARTESIAN_POINT('Ctrl Pts',(5.67775659253729,-19.9939858021509,0.127302152445153));
#45743=CARTESIAN_POINT('Ctrl Pts',(-5.67775659315864,-19.9940658453786,
-0.0986748542825062));
#45744=CARTESIAN_POINT('Ctrl Pts',(-3.78517106210576,-19.9628582683932,
-0.355018823012134));
#45745=CARTESIAN_POINT('Ctrl Pts',(-2.07350540383511E-10,-20.0865987098241,
-0.615372372365866));
#45746=CARTESIAN_POINT('Ctrl Pts',(3.7851710616912,-19.9628582684084,-0.355018823042515));
#45747=CARTESIAN_POINT('Ctrl Pts',(5.67775659253729,-19.9940658453618,-0.0986748543637739));
#45748=CARTESIAN_POINT('Ctrl Pts',(-5.67775659315864,-19.9922505697091,
-0.324580927234301));
#45749=CARTESIAN_POINT('Ctrl Pts',(-3.78517106210576,-19.95269048127,-1.16725509800203));
#45750=CARTESIAN_POINT('Ctrl Pts',(-2.07350540383511E-10,-19.9209116236529,
-2.01013791647348));
#45751=CARTESIAN_POINT('Ctrl Pts',(3.7851710616912,-19.9526904812655,-1.16725509809374));
#45752=CARTESIAN_POINT('Ctrl Pts',(5.67775659253729,-19.9922505696944,-0.324580927510664));
#45753=CARTESIAN_POINT('Ctrl Pts',(-5.5933616962571,-19.9918770425183,0.136828655319151));
#45754=CARTESIAN_POINT('Ctrl Pts',(-5.58012472919481,-19.99163674265,0.142971485509285));
#45755=CARTESIAN_POINT('Ctrl Pts',(-5.56080272347521,-19.9912875756678,
0.151932544276364));
#45756=CARTESIAN_POINT('Ctrl Pts',(-5.53535952182951,-19.9908363415534,
0.163638016329727));
#45757=CARTESIAN_POINT('Ctrl Pts',(-5.51000522444049,-19.9903866841523,
0.175302586836719));
#45758=CARTESIAN_POINT('Ctrl Pts',(-5.47857227855432,-19.989835793103,0.189692500930799));
#45759=CARTESIAN_POINT('Ctrl Pts',(-5.44100422143108,-19.9891930595044,
0.2066874873172));
#45760=CARTESIAN_POINT('Ctrl Pts',(-5.41357576116322,-19.9887237993318,
0.21909553672266));
#45761=CARTESIAN_POINT('Ctrl Pts',(-5.38287654985487,-19.9882056556176,
0.232891249080397));
#45762=CARTESIAN_POINT('Ctrl Pts',(-5.34887846376692,-19.9876425066992,
0.24801136658331));
#45763=CARTESIAN_POINT('Ctrl Pts',(-5.30328327368837,-19.9868872617741,
0.268289114859251));
#45764=CARTESIAN_POINT('Ctrl Pts',(-5.25175535678456,-19.9860510323723,
0.29095083654136));
#45765=CARTESIAN_POINT('Ctrl Pts',(-5.1942123821824,-19.9851444278923,0.315802052049564));
#45766=CARTESIAN_POINT('Ctrl Pts',(-5.1577545619446,-19.9845700254846,0.331547173916361));
#45767=CARTESIAN_POINT('Ctrl Pts',(-5.11888187229187,-19.9839673843954,
0.34817024080352));
#45768=CARTESIAN_POINT('Ctrl Pts',(-5.07757050665736,-19.9833390403789,
0.365611308779708));
#45769=CARTESIAN_POINT('Ctrl Pts',(-5.0142792917611,-19.982376383842,0.392331954886338));
#45770=CARTESIAN_POINT('Ctrl Pts',(-4.94526457323561,-19.9813533518089,
0.420975101801376));
#45771=CARTESIAN_POINT('Ctrl Pts',(-4.87043008439426,-19.9802806585483,
0.451284577322271));
#45772=CARTESIAN_POINT('Ctrl Pts',(-4.84061248935803,-19.9798532468864,
0.463361303987141));
#45773=CARTESIAN_POINT('Ctrl Pts',(-4.80987082635485,-19.9794179489913,
0.475702019067311));
#45774=CARTESIAN_POINT('Ctrl Pts',(-4.77819856292879,-19.9789754207395,
0.488288233952837));
#45775=CARTESIAN_POINT('Ctrl Pts',(-4.70106309934213,-19.9778976757931,
0.518941032805151));
#45776=CARTESIAN_POINT('Ctrl Pts',(-4.61840846663568,-19.9767770032238,
0.55105350273108));
#45777=CARTESIAN_POINT('Ctrl Pts',(-4.53013413330441,-19.9756247259809,
0.58432325758402));
#45778=CARTESIAN_POINT('Ctrl Pts',(-4.50292955806877,-19.9752696146846,
0.594576402692142));
#45779=CARTESIAN_POINT('Ctrl Pts',(-4.47519119417953,-19.9749115039132,
0.604939096084163));
#45780=CARTESIAN_POINT('Ctrl Pts',(-4.44691597456336,-19.9745507289419,
0.615401484750342));
#45781=CARTESIAN_POINT('Ctrl Pts',(-4.3578107093497,-19.9734137987985,0.648372189470696));
#45782=CARTESIAN_POINT('Ctrl Pts',(-4.26337415693458,-19.9722503419874,
0.682336805905467));
#45783=CARTESIAN_POINT('Ctrl Pts',(-4.16350818045132,-19.9710726185038,
0.716953903297154));
#45784=CARTESIAN_POINT('Ctrl Pts',(-4.13544195145048,-19.9707416323346,
0.726682655940978));
#45785=CARTESIAN_POINT('Ctrl Pts',(-4.1069468718516,-19.9704095241886,0.736462630533679));
#45786=CARTESIAN_POINT('Ctrl Pts',(-4.07802072641322,-19.9700765770652,
0.74628549838169));
#45787=CARTESIAN_POINT('Ctrl Pts',(-3.98959650005386,-19.9690587922426,
0.776312986556394));
#45788=CARTESIAN_POINT('Ctrl Pts',(-3.89714408537845,-19.968033114597,0.806743604209373));
#45789=CARTESIAN_POINT('Ctrl Pts',(-3.80060148807689,-19.9670086332002,
0.837319610561497));
#45790=CARTESIAN_POINT('Ctrl Pts',(-3.75616522180159,-19.9665370887275,
0.851393020619588));
#45791=CARTESIAN_POINT('Ctrl Pts',(-3.71086243987753,-19.9660658070662,
0.865496800800391));
#45792=CARTESIAN_POINT('Ctrl Pts',(-3.66468717719672,-19.965595723055,0.87960351915793));
#45793=CARTESIAN_POINT('Ctrl Pts',(-3.62904937773455,-19.9652329149462,
0.890491002427281));
#45794=CARTESIAN_POINT('Ctrl Pts',(-3.59289187019038,-19.9648708206383,
0.901380206343566));
#45795=CARTESIAN_POINT('Ctrl Pts',(-3.55621207182732,-19.9645098984448,
0.912257972988526));
#45796=CARTESIAN_POINT('Ctrl Pts',(-3.51410949158726,-19.9640956171159,
0.924743920661103));
#45797=CARTESIAN_POINT('Ctrl Pts',(-3.4713187055698,-19.9636828722794,0.937215022091883));
#45798=CARTESIAN_POINT('Ctrl Pts',(-3.42783597968764,-19.9632723869592,
0.949650254350777));
#45799=CARTESIAN_POINT('Ctrl Pts',(-3.40609461674657,-19.9630671442991,
0.955867870480223));
#45800=CARTESIAN_POINT('Ctrl Pts',(-3.38418026883877,-19.9628624663561,
0.962076519309465));
#45801=CARTESIAN_POINT('Ctrl Pts',(-3.36209246653124,-19.9626584445229,
0.968273515281171));
#45802=CARTESIAN_POINT('Ctrl Pts',(-3.35104856537748,-19.9625564336064,
0.971372013267024));
#45803=CARTESIAN_POINT('Ctrl Pts',(-3.33996130062377,-19.9624545867031,
0.974467598037997));
#45804=CARTESIAN_POINT('Ctrl Pts',(-3.32883061483636,-19.9623529153641,
0.977559928309276));
#45805=CARTESIAN_POINT('Ctrl Pts',(-3.32326527194265,-19.9623020796946,
0.979106093444916));
#45806=CARTESIAN_POINT('Ctrl Pts',(-3.31768907379052,-19.9622512879152,
0.980651444955594));
#45807=CARTESIAN_POINT('Ctrl Pts',(-3.31210201325294,-19.9622005414794,
0.982195939788543));
#45808=CARTESIAN_POINT('Ctrl Pts',(-3.30651495271535,-19.9621497950436,
0.983740434621492));
#45809=CARTESIAN_POINT('Ctrl Pts',(-3.30209405065048,-19.9621097238955,
0.984960324852798));
#45810=CARTESIAN_POINT('Ctrl Pts',(-3.29530823737352,-19.9620484396568,
0.986826811081932));
#45811=CARTESIAN_POINT('Ctrl Pts',(-3.26371351551596,-19.9617631004648,
0.995517164154379));
#45812=CARTESIAN_POINT('Ctrl Pts',(-3.23221976327874,-19.9614833155026,
1.00405525712431));
#45813=CARTESIAN_POINT('Ctrl Pts',(-3.20082837943391,-19.9612089854768,
1.01244306424384));
#45814=CARTESIAN_POINT('Ctrl Pts',(-3.02529692306615,-19.9596750120403,
1.05934523353657));
#45815=CARTESIAN_POINT('Ctrl Pts',(-2.85296934932615,-19.9583115521099,
1.10154715968608));
#45816=CARTESIAN_POINT('Ctrl Pts',(-2.68408332990121,-19.957101515053,1.13941645657479));
#45817=CARTESIAN_POINT('Ctrl Pts',(-2.50184473349649,-19.9557958092545,
1.18027980059422));
#45818=CARTESIAN_POINT('Ctrl Pts',(-2.32361410663327,-19.9546686989974,
1.21609906014452));
#45819=CARTESIAN_POINT('Ctrl Pts',(-2.14965775902324,-19.9536981810796,
1.24737014880551));
#45820=CARTESIAN_POINT('Ctrl Pts',(-2.13682704255917,-19.9536265973725,
1.24967664970441));
#45821=CARTESIAN_POINT('Ctrl Pts',(-2.12401955626893,-19.9535558661227,
1.25195841043766));
#45822=CARTESIAN_POINT('Ctrl Pts',(-2.1112353961309,-19.9534859787631,1.25421563135693));
#45823=CARTESIAN_POINT('Ctrl Pts',(-1.93625472138247,-19.952529409288,1.28511089825319));
#45824=CARTESIAN_POINT('Ctrl Pts',(-1.76564842135957,-19.9517307494261,
1.31140933237227));
#45825=CARTESIAN_POINT('Ctrl Pts',(-1.59964960695838,-19.9510660439799,
1.33364778692522));
#45826=CARTESIAN_POINT('Ctrl Pts',(-1.55747659209,-19.9508971714927,1.33929760242477));
#45827=CARTESIAN_POINT('Ctrl Pts',(-1.51560070355459,-19.9507369561823,
1.34468533408111));
#45828=CARTESIAN_POINT('Ctrl Pts',(-1.47402524339339,-19.9505850276501,
1.34981970536911));
#45829=CARTESIAN_POINT('Ctrl Pts',(-1.30954622608724,-19.9499839746354,
1.37013208052167));
#45830=CARTESIAN_POINT('Ctrl Pts',(-1.14977310823239,-19.9495123677062,
1.38648080161668));
#45831=CARTESIAN_POINT('Ctrl Pts',(-0.994888669132556,-19.9491460309321,
1.39942188067988));
#45832=CARTESIAN_POINT('Ctrl Pts',(-0.923054604482982,-19.9489761271015,
1.40542384133819));
#45833=CARTESIAN_POINT('Ctrl Pts',(-0.85227141748989,-19.9488289113757,
1.41069250714498));
#45834=CARTESIAN_POINT('Ctrl Pts',(-0.782553962151891,-19.9487021923061,
1.41528169882576));
#45835=CARTESIAN_POINT('Ctrl Pts',(-0.633225993292338,-19.9484307724559,
1.42511129844432));
#45836=CARTESIAN_POINT('Ctrl Pts',(-0.488789989415151,-19.9482530035993,
1.43182610541899));
#45837=CARTESIAN_POINT('Ctrl Pts',(-0.349367810876151,-19.948143898493,
1.43595869572865));
#45838=CARTESIAN_POINT('Ctrl Pts',(-0.262283845607513,-19.9480757507608,
1.43853993749927));
#45839=CARTESIAN_POINT('Ctrl Pts',(-0.177155096851432,-19.9480344970638,
1.44011308848701));
#45840=CARTESIAN_POINT('Ctrl Pts',(-0.0940037411794105,-19.948015009502,
1.44080102246092));
#45841=CARTESIAN_POINT('Ctrl Pts',(0.0408033074116613,-19.9479834157815,
1.44191631815152));
#45842=CARTESIAN_POINT('Ctrl Pts',(0.170411318462979,-19.9480093421139,
1.44070714992397));
#45843=CARTESIAN_POINT('Ctrl Pts',(0.294749903916067,-19.9480858766655,
1.43767293836567));
#45844=CARTESIAN_POINT('Ctrl Pts',(0.343180995220454,-19.9481156876195,
1.4364910833809));
#45845=CARTESIAN_POINT('Ctrl Pts',(0.390812983906775,-19.9481531567733,
1.43503190092335));
#45846=CARTESIAN_POINT('Ctrl Pts',(0.437643016283311,-19.9481978063411,
1.43332323677407));
#45847=CARTESIAN_POINT('Ctrl Pts',(0.474088859801895,-19.9482325552208,
1.43199345536992));
#45848=CARTESIAN_POINT('Ctrl Pts',(0.510048984651785,-19.9482716524046,
1.43051254789329));
#45849=CARTESIAN_POINT('Ctrl Pts',(0.545522325919625,-19.948314859256,1.42889324789818));
#45850=CARTESIAN_POINT('Ctrl Pts',(0.575342930585281,-19.948351181023,1.42753198608118));
#45851=CARTESIAN_POINT('Ctrl Pts',(0.604819536025602,-19.9483904067925,
1.42607291952875));
#45852=CARTESIAN_POINT('Ctrl Pts',(0.633951737248377,-19.9484323866779,
1.42452357218047));
#45853=CARTESIAN_POINT('Ctrl Pts',(0.665845060554363,-19.9484783453766,
1.42282737917692));
#45854=CARTESIAN_POINT('Ctrl Pts',(0.697325522058463,-19.948527604552,1.42102299411122));
#45855=CARTESIAN_POINT('Ctrl Pts',(0.728392805781448,-19.9485799624068,
1.41912001321096));
#45856=CARTESIAN_POINT('Ctrl Pts',(0.743926447642939,-19.9486061413342,
1.41816852276083));
#45857=CARTESIAN_POINT('Ctrl Pts',(0.759356795058225,-19.9486330945423,
1.41719238332444));
#45858=CARTESIAN_POINT('Ctrl Pts',(0.774683802833065,-19.9486607965246,
1.41619276610858));
#45859=CARTESIAN_POINT('Ctrl Pts',(0.782347306720485,-19.9486746475157,
1.41569295750065));
#45860=CARTESIAN_POINT('Ctrl Pts',(0.78998497569773,-19.948688685677,1.41518727944621));
#45861=CARTESIAN_POINT('Ctrl Pts',(0.797596805412144,-19.94870290775,1.41467587730628));
#45862=CARTESIAN_POINT('Ctrl Pts',(0.805208635126558,-19.948717129823,1.41416447516635));
#45863=CARTESIAN_POINT('Ctrl Pts',(0.81455809586776,-19.9487349382461,1.41352542345741));
#45864=CARTESIAN_POINT('Ctrl Pts',(0.820354772636643,-19.9487461223901,
1.41312464346554));
#45865=CARTESIAN_POINT('Ctrl Pts',(0.913219559701145,-19.9489252962841,
1.40670400797247));
#45866=CARTESIAN_POINT('Ctrl Pts',(1.01097505164935,-19.9491467067125,1.39886195763818));
#45867=CARTESIAN_POINT('Ctrl Pts',(1.1135640324211,-19.9494231953357,1.38924936584772));
#45868=CARTESIAN_POINT('Ctrl Pts',(1.22619399111071,-19.9497267455022,1.37869593400625));
#45869=CARTESIAN_POINT('Ctrl Pts',(1.34465071383681,-19.9500967037675,1.36600849025799));
#45870=CARTESIAN_POINT('Ctrl Pts',(1.46882938107773,-19.9505511703804,1.35069212718216));
#45871=CARTESIAN_POINT('Ctrl Pts',(1.51533015773198,-19.9507213529965,1.34495665913141));
#45872=CARTESIAN_POINT('Ctrl Pts',(1.56263295566258,-19.9509034123575,1.33885215798398));
#45873=CARTESIAN_POINT('Ctrl Pts',(1.6107309717886,-19.9510983971473,1.33235126464855));
#45874=CARTESIAN_POINT('Ctrl Pts',(1.74016072627675,-19.9516230930807,1.31485763193504));
#45875=CARTESIAN_POINT('Ctrl Pts',(1.87535188685385,-19.9522412101344,1.29449569857747));
#45876=CARTESIAN_POINT('Ctrl Pts',(2.01614804957389,-19.9529740117998,1.27071914141072));
#45877=CARTESIAN_POINT('Ctrl Pts',(2.02946099004117,-19.9530433016494,1.2684709559207));
#45878=CARTESIAN_POINT('Ctrl Pts',(2.04282401054921,-19.9531136187254,1.26619222015002));
#45879=CARTESIAN_POINT('Ctrl Pts',(2.05623695835842,-19.9531849821918,1.26388245908358));
#45880=CARTESIAN_POINT('Ctrl Pts',(2.18613474459512,-19.9538761021776,1.24151356198998));
#45881=CARTESIAN_POINT('Ctrl Pts',(2.32071794588983,-19.9546652443161,1.21623591885326));
#45882=CARTESIAN_POINT('Ctrl Pts',(2.45983349748496,-19.9555696850239,1.18761773855746));
#45883=CARTESIAN_POINT('Ctrl Pts',(2.57754555067168,-19.9563349738178,1.16340258272146));
#45884=CARTESIAN_POINT('Ctrl Pts',(2.69850206719957,-19.9571828472084,1.13679523393321));
#45885=CARTESIAN_POINT('Ctrl Pts',(2.82259417732612,-19.958124134521,1.10753308187823));
#45886=CARTESIAN_POINT('Ctrl Pts',(2.92928969165264,-19.958933461833,1.08237321989649));
#45887=CARTESIAN_POINT('Ctrl Pts',(3.03830297462944,-19.9598118612748,1.05525055320977));
#45888=CARTESIAN_POINT('Ctrl Pts',(3.14955604559989,-19.9607663936939,1.02599991467783));
#45889=CARTESIAN_POINT('Ctrl Pts',(3.24644396496343,-19.9615976755565,1.00052615936759));
#45890=CARTESIAN_POINT('Ctrl Pts',(3.34503044467376,-19.9624867037711,0.973438421394531));
#45891=CARTESIAN_POINT('Ctrl Pts',(3.44525913621966,-19.9634382995461,0.944629727965889));
#45892=CARTESIAN_POINT('Ctrl Pts',(3.44870611911616,-19.963471026047,0.943638963026355));
#45893=CARTESIAN_POINT('Ctrl Pts',(3.45215504374027,-19.9635038265659,0.942646162746129));
#45894=CARTESIAN_POINT('Ctrl Pts',(3.45560590773787,-19.963536701306,0.94165132284774));
#45895=CARTESIAN_POINT('Ctrl Pts',(3.53367153282903,-19.9642803953891,0.919146002850343));
#45896=CARTESIAN_POINT('Ctrl Pts',(3.61272983141187,-19.9650620670969,0.895596831425127));
#45897=CARTESIAN_POINT('Ctrl Pts',(3.69275236865053,-19.9658841047799,0.870954669388449));
#45898=CARTESIAN_POINT('Ctrl Pts',(3.69944558974584,-19.9659528614096,0.868893557050984));
#45899=CARTESIAN_POINT('Ctrl Pts',(3.706145556583,-19.9660219004815,0.866824798522152));
#45900=CARTESIAN_POINT('Ctrl Pts',(3.71285225154802,-19.966091223414,0.864748365335758));
#45901=CARTESIAN_POINT('Ctrl Pts',(3.74623737037075,-19.9664363046125,0.854412131316357));
#45902=CARTESIAN_POINT('Ctrl Pts',(3.77978921264104,-19.9667884194618,0.843885722316286));
#45903=CARTESIAN_POINT('Ctrl Pts',(3.81350561990606,-19.9671477526821,0.833165672987393));
#45904=CARTESIAN_POINT('Ctrl Pts',(3.83375044708249,-19.9673635122939,0.82672887963986));
#45905=CARTESIAN_POINT('Ctrl Pts',(3.8540546057761,-19.9675818744595,0.820222271796804));
#45906=CARTESIAN_POINT('Ctrl Pts',(3.87441762676972,-19.967802879636,0.813645104648946));
#45907=CARTESIAN_POINT('Ctrl Pts',(3.88459913726653,-19.9679133822243,0.810356521075018));
#45908=CARTESIAN_POINT('Ctrl Pts',(3.89479536333834,-19.968024545573,0.807050297675153));
#45909=CARTESIAN_POINT('Ctrl Pts',(3.90500624519459,-19.9681363747775,0.803726341583876));
#45910=CARTESIAN_POINT('Ctrl Pts',(3.91011168612271,-19.9681922893797,0.802064363538237));
#45911=CARTESIAN_POINT('Ctrl Pts',(3.91522079099694,-19.9682483704464,0.800397952319758));
#45912=CARTESIAN_POINT('Ctrl Pts',(3.92033355229372,-19.9683046186163,0.798727096350555));
#45913=CARTESIAN_POINT('Ctrl Pts',(3.92544631359051,-19.9683608667862,0.797056240381352));
#45914=CARTESIAN_POINT('Ctrl Pts',(3.93232800683171,-19.9684367905194,0.79480179993151));
#45915=CARTESIAN_POINT('Ctrl Pts',(3.9356827979111,-19.9684738650762,0.793701182621356));
#45916=CARTESIAN_POINT('Ctrl Pts',(3.94201776596352,-19.9685438742444,0.791622848879327));
#45917=CARTESIAN_POINT('Ctrl Pts',(3.94833529221475,-19.9686138847017,0.789545282538373));
#45918=CARTESIAN_POINT('Ctrl Pts',(3.95463539436655,-19.9686838938132,0.787468559316938));
#45919=CARTESIAN_POINT('Ctrl Pts',(4.02984793005298,-19.9695196838803,0.762676005856775));
#45920=CARTESIAN_POINT('Ctrl Pts',(4.10257711980881,-19.9703552659729,0.7380045802307));
#45921=CARTESIAN_POINT('Ctrl Pts',(4.1728536855241,-19.9711864277094,0.713576948003457));
#45922=CARTESIAN_POINT('Ctrl Pts',(4.24078041990787,-19.9719897979641,0.689966100361207));
#45923=CARTESIAN_POINT('Ctrl Pts',(4.30641583373046,-19.9727890443001,0.666582917234265));
#45924=CARTESIAN_POINT('Ctrl Pts',(4.36978780546687,-19.9735806927637,0.643528252680029));
#45925=CARTESIAN_POINT('Ctrl Pts',(4.43123718177006,-19.9743483239894,0.621173026561618));
#45926=CARTESIAN_POINT('Ctrl Pts',(4.49055838824294,-19.9751088167531,0.599126610536702));
#45927=CARTESIAN_POINT('Ctrl Pts',(4.54777651242298,-19.9758592774546,0.577472662590279));
#45928=CARTESIAN_POINT('Ctrl Pts',(4.60352991899979,-19.9765905272327,0.556373030591668));
#45929=CARTESIAN_POINT('Ctrl Pts',(4.65728654863231,-19.9773122570472,0.535645970642595));
#45930=CARTESIAN_POINT('Ctrl Pts',(4.70906899455022,-19.9780220136423,0.515361826729719));
#45931=CARTESIAN_POINT('Ctrl Pts',(4.75988646514747,-19.9787185437938,0.495455681536865));
#45932=CARTESIAN_POINT('Ctrl Pts',(4.80880265137162,-19.9794035476555,0.475976054196603));
#45933=CARTESIAN_POINT('Ctrl Pts',(4.85583810555937,-19.9800748867969,0.45698327080129));
#45934=CARTESIAN_POINT('Ctrl Pts',(4.90206734298214,-19.9807347187704,0.438316035455873));
#45935=CARTESIAN_POINT('Ctrl Pts',(4.94647977271578,-19.9813813550584,0.420119060257995));
#45936=CARTESIAN_POINT('Ctrl Pts',(4.9890939954169,-19.9820129039542,0.402444197157457));
#45937=CARTESIAN_POINT('Ctrl Pts',(4.98946317908515,-19.9820183753092,0.402291072909692));
#45938=CARTESIAN_POINT('Ctrl Pts',(4.98983222778481,-19.9820238455311,0.402137987816611));
#45939=CARTESIAN_POINT('Ctrl Pts',(4.9902011415277,-19.9820293146189,0.401984941910257));
#45940=CARTESIAN_POINT('Ctrl Pts',(5.03326624102464,-19.9826677478928,0.384119147231026));
#45941=CARTESIAN_POINT('Ctrl Pts',(5.0744923583959,-19.9832907382138,0.366787777783412));
#45942=CARTESIAN_POINT('Ctrl Pts',(5.11389765669138,-19.9838964340089,0.350039136630992));
#45943=CARTESIAN_POINT('Ctrl Pts',(5.15370169359892,-19.9845082587844,0.33312101750947));
#45944=CARTESIAN_POINT('Ctrl Pts',(5.19164787976516,-19.9851024422408,0.316797468369802));
#45945=CARTESIAN_POINT('Ctrl Pts',(5.22775373276918,-19.9856771422,0.301113068622864));
#45946=CARTESIAN_POINT('Ctrl Pts',(5.26453890956988,-19.9862626550142,0.285133570294995));
#45947=CARTESIAN_POINT('Ctrl Pts',(5.29941385696856,-19.9868279488227,0.269817495334042));
#45948=CARTESIAN_POINT('Ctrl Pts',(5.33239574607363,-19.9873710979507,0.255206700780277));
#45949=CARTESIAN_POINT('Ctrl Pts',(5.36640991150646,-19.987931246711,0.2401386135196));
#45950=CARTESIAN_POINT('Ctrl Pts',(5.39841067725307,-19.9884678461484,0.225820654257808));
#45951=CARTESIAN_POINT('Ctrl Pts',(5.42841530804753,-19.9889787612015,0.212293095298047));
#45952=CARTESIAN_POINT('Ctrl Pts',(5.4599627399709,-19.9895159468767,0.198069965931917));
#45953=CARTESIAN_POINT('Ctrl Pts',(5.48930350818925,-19.9900247389058,0.184720640340341));
#45954=CARTESIAN_POINT('Ctrl Pts',(5.51645571937383,-19.9905025966942,0.172285432958562));
#45955=CARTESIAN_POINT('Ctrl Pts',(5.54440396445813,-19.9909944640597,0.159485656866014));
#45956=CARTESIAN_POINT('Ctrl Pts',(5.57003347911907,-19.9914535484999,0.147654394959246));
#45957=CARTESIAN_POINT('Ctrl Pts',(5.59336166001797,-19.9918770419854,0.136828574222652));
#45958=CARTESIAN_POINT('Ctrl Pts',(-5.84637332561518,-19.8012032245096,
0.398518228706042));
#45959=CARTESIAN_POINT('Ctrl Pts',(-5.81071186290306,-19.8004233834171,
0.41520737060269));
#45960=CARTESIAN_POINT('Ctrl Pts',(-5.69191724351161,-19.797880036612,0.470271235481794));
#45961=CARTESIAN_POINT('Ctrl Pts',(-5.48049048458094,-19.7936450596294,
0.565146741690545));
#45962=CARTESIAN_POINT('Ctrl Pts',(-5.20214452284485,-19.7884998191918,
0.68405291707163));
#45963=CARTESIAN_POINT('Ctrl Pts',(-4.89413796055143,-19.7832359786177,
0.80835770933709));
#45964=CARTESIAN_POINT('Ctrl Pts',(-4.55276036907155,-19.7778647893813,
0.937269633545895));
#45965=CARTESIAN_POINT('Ctrl Pts',(-4.17237911340894,-19.7724099073617,
1.06997883011475));
#45966=CARTESIAN_POINT('Ctrl Pts',(-3.74657608413542,-19.7669368130706,
1.20488312141804));
#45967=CARTESIAN_POINT('Ctrl Pts',(-3.27004596375486,-19.7615847658559,
1.33873580301228));
#45968=CARTESIAN_POINT('Ctrl Pts',(-2.7387201600104,-19.7565630655646,1.4666394592086));
#45969=CARTESIAN_POINT('Ctrl Pts',(-2.14782149463107,-19.7521260156702,
1.58251297890624));
#45970=CARTESIAN_POINT('Ctrl Pts',(-1.49674277411264,-19.7486061536723,
1.6779232271702));
#45971=CARTESIAN_POINT('Ctrl Pts',(-0.805541188049843,-19.746389950329,
1.7416146737656));
#45972=CARTESIAN_POINT('Ctrl Pts',(-0.113422498758484,-19.7456264454589,
1.76632910849782));
#45973=CARTESIAN_POINT('Ctrl Pts',(0.536119675471227,-19.7459828406868,
1.75439019730121));
#45974=CARTESIAN_POINT('Ctrl Pts',(1.11982241639085,-19.7473094854822,1.71489595544031));
#45975=CARTESIAN_POINT('Ctrl Pts',(1.63691910409778,-19.7493621956864,1.65738874956046));
#45976=CARTESIAN_POINT('Ctrl Pts',(2.09764987887928,-19.7519182415327,1.58837871802467));
#45977=CARTESIAN_POINT('Ctrl Pts',(2.51229038328305,-19.7548277285975,1.51185825784502));
#45978=CARTESIAN_POINT('Ctrl Pts',(2.8862805445336,-19.7579580036799,1.43110355046616));
#45979=CARTESIAN_POINT('Ctrl Pts',(3.22330033713463,-19.7611952123647,1.34881182009632));
#45980=CARTESIAN_POINT('Ctrl Pts',(3.52771849241463,-19.7644627557382,1.26671644234715));
#45981=CARTESIAN_POINT('Ctrl Pts',(3.80296220780623,-19.7677012652864,1.18613702323411));
#45982=CARTESIAN_POINT('Ctrl Pts',(4.05167352309718,-19.7708626842596,1.10813376736068));
#45983=CARTESIAN_POINT('Ctrl Pts',(4.27619687672365,-19.7739112820015,1.03348278511119));
#45984=CARTESIAN_POINT('Ctrl Pts',(4.47888810581092,-19.7768251650753,0.962639383477481));
#45985=CARTESIAN_POINT('Ctrl Pts',(4.66210367547018,-19.7795944348557,0.895783474658922));
#45986=CARTESIAN_POINT('Ctrl Pts',(4.82816201172659,-19.782218972549,0.83287332055465));
#45987=CARTESIAN_POINT('Ctrl Pts',(4.9793040978404,-19.784706262591,0.77369827621928));
#45988=CARTESIAN_POINT('Ctrl Pts',(5.11759466992664,-19.7870683576696,0.717952243040958));
#45989=CARTESIAN_POINT('Ctrl Pts',(5.24463568621137,-19.7893154089871,0.665386419186038));
#45990=CARTESIAN_POINT('Ctrl Pts',(5.3615195899783,-19.7914527440325,0.615872671561029));
#45991=CARTESIAN_POINT('Ctrl Pts',(5.46894761080408,-19.7934811813725,0.569388237748869));
#45992=CARTESIAN_POINT('Ctrl Pts',(5.56755786506634,-19.795402135003,0.525892474641232));
#45993=CARTESIAN_POINT('Ctrl Pts',(5.65799402501198,-19.7972185803945,0.485302861498154));
#45994=CARTESIAN_POINT('Ctrl Pts',(5.74090216955938,-19.7989347556667,0.447500470475536));
#45995=CARTESIAN_POINT('Ctrl Pts',(5.80283684827997,-19.8002553617805,0.418853196576111));
#45996=CARTESIAN_POINT('Ctrl Pts',(5.83721009892043,-19.8010035313691,0.402805975572136));
#45997=CARTESIAN_POINT('Ctrl Pts',(5.84634760404617,-19.8012035243102,0.398529618156887));
#45998=CARTESIAN_POINT('Ctrl Pts',(-5.81214087242335,-19.9271873066255,
0.330204210423679));
#45999=CARTESIAN_POINT('Ctrl Pts',(-5.77669421382378,-19.9264341811936,
0.346835037585213));
#46000=CARTESIAN_POINT('Ctrl Pts',(-5.65860674649306,-19.9239789090011,
0.401710664034115));
#46001=CARTESIAN_POINT('Ctrl Pts',(-5.44839807624833,-19.9198953659561,
0.496281732480572));
#46002=CARTESIAN_POINT('Ctrl Pts',(-5.17161876013454,-19.9149409583558,
0.614825658279969));
#46003=CARTESIAN_POINT('Ctrl Pts',(-4.86533505608267,-19.909878877687,0.7387605376848));
#46004=CARTESIAN_POINT('Ctrl Pts',(-4.52587295649738,-19.9047199784787,
0.867291774518096));
#46005=CARTESIAN_POINT('Ctrl Pts',(-4.14764429923081,-19.8994872295208,
0.99960842331503));
#46006=CARTESIAN_POINT('Ctrl Pts',(-3.72427883488178,-19.8942438262849,
1.13411085093911));
#46007=CARTESIAN_POINT('Ctrl Pts',(-3.25051249031194,-19.8891235326155,
1.26756067629006));
#46008=CARTESIAN_POINT('Ctrl Pts',(-2.72230931503972,-19.8843266474812,
1.39507475420067));
#46009=CARTESIAN_POINT('Ctrl Pts',(-2.1349256811288,-19.8800956328736,1.51059101517757));
#46010=CARTESIAN_POINT('Ctrl Pts',(-1.48775542564675,-19.876746360621,1.60570392250982));
#46011=CARTESIAN_POINT('Ctrl Pts',(-0.800722870452506,-19.8746435601401,
1.66919556666686));
#46012=CARTESIAN_POINT('Ctrl Pts',(-0.112751530308937,-19.8739229914661,
1.69383291987766));
#46013=CARTESIAN_POINT('Ctrl Pts',(0.532923322865208,-19.8742588033861,
1.68193113155805));
#46014=CARTESIAN_POINT('Ctrl Pts',(1.11310674871294,-19.875515597709,1.64256070755316));
#46015=CARTESIAN_POINT('Ctrl Pts',(1.62709029937881,-19.8774656632708,1.58523349554965));
#46016=CARTESIAN_POINT('Ctrl Pts',(2.08505695577575,-19.8798984167727,1.51643825624151));
#46017=CARTESIAN_POINT('Ctrl Pts',(2.49722536838503,-19.8826716687465,1.44015424964475));
#46018=CARTESIAN_POINT('Ctrl Pts',(2.86900237522437,-19.8856590909154,1.35964711728455));
#46019=CARTESIAN_POINT('Ctrl Pts',(3.20404389672357,-19.8887519187439,1.27760569307259));
#46020=CARTESIAN_POINT('Ctrl Pts',(3.50668982756711,-19.8918767530765,1.1957581658858));
#46021=CARTESIAN_POINT('Ctrl Pts',(3.78034401648963,-19.8949765502608,1.11542038234925));
#46022=CARTESIAN_POINT('Ctrl Pts',(4.02762986002984,-19.8980050099384,1.03764968920657));
#46023=CARTESIAN_POINT('Ctrl Pts',(4.25087514579436,-19.9009275845067,0.963220264239793));
#46024=CARTESIAN_POINT('Ctrl Pts',(4.45241937565161,-19.9037229678009,0.89258647044243));
#46025=CARTESIAN_POINT('Ctrl Pts',(4.63460310816801,-19.9063813646969,0.825928096032151));
#46026=CARTESIAN_POINT('Ctrl Pts',(4.79972950250149,-19.9089023917319,0.763203922014176));
#46027=CARTESIAN_POINT('Ctrl Pts',(4.95002508592934,-19.9112930043664,0.704204306591428));
#46028=CARTESIAN_POINT('Ctrl Pts',(5.08754142435965,-19.9135645911091,0.648624430192096));
#46029=CARTESIAN_POINT('Ctrl Pts',(5.21387010188393,-19.9157267527803,0.596216606190617));
#46030=CARTESIAN_POINT('Ctrl Pts',(5.33009618357311,-19.9177844763503,0.546853461908779));
#46031=CARTESIAN_POINT('Ctrl Pts',(5.43691587105589,-19.9197384200799,0.500512656976851));
#46032=CARTESIAN_POINT('Ctrl Pts',(5.53496282016363,-19.9215898205621,0.457153966966406));
#46033=CARTESIAN_POINT('Ctrl Pts',(5.62487650603923,-19.9233414240886,0.416695315435241));
#46034=CARTESIAN_POINT('Ctrl Pts',(5.70729922003086,-19.9249972011021,0.379018161123265));
#46035=CARTESIAN_POINT('Ctrl Pts',(5.76886605586837,-19.9262719866521,0.350468412781502));
#46036=CARTESIAN_POINT('Ctrl Pts',(5.80303331086259,-19.9269944605838,0.33447675633162));
#46037=CARTESIAN_POINT('Ctrl Pts',(5.81211594933361,-19.927187604253,0.330215260750033));
#46038=CARTESIAN_POINT('Ctrl Pts',(-5.7563773441824,-19.9977612734129,0.213435765605445));
#46039=CARTESIAN_POINT('Ctrl Pts',(-5.72124284761157,-19.9970527865212,
0.229944522484756));
#46040=CARTESIAN_POINT('Ctrl Pts',(-5.60419033028892,-19.9947448867347,
0.284419868696954));
#46041=CARTESIAN_POINT('Ctrl Pts',(-5.39580264092759,-19.9909160146533,
0.378311890771256));
#46042=CARTESIAN_POINT('Ctrl Pts',(-5.12141647166683,-19.9862842137298,
0.496009003059121));
#46043=CARTESIAN_POINT('Ctrl Pts',(-4.81780583433225,-19.9815646423287,
0.61905163753994));
#46044=CARTESIAN_POINT('Ctrl Pts',(-4.48135309706814,-19.976767498175,0.746643501707943));
#46045=CARTESIAN_POINT('Ctrl Pts',(-4.10654376060317,-19.9719146709044,
0.877973972287787));
#46046=CARTESIAN_POINT('Ctrl Pts',(-3.68709091834991,-19.9670655738919,
1.01145112966721));
#46047=CARTESIAN_POINT('Ctrl Pts',(-3.21780670805486,-19.9623446304896,
1.14385873471159));
#46048=CARTESIAN_POINT('Ctrl Pts',(-2.69471979114672,-19.9579366090462,
1.27035198639089));
#46049=CARTESIAN_POINT('Ctrl Pts',(-2.113153523698,-19.9540632878202,1.38492123805317));
#46050=CARTESIAN_POINT('Ctrl Pts',(-1.47251555568381,-19.9510111884615,
1.47923787592944));
#46051=CARTESIAN_POINT('Ctrl Pts',(-0.792512707544035,-19.9491065172301,
1.54218975145515));
#46052=CARTESIAN_POINT('Ctrl Pts',(-0.111600877674484,-19.9484611334256,
1.56661679030302));
#46053=CARTESIAN_POINT('Ctrl Pts',(0.527465568453815,-19.9487608876799,
1.55481654016177));
#46054=CARTESIAN_POINT('Ctrl Pts',(1.10169493934809,-19.9498955386969,1.5157817092239));
#46055=CARTESIAN_POINT('Ctrl Pts',(1.61044354822359,-19.9516664740186,1.45893909693094));
#46056=CARTESIAN_POINT('Ctrl Pts',(2.0637940430478,-19.9538845323556,1.39071840306173));
#46057=CARTESIAN_POINT('Ctrl Pts',(2.47186151969891,-19.956421103771,1.31506249690282));
#46058=CARTESIAN_POINT('Ctrl Pts',(2.8399917317103,-19.9591609446546,1.23520815727489));
#46059=CARTESIAN_POINT('Ctrl Pts',(3.17179488226422,-19.9620041439025,1.15382165859323));
#46060=CARTESIAN_POINT('Ctrl Pts',(3.47155832017755,-19.9648828221612,1.07261750478866));
#46061=CARTESIAN_POINT('Ctrl Pts',(3.74264328259959,-19.9677439052293,0.992901886387031));
#46062=CARTESIAN_POINT('Ctrl Pts',(3.98763901532054,-19.9705440558936,0.915725050081919));
#46063=CARTESIAN_POINT('Ctrl Pts',(4.20884309016115,-19.9732506878429,0.841856595879339));
#46064=CARTESIAN_POINT('Ctrl Pts',(4.40856598483163,-19.9758434281717,0.771748892091009));
#46065=CARTESIAN_POINT('Ctrl Pts',(4.58912056827828,-19.9783125889059,0.705581797064866));
#46066=CARTESIAN_POINT('Ctrl Pts',(4.75278392458491,-19.9806572720839,0.643315711772626));
#46067=CARTESIAN_POINT('Ctrl Pts',(4.90175832814151,-19.982883478262,0.584743714215282));
#46068=CARTESIAN_POINT('Ctrl Pts',(5.03807359660553,-19.9850014227761,0.529564249821708));
#46069=CARTESIAN_POINT('Ctrl Pts',(5.16330433238403,-19.9870197378106,0.477532360449496));
#46070=CARTESIAN_POINT('Ctrl Pts',(5.27852354539555,-19.9889428058235,0.428522451677135));
#46071=CARTESIAN_POINT('Ctrl Pts',(5.38441915349035,-19.9907709904362,0.382513134578401));
#46072=CARTESIAN_POINT('Ctrl Pts',(5.48161746205723,-19.992505207299,0.339465166211689));
#46073=CARTESIAN_POINT('Ctrl Pts',(5.57075099051052,-19.9941477956291,0.299297609682865));
#46074=CARTESIAN_POINT('Ctrl Pts',(5.65245559258702,-19.9957022530114,0.26189312047201));
#46075=CARTESIAN_POINT('Ctrl Pts',(5.71348329895462,-19.9969003461367,0.233551396585078));
#46076=CARTESIAN_POINT('Ctrl Pts',(5.74735040689118,-19.9975798766668,0.217676759133368));
#46077=CARTESIAN_POINT('Ctrl Pts',(5.75635321179484,-19.997761577835,0.213446472193785));
#46078=CARTESIAN_POINT('Ctrl Pts',(-5.69417817153309,-19.9936700926002,
0.0798164952284382));
#46079=CARTESIAN_POINT('Ctrl Pts',(-5.65936864913364,-19.993012084528,0.0961724409863023));
#46080=CARTESIAN_POINT('Ctrl Pts',(-5.54339858366178,-19.9908709649436,
0.150143718198236));
#46081=CARTESIAN_POINT('Ctrl Pts',(-5.33694163762173,-19.9873310692217,
0.243165701629514));
#46082=CARTESIAN_POINT('Ctrl Pts',(-5.0651271037478,-19.9830663309066,0.359760385930429));
#46083=CARTESIAN_POINT('Ctrl Pts',(-4.7644159818022,-19.978737314844,0.48162965459219));
#46084=CARTESIAN_POINT('Ctrl Pts',(-4.43125170591844,-19.9743534799028,
0.607977396601455));
#46085=CARTESIAN_POINT('Ctrl Pts',(-4.06020269022993,-19.9699355366651,
0.737994634112659));
#46086=CARTESIAN_POINT('Ctrl Pts',(-3.64507829848936,-19.9655386431136,
0.870100245942965));
#46087=CARTESIAN_POINT('Ctrl Pts',(-3.18078122531583,-19.9612765652182,
1.00110796921292));
#46088=CARTESIAN_POINT('Ctrl Pts',(-2.66341923623205,-19.9573162141937,
1.1262250575769));
#46089=CARTESIAN_POINT('Ctrl Pts',(-2.08839798589795,-19.9538554399291,
1.23951350128208));
#46090=CARTESIAN_POINT('Ctrl Pts',(-1.45514799386454,-19.95114667215,1.33275014651456));
#46091=CARTESIAN_POINT('Ctrl Pts',(-0.783132822868955,-19.9494712370586,
1.39496816565624));
#46092=CARTESIAN_POINT('Ctrl Pts',(-0.110281963156994,-19.9489129397822,
1.41910849568614));
#46093=CARTESIAN_POINT('Ctrl Pts',(0.521223569921493,-19.9491709201523,
1.40744675804296));
#46094=CARTESIAN_POINT('Ctrl Pts',(1.08867568765767,-19.9501641904296,1.36886859839447));
#46095=CARTESIAN_POINT('Ctrl Pts',(1.59148448876097,-19.9517279879307,1.31268422210672));
#46096=CARTESIAN_POINT('Ctrl Pts',(2.03961626718321,-19.9536980517254,1.24524254578414));
#46097=CARTESIAN_POINT('Ctrl Pts',(2.44306402237904,-19.9559615511016,1.17043662862498));
#46098=CARTESIAN_POINT('Ctrl Pts',(2.80710095593827,-19.9584160870507,1.09146386419318));
#46099=CARTESIAN_POINT('Ctrl Pts',(3.13528225918272,-19.9609719694098,1.01095989522807));
#46100=CARTESIAN_POINT('Ctrl Pts',(3.43183324401102,-19.963567664804,0.930620741221009));
#46101=CARTESIAN_POINT('Ctrl Pts',(3.70006480313533,-19.9661546387235,0.851739649889142));
#46102=CARTESIAN_POINT('Ctrl Pts',(3.94252576462863,-19.9686929218185,0.77535744497962));
#46103=CARTESIAN_POINT('Ctrl Pts',(4.16147809566364,-19.9711521364158,0.702237741174908));
#46104=CARTESIAN_POINT('Ctrl Pts',(4.35919841515776,-19.97351293619,0.632830400882521));
#46105=CARTESIAN_POINT('Ctrl Pts',(4.53796761308272,-19.9757657149123,0.567315528008788));
#46106=CARTESIAN_POINT('Ctrl Pts',(4.70003294752602,-19.9779089494471,0.505655806689799));
#46107=CARTESIAN_POINT('Ctrl Pts',(4.8475692076678,-19.9799475179402,0.44764801631894));
#46108=CARTESIAN_POINT('Ctrl Pts',(4.98258177188227,-19.9818902710195,0.392994970754419));
#46109=CARTESIAN_POINT('Ctrl Pts',(5.10662625027061,-19.9837447161293,0.341455316020886));
#46110=CARTESIAN_POINT('Ctrl Pts',(5.220762183999,-19.985514530804,0.292905773024752));
#46111=CARTESIAN_POINT('Ctrl Pts',(5.32566819366107,-19.9871997294046,0.24732617640553));
#46112=CARTESIAN_POINT('Ctrl Pts',(5.42196233400887,-19.9888008499558,0.204678562150652));
#46113=CARTESIAN_POINT('Ctrl Pts',(5.51026929291715,-19.9903197568625,0.164883520156243));
#46114=CARTESIAN_POINT('Ctrl Pts',(5.59121757885841,-19.991759397639,0.127825389454448));
#46115=CARTESIAN_POINT('Ctrl Pts',(5.65168088095001,-19.9928706851653,0.0997459306861807));
#46116=CARTESIAN_POINT('Ctrl Pts',(5.68523498108013,-19.9935016482941,0.0840181187176475));
#46117=CARTESIAN_POINT('Ctrl Pts',(5.69415460745399,-19.9936704109565,0.0798269467380955));
#46118=CARTESIAN_POINT('',(5.73644274981144,-19.808949593799,0.442545696620674));
#46119=CARTESIAN_POINT('Origin',(5.599999999773,-19.591934376757,0.135488061232669));
#46120=CARTESIAN_POINT('Ctrl Pts',(-5.73644387793174,-19.8089519016381,
0.442549068206041));
#46121=CARTESIAN_POINT('Ctrl Pts',(-5.66411038140175,-19.8074370301154,
0.475761117952496));
#46122=CARTESIAN_POINT('Ctrl Pts',(-5.58548128727225,-19.8058476858708,
0.511218927486439));
#46123=CARTESIAN_POINT('Ctrl Pts',(-5.50055659392378,-19.80419803833,0.548567705601548));
#46124=CARTESIAN_POINT('Ctrl Pts',(-5.41741954148235,-19.8025831154059,
0.585130302442944));
#46125=CARTESIAN_POINT('Ctrl Pts',(-5.32824914148616,-19.8009104085098,
0.623504910589953));
#46126=CARTESIAN_POINT('Ctrl Pts',(-5.23304539241587,-19.7991952413925,
0.663306052555013));
#46127=CARTESIAN_POINT('Ctrl Pts',(-5.13477098872149,-19.7974247541235,
0.704390920862915));
#46128=CARTESIAN_POINT('Ctrl Pts',(-5.03006776621619,-19.7956090117036,
0.746996134649694));
#46129=CARTESIAN_POINT('Ctrl Pts',(-4.91893572322883,-19.7937671144692,
0.790639472565173));
#46130=CARTESIAN_POINT('Ctrl Pts',(-4.80780368024147,-19.7919252172349,
0.834282810480652));
#46131=CARTESIAN_POINT('Ctrl Pts',(-4.69024281677204,-19.7900571649709,
0.878964276341194));
#46132=CARTESIAN_POINT('Ctrl Pts',(-4.56625313114939,-19.7881843414101,
0.924142444101347));
#46133=CARTESIAN_POINT('Ctrl Pts',(-4.44622756681731,-19.786371394602,0.96787620351586));
#46134=CARTESIAN_POINT('Ctrl Pts',(-4.3201776876802,-19.7845539879721,1.01207512388596));
#46135=CARTESIAN_POINT('Ctrl Pts',(-4.18810349373807,-19.7827535612779,
1.05619516429525));
#46136=CARTESIAN_POINT('Ctrl Pts',(-4.05161761231589,-19.7808929947511,
1.1017889508171));
#46137=CARTESIAN_POINT('Ctrl Pts',(-3.90869823277936,-19.7790505488329,
1.14729881956836));
#46138=CARTESIAN_POINT('Ctrl Pts',(-3.75934535512849,-19.7772521442393,
1.19206590678836));
#46139=CARTESIAN_POINT('Ctrl Pts',(-3.60999247747762,-19.7754537396457,
1.23683299400836));
#46140=CARTESIAN_POINT('Ctrl Pts',(-3.45420610171241,-19.773699375747,1.28085730551268));
#46141=CARTESIAN_POINT('Ctrl Pts',(-3.29198622783285,-19.7720172785995,
1.32342047204876));
#46142=CARTESIAN_POINT('Ctrl Pts',(-3.21175020715356,-19.7711852918751,
1.34447275762075));
#46143=CARTESIAN_POINT('Ctrl Pts',(-3.12994028410414,-19.7703710201625,
1.36516666911119));
#46144=CARTESIAN_POINT('Ctrl Pts',(-3.04655646337055,-19.7695781029454,
1.38540988355588));
#46145=CARTESIAN_POINT('Ctrl Pts',(-3.00486455300375,-19.7691816443369,
1.39553149077823));
#46146=CARTESIAN_POINT('Ctrl Pts',(-2.96277915948905,-19.7687905006953,
1.40554038637855));
#46147=CARTESIAN_POINT('Ctrl Pts',(-2.92030029408361,-19.7684051710099,
1.41542467313665));
#46148=CARTESIAN_POINT('Ctrl Pts',(-2.89906086138089,-19.7682125061672,
1.4203668165157));
#46149=CARTESIAN_POINT('Ctrl Pts',(-2.87772306013855,-19.7680212933365,
1.42527780536093));
#46150=CARTESIAN_POINT('Ctrl Pts',(-2.85628689020884,-19.7678315911959,
1.43015613482796));
#46151=CARTESIAN_POINT('Ctrl Pts',(-2.84556880524398,-19.7677367401257,
1.43259529956148));
#46152=CARTESIAN_POINT('Ctrl Pts',(-2.83482612807483,-19.7676422666352,
1.43502629930336));
#46153=CARTESIAN_POINT('Ctrl Pts',(-2.8240588586925,-19.7675481781346,1.43744894462185));
#46154=CARTESIAN_POINT('Ctrl Pts',(-2.81867522400134,-19.7675011338842,
1.4386602672811));
#46155=CARTESIAN_POINT('Ctrl Pts',(-2.81328544125487,-19.7674541858755,
1.43986950132529));
#46156=CARTESIAN_POINT('Ctrl Pts',(-2.80788951045314,-19.7674073350413,
1.44107662299125));
#46157=CARTESIAN_POINT('Ctrl Pts',(-2.80249357965141,-19.7673604842071,
1.44228374465721));
#46158=CARTESIAN_POINT('Ctrl Pts',(-2.79531854980412,-19.7672984356932,
1.44388308559887));
#46159=CARTESIAN_POINT('Ctrl Pts',(-2.79168327387814,-19.7672670749844,
1.44469162704568));
#46160=CARTESIAN_POINT('Ctrl Pts',(-2.04596901439503,-19.7608339655671,
1.61054998237992));
#46161=CARTESIAN_POINT('Ctrl Pts',(-1.30026709200512,-19.7571553182439,
1.70987224350879));
#46162=CARTESIAN_POINT('Ctrl Pts',(-0.554547850970883,-19.7562174227089,
1.7426256094221));
#46163=CARTESIAN_POINT('Ctrl Pts',(-0.369699781998668,-19.7559849381906,
1.75074447790271));
#46164=CARTESIAN_POINT('Ctrl Pts',(-0.184850648900509,-19.7559209178912,
1.75477284736426));
#46165=CARTESIAN_POINT('Ctrl Pts',(3.10862446895044E-14,-19.7560252757495,
1.75470973948686));
#46166=CARTESIAN_POINT('Ctrl Pts',(6.95448532179484E-5,-19.7560253150112,
1.7547097157443));
#46167=CARTESIAN_POINT('Ctrl Pts',(0.00013908970661878,-19.7560253542967,
1.75470969142261));
#46168=CARTESIAN_POINT('Ctrl Pts',(0.000208634560234102,-19.7560253936061,
1.7547096665218));
#46169=CARTESIAN_POINT('Ctrl Pts',(0.465533558834944,-19.7562884127967,
1.75454305511928));
#46170=CARTESIAN_POINT('Ctrl Pts',(0.930858482087836,-19.7573599746889,
1.7286044125423));
#46171=CARTESIAN_POINT('Ctrl Pts',(1.39618340431891,-19.759242170924,1.67690524758153));
#46172=CARTESIAN_POINT('Ctrl Pts',(1.62884586543444,-19.7601832690415,1.65105566510115));
#46173=CARTESIAN_POINT('Ctrl Pts',(1.86150832640128,-19.7613268920606,1.61876628003846));
#46174=CARTESIAN_POINT('Ctrl Pts',(2.09417078585734,-19.7626724996003,1.58004052341054));
#46175=CARTESIAN_POINT('Ctrl Pts',(2.21050201558537,-19.7633453033701,1.56067764509659));
#46176=CARTESIAN_POINT('Ctrl Pts',(2.32683324685238,-19.7640686101838,1.53970568504067));
#46177=CARTESIAN_POINT('Ctrl Pts',(2.44316447733886,-19.7648422853926,1.51712520929198));
#46178=CARTESIAN_POINT('Ctrl Pts',(2.5013300925821,-19.7652291229971,1.50583497141763));
#46179=CARTESIAN_POINT('Ctrl Pts',(2.55949570773314,-19.7656285531405,1.49414260533559));
#46180=CARTESIAN_POINT('Ctrl Pts',(2.61766132280996,-19.7660405585964,1.48204818801444));
#46181=CARTESIAN_POINT('Ctrl Pts',(2.64674413034836,-19.7662465613244,1.47600097935386));
#46182=CARTESIAN_POINT('Ctrl Pts',(2.67582693787725,-19.7664557079078,1.46985325792706));
#46183=CARTESIAN_POINT('Ctrl Pts',(2.70490974539835,-19.7666679959892,1.46360503385831));
#46184=CARTESIAN_POINT('Ctrl Pts',(2.73217487744938,-19.7668670160654,1.45774732379385));
#46185=CARTESIAN_POINT('Ctrl Pts',(2.75944000949386,-19.7670687972249,1.45180128133079));
#46186=CARTESIAN_POINT('Ctrl Pts',(2.78670514153807,-19.7672733374521,1.44576691505616));
#46187=CARTESIAN_POINT('Ctrl Pts',(2.78852281700768,-19.7672869734672,1.44536462397119));
#46188=CARTESIAN_POINT('Ctrl Pts',(2.79172281222576,-19.7673110104151,1.44465540587742));
#46189=CARTESIAN_POINT('Ctrl Pts',(2.79215816794666,-19.7673142822828,1.4445588641543));
#46190=CARTESIAN_POINT('Ctrl Pts',(2.80635173261917,-19.7674209524462,1.44141138928538));
#46191=CARTESIAN_POINT('Ctrl Pts',(2.82657059814034,-19.7675848511013,1.43690103084202));
#46192=CARTESIAN_POINT('Ctrl Pts',(2.85281476451015,-19.7678094469751,1.43094042386484));
#46193=CARTESIAN_POINT('Ctrl Pts',(2.87905922487078,-19.7680340453649,1.42497975011611));
#46194=CARTESIAN_POINT('Ctrl Pts',(2.91132912107335,-19.7683193421491,1.41756879525677));
#46195=CARTESIAN_POINT('Ctrl Pts',(2.94962445311786,-19.768670883477,1.40856810271974));
#46196=CARTESIAN_POINT('Ctrl Pts',(2.9879202384843,-19.7690224289664,1.39956730363679));
#46197=CARTESIAN_POINT('Ctrl Pts',(3.03224160234602,-19.769440220275,1.38897672914351));
#46198=CARTESIAN_POINT('Ctrl Pts',(3.08258854470301,-19.7699318846709,1.37660482945053));
#46199=CARTESIAN_POINT('Ctrl Pts',(3.13293647355783,-19.7704235587004,1.36423268734258));
#46200=CARTESIAN_POINT('Ctrl Pts',(3.18931021704058,-19.7709891083087,1.35007915018452));
#46201=CARTESIAN_POINT('Ctrl Pts',(3.25170977515124,-19.77163824743,1.3339005678628));
#46202=CARTESIAN_POINT('Ctrl Pts',(3.31411003816818,-19.7722873938844,1.31772180277722));
#46203=CARTESIAN_POINT('Ctrl Pts',(3.38253625195691,-19.7730201312322,1.29951794664595));
#46204=CARTESIAN_POINT('Ctrl Pts',(3.45698841651743,-19.7738482668148,1.27899325277008));
#46205=CARTESIAN_POINT('Ctrl Pts',(3.53144199947791,-19.7746764181744,1.25846816787501));
#46206=CARTESIAN_POINT('Ctrl Pts',(3.61192176281505,-19.7755999707861,1.2356221567306));
#46207=CARTESIAN_POINT('Ctrl Pts',(3.69842770652883,-19.7766328342588,1.21010736714599));
#46208=CARTESIAN_POINT('Ctrl Pts',(3.77372504312439,-19.7775318692293,1.18789853828361));
#46209=CARTESIAN_POINT('Ctrl Pts',(3.85358810166981,-19.778513755189,1.16366691832388));
#46210=CARTESIAN_POINT('Ctrl Pts',(3.93801688216508,-19.7795889672883,1.13715098203608));
#46211=CARTESIAN_POINT('Ctrl Pts',(3.98561589130771,-19.7801951471981,1.122201905591));
#46212=CARTESIAN_POINT('Ctrl Pts',(4.03466609031313,-19.7808310122523,1.1065262314541));
#46213=CARTESIAN_POINT('Ctrl Pts',(4.0851674847676,-19.7814986223688,1.09007289718878));
#46214=CARTESIAN_POINT('Ctrl Pts',(4.11041818199483,-19.7818324274271,1.08184623005612));
#46215=CARTESIAN_POINT('Ctrl Pts',(4.1360316685357,-19.7821741490636,1.07342511796124));
#46216=CARTESIAN_POINT('Ctrl Pts',(4.16200795649282,-19.7825240823293,1.06480287426906));
#46217=CARTESIAN_POINT('Ctrl Pts',(4.17499610047137,-19.7826990489621,1.06049175242297));
#46218=CARTESIAN_POINT('Ctrl Pts',(4.18807494421639,-19.7828760672703,1.05613034579871));
#46219=CARTESIAN_POINT('Ctrl Pts',(4.20124448757875,-19.7830551710674,1.05171780388577));
#46220=CARTESIAN_POINT('Ctrl Pts',(4.20782925925993,-19.783144722966,1.0495115329293));
#46221=CARTESIAN_POINT('Ctrl Pts',(4.21443670580743,-19.78323479616,1.04729247803444));
#46222=CARTESIAN_POINT('Ctrl Pts',(4.22106682722272,-19.7833253949677,1.04506053174477));
#46223=CARTESIAN_POINT('Ctrl Pts',(4.22769694863801,-19.7834159937755,1.04282858545509));
#46224=CARTESIAN_POINT('Ctrl Pts',(4.23593845356822,-19.7835289311228,1.04004640064536));
#46225=CARTESIAN_POINT('Ctrl Pts',(4.24102521599583,-19.7835987724094,1.03832591063626));
#46226=CARTESIAN_POINT('Ctrl Pts',(4.37039632198203,-19.7853750386718,0.994568865072864));
#46227=CARTESIAN_POINT('Ctrl Pts',(4.49374157185689,-19.7871644886092,0.95084303173788));
#46228=CARTESIAN_POINT('Ctrl Pts',(4.61106096691901,-19.788946139999,0.907680881245061));
#46229=CARTESIAN_POINT('Ctrl Pts',(4.72934383257832,-19.7907424229741,0.86416426708586));
#46230=CARTESIAN_POINT('Ctrl Pts',(4.84150146389165,-19.7925307763442,0.821220700844053));
#46231=CARTESIAN_POINT('Ctrl Pts',(4.94753386218982,-19.7942917673862,0.779342300060695));
#46232=CARTESIAN_POINT('Ctrl Pts',(5.05275938615735,-19.7960393578216,0.737782581181571));
#46233=CARTESIAN_POINT('Ctrl Pts',(5.15195254473685,-19.7977600036065,0.69727180802215));
#46234=CARTESIAN_POINT('Ctrl Pts',(5.24511333922899,-19.799436732092,0.658238623808673));
#46235=CARTESIAN_POINT('Ctrl Pts',(5.33934567583654,-19.8011327464283,0.618756477121113));
#46236=CARTESIAN_POINT('Ctrl Pts',(5.42740608092356,-19.8027838235402,0.58078620540688));
#46237=CARTESIAN_POINT('Ctrl Pts',(5.50929455583613,-19.8043744898071,0.54471720648797));
#46238=CARTESIAN_POINT('Ctrl Pts',(5.5911830307487,-19.805965156074,0.508648207569059));
#46239=CARTESIAN_POINT('Ctrl Pts',(5.66689957548683,-19.807495411507,0.474480479178912));
#46240=CARTESIAN_POINT('Ctrl Pts',(5.73644419139658,-19.8089518848396,0.442548940790224));
#46241=CARTESIAN_POINT('Origin',(5.6,-19.5919343769583,0.135488060981343));
#46242=CARTESIAN_POINT('Origin',(5.59997427801439,-19.5919309020471,0.135464036486979));
#46243=CARTESIAN_POINT('Ctrl Pts',(5.71133811337302,-10.3755286010609,1.73145257720377));
#46244=CARTESIAN_POINT('Ctrl Pts',(5.75152712774209,-10.3630818178758,1.71508837504171));
#46245=CARTESIAN_POINT('Ctrl Pts',(5.83253386184225,-10.339510644463,1.66946189472995));
#46246=CARTESIAN_POINT('Ctrl Pts',(5.93556513369406,-10.3144216017685,1.56983798684213));
#46247=CARTESIAN_POINT('Ctrl Pts',(6.0101868944103,-10.3020933870588,1.44730328144741));
#46248=CARTESIAN_POINT('Ctrl Pts',(6.0464526344208,-10.3029959215501,1.32878328478311));
#46249=CARTESIAN_POINT('Ctrl Pts',(6.05178037288678,-10.3097270187875,1.25604070393047));
#46250=CARTESIAN_POINT('Ctrl Pts',(6.05105514091469,-10.3135670567819,1.22629617474195));
#46251=CARTESIAN_POINT('Ctrl Pts',(5.59496958662951,-10.0914744550291,1.65476262870179));
#46252=CARTESIAN_POINT('Ctrl Pts',(5.6324300295316,-10.079786670298,1.63972737512157));
#46253=CARTESIAN_POINT('Ctrl Pts',(5.70803679797223,-10.0575373066719,1.59779561973394));
#46254=CARTESIAN_POINT('Ctrl Pts',(5.8042440459682,-10.0335959394155,1.50625015057469));
#46255=CARTESIAN_POINT('Ctrl Pts',(5.87377408174617,-10.0215572105226,1.39395818247593));
#46256=CARTESIAN_POINT('Ctrl Pts',(5.90737675075672,-10.0219742604469,1.28598673146488));
#46257=CARTESIAN_POINT('Ctrl Pts',(5.91225807786315,-10.0279912265321,1.22030099419056));
#46258=CARTESIAN_POINT('Ctrl Pts',(5.91159342033835,-10.0314515024023,1.19357093143111));
#46259=CARTESIAN_POINT('Ctrl Pts',(5.57745794489003,-9.81893181439426,1.81452368423867));
#46260=CARTESIAN_POINT('Ctrl Pts',(5.63078003213836,-9.80260188831539,1.7933090225621));
#46261=CARTESIAN_POINT('Ctrl Pts',(5.73752235044812,-9.77206798166216,1.73458079337837));
#46262=CARTESIAN_POINT('Ctrl Pts',(5.87296120872625,-9.74001612997592,1.60722602071493));
#46263=CARTESIAN_POINT('Ctrl Pts',(5.97215523450811,-9.72435725886636,1.44946063567694));
#46264=CARTESIAN_POINT('Ctrl Pts',(6.02175241241746,-9.7257043359174,1.29349598934462));
#46265=CARTESIAN_POINT('Ctrl Pts',(6.02944537147473,-9.73486110115558,1.19446719239946));
#46266=CARTESIAN_POINT('Ctrl Pts',(6.02839959740249,-9.74017965350145,1.15322607941975));
#46267=CARTESIAN_POINT('Ctrl Pts',(5.67031557196363,-9.7370756153637,2.10570536871782));
#46268=CARTESIAN_POINT('Ctrl Pts',(5.74766173694799,-9.71375425056511,2.07486541692242));
#46269=CARTESIAN_POINT('Ctrl Pts',(5.90160594775961,-9.67077588277422,1.98989187537063));
#46270=CARTESIAN_POINT('Ctrl Pts',(6.09654035518264,-9.62668739149764,1.80638185716079));
#46271=CARTESIAN_POINT('Ctrl Pts',(6.24065234784129,-9.60587870824828,1.577322095495));
#46272=CARTESIAN_POINT('Ctrl Pts',(6.31438648424582,-9.60895990411399,1.34637426317501));
#46273=CARTESIAN_POINT('Ctrl Pts',(6.32630069195067,-9.6230462278461,1.19552294162878));
#46274=CARTESIAN_POINT('Ctrl Pts',(6.32468266445671,-9.63123942470839,1.13178513551015));
#46275=CARTESIAN_POINT('',(5.99999999999901,-10.0933615553116,1.21101376485454));
#46276=CARTESIAN_POINT('',(5.99999927107837,-9.65439083358236,1.8624630218698));
#46277=CARTESIAN_POINT('Ctrl Pts',(5.99998770355867,-10.0933615554491,1.21101376294399));
#46278=CARTESIAN_POINT('Ctrl Pts',(5.99998389443016,-10.0741186879649,1.2256833335264));
#46279=CARTESIAN_POINT('Ctrl Pts',(5.99998390164969,-10.0552448950568,1.2406862381206));
#46280=CARTESIAN_POINT('Ctrl Pts',(5.99999784523119,-10.0368574489198,1.25602792947848));
#46281=CARTESIAN_POINT('Ctrl Pts',(6.00000835464427,-10.0229986518209,1.26759111155923));
#46282=CARTESIAN_POINT('Ctrl Pts',(6.0000254843442,-10.009416316904,1.27934608106548));
#46283=CARTESIAN_POINT('Ctrl Pts',(6.00004217340985,-9.99615755794859,1.29127967956365));
#46284=CARTESIAN_POINT('Ctrl Pts',(6.00006539524908,-9.97770878583298,1.30788456995736));
#46285=CARTESIAN_POINT('Ctrl Pts',(6.00008857477621,-9.95988747126659,1.32483689381485));
#46286=CARTESIAN_POINT('Ctrl Pts',(6.00010759262717,-9.94279223481774,1.34206757541617));
#46287=CARTESIAN_POINT('Ctrl Pts',(6.00011528625985,-9.93587639189722,1.34903821239592));
#46288=CARTESIAN_POINT('Ctrl Pts',(6.00012209870678,-9.92907912135122,1.356053879453));
#46289=CARTESIAN_POINT('Ctrl Pts',(6.00012731958345,-9.92240574123668,1.36310798860156));
#46290=CARTESIAN_POINT('Ctrl Pts',(6.0001405716832,-9.90546676629374,1.38101336429743));
#46291=CARTESIAN_POINT('Ctrl Pts',(6.00014254779794,-9.8893288051776,1.39916896132706));
#46292=CARTESIAN_POINT('Ctrl Pts',(6.000126590469,-9.87405375348299,1.41743989761469));
#46293=CARTESIAN_POINT('Ctrl Pts',(6.00011864155799,-9.86644470894263,1.42654129843389));
#46294=CARTESIAN_POINT('Ctrl Pts',(6.0001064336008,-9.8590491939023,1.4356707588169));
#46295=CARTESIAN_POINT('Ctrl Pts',(6.00009082199952,-9.85187121335682,1.44480893859278));
#46296=CARTESIAN_POINT('Ctrl Pts',(6.00008441100787,-9.84892353537432,1.44856158338677));
#46297=CARTESIAN_POINT('Ctrl Pts',(6.0000781550863,-9.84599792430372,1.45233257340954));
#46298=CARTESIAN_POINT('Ctrl Pts',(6.00007171917567,-9.84310110032392,1.45611438476854));
#46299=CARTESIAN_POINT('Ctrl Pts',(6.00005349850847,-9.83489991967,1.46682104777966));
#46300=CARTESIAN_POINT('Ctrl Pts',(6.00003298876159,-9.8269318828134,1.47761727587867));
#46301=CARTESIAN_POINT('Ctrl Pts',(6.00001091572104,-9.81932764534066,1.4883072411331));
#46302=CARTESIAN_POINT('Ctrl Pts',(5.99998852113744,-9.81161263519312,1.49915292956805));
#46303=CARTESIAN_POINT('Ctrl Pts',(5.99996411956146,-9.80427237022355,1.50988876190026));
#46304=CARTESIAN_POINT('Ctrl Pts',(5.99995391373301,-9.79740660411635,1.52027358190028));
#46305=CARTESIAN_POINT('Ctrl Pts',(5.99995171009857,-9.79592415331001,1.52251586404948));
#46306=CARTESIAN_POINT('Ctrl Pts',(5.99995023593322,-9.79446368393491,1.52474166500346));
#46307=CARTESIAN_POINT('Ctrl Pts',(5.9999497685552,-9.79302597069511,1.52694837772846));
#46308=CARTESIAN_POINT('Ctrl Pts',(5.99994527145316,-9.77919232251255,1.54818132365431));
#46309=CARTESIAN_POINT('Ctrl Pts',(5.99996424179167,-9.76607610181729,1.56992337199025));
#46310=CARTESIAN_POINT('Ctrl Pts',(5.99998963853606,-9.75381433254361,1.59208686252081));
#46311=CARTESIAN_POINT('Ctrl Pts',(6.0000149372747,-9.74159988130341,1.61416482438388));
#46312=CARTESIAN_POINT('Ctrl Pts',(6.00004588401721,-9.73023410458729,1.63666047488403));
#46313=CARTESIAN_POINT('Ctrl Pts',(6.0000667455618,-9.71982413701758,1.65944401473347));
#46314=CARTESIAN_POINT('Ctrl Pts',(6.00008321614764,-9.71160526982082,1.67743205235613));
#46315=CARTESIAN_POINT('Ctrl Pts',(6.00009334879337,-9.70398170771886,1.69559852861912));
#46316=CARTESIAN_POINT('Ctrl Pts',(6.00009392184178,-9.696989358003,1.71386448439385));
#46317=CARTESIAN_POINT('Ctrl Pts',(6.00009465088789,-9.68809352076062,1.7371028772448));
#46318=CARTESIAN_POINT('Ctrl Pts',(6.00007926180274,-9.68022089597653,1.76050251695918));
#46319=CARTESIAN_POINT('Ctrl Pts',(6.00005735438713,-9.67340477113262,1.78388361762506));
#46320=CARTESIAN_POINT('Ctrl Pts',(6.00003516239185,-9.66650010409649,1.80756844129435));
#46321=CARTESIAN_POINT('Ctrl Pts',(6.00000603608545,-9.66067964436474,1.83123317213234));
#46322=CARTESIAN_POINT('Ctrl Pts',(5.99999995656782,-9.65592999578,1.85467974452393));
#46323=CARTESIAN_POINT('Ctrl Pts',(5.99999928313501,-9.65540387358089,1.85727693924436));
#46324=CARTESIAN_POINT('Ctrl Pts',(5.99999891415755,-9.65489084251379,1.85987145558861));
#46325=CARTESIAN_POINT('Ctrl Pts',(5.99999890661755,-9.6543908489942,1.86246302484216));
#46326=CARTESIAN_POINT('',(5.72001518115902,-9.72697656272786,2.0594344008613));
#46327=CARTESIAN_POINT('Ctrl Pts',(5.72001578478243,-9.72697810542107,2.05943472749027));
#46328=CARTESIAN_POINT('Ctrl Pts',(5.74831100472407,-9.71874550010011,2.04602639308294));
#46329=CARTESIAN_POINT('Ctrl Pts',(5.77568625593793,-9.71101591981585,2.03140417355019));
#46330=CARTESIAN_POINT('Ctrl Pts',(5.80217318781282,-9.70375779008786,2.01566912583796));
#46331=CARTESIAN_POINT('Ctrl Pts',(5.82514840580841,-9.69746196414892,2.00202027616873));
#46332=CARTESIAN_POINT('Ctrl Pts',(5.84745545926059,-9.6915209690025,1.9875330189415));
#46333=CARTESIAN_POINT('Ctrl Pts',(5.86910927423317,-9.68592085153798,1.97224290234583));
#46334=CARTESIAN_POINT('Ctrl Pts',(5.87213457678101,-9.68513844669823,1.97010668622169));
#46335=CARTESIAN_POINT('Ctrl Pts',(5.8751470713802,-9.68436271319161,1.9679548108044));
#46336=CARTESIAN_POINT('Ctrl Pts',(5.87814679973064,-9.6835936198623,1.96578732373684));
#46337=CARTESIAN_POINT('Ctrl Pts',(5.90308793908996,-9.6771990195299,1.94776582622233));
#46338=CARTESIAN_POINT('Ctrl Pts',(5.92714861735105,-9.67126222158962,1.92866869327927));
#46339=CARTESIAN_POINT('Ctrl Pts',(5.9503530048751,-9.6657663374122,1.90851108261494));
#46340=CARTESIAN_POINT('Ctrl Pts',(5.96736235160321,-9.66173772862197,1.8937350930033));
#46341=CARTESIAN_POINT('Ctrl Pts',(5.9839111813902,-9.65794632524712,1.87838828078923));
#46342=CARTESIAN_POINT('Ctrl Pts',(5.99999890661755,-9.65439084899398,1.86246302484326));
#46343=CARTESIAN_POINT('',(5.73278448927459,-10.3449549114295,1.71289216038973));
#46344=CARTESIAN_POINT('Origin',(5.89877390157852,-10.1838134841955,2.15616635811418));
#46345=CARTESIAN_POINT('Ctrl Pts',(5.73278343850714,-10.3449559315799,1.71288935424927));
#46346=CARTESIAN_POINT('Ctrl Pts',(5.74706594025812,-10.3340579318584,1.70357912933021));
#46347=CARTESIAN_POINT('Ctrl Pts',(5.7606924637996,-10.3236084956166,1.69367908770345));
#46348=CARTESIAN_POINT('Ctrl Pts',(5.7736157350861,-10.3135974006678,1.68336145275714));
#46349=CARTESIAN_POINT('Ctrl Pts',(5.78686204651708,-10.3033360606001,1.6727859101797));
#46350=CARTESIAN_POINT('Ctrl Pts',(5.79937022147026,-10.2935348620722,1.66177263797491));
#46351=CARTESIAN_POINT('Ctrl Pts',(5.81114106549577,-10.2841865752441,1.65048704321575));
#46352=CARTESIAN_POINT('Ctrl Pts',(5.82340063156014,-10.2744501502512,1.63873287382688));
#46353=CARTESIAN_POINT('Ctrl Pts',(5.83486131813222,-10.2652047124572,1.62668404740507));
#46354=CARTESIAN_POINT('Ctrl Pts',(5.84556649895441,-10.2564517360702,1.61449197344315));
#46355=CARTESIAN_POINT('Ctrl Pts',(5.84821827311156,-10.254283541346,1.61147188184532));
#46356=CARTESIAN_POINT('Ctrl Pts',(5.85082384535926,-10.2521456204111,1.60844280935656));
#46357=CARTESIAN_POINT('Ctrl Pts',(5.8533841464279,-10.2500381107383,1.60540667504513));
#46358=CARTESIAN_POINT('Ctrl Pts',(5.86462142145881,-10.2407881572411,1.59208094679144));
#46359=CARTESIAN_POINT('Ctrl Pts',(5.87496485395669,-10.2321098068509,1.57863342454987));
#46360=CARTESIAN_POINT('Ctrl Pts',(5.88446757402116,-10.2239747888587,1.5652369199639));
#46361=CARTESIAN_POINT('Ctrl Pts',(5.88870736401695,-10.2203452209387,1.55925985595098));
#46362=CARTESIAN_POINT('Ctrl Pts',(5.89278028921961,-10.2168239588668,1.55329243262826));
#46363=CARTESIAN_POINT('Ctrl Pts',(5.89669301056068,-10.2134092586863,1.54734745152633));
#46364=CARTESIAN_POINT('Ctrl Pts',(5.90303419873817,-10.2078751931276,1.53771266269452));
#46365=CARTESIAN_POINT('Ctrl Pts',(5.90895335839127,-10.2026197175057,1.52813789901526));
#46366=CARTESIAN_POINT('Ctrl Pts',(5.91447772628224,-10.1976310571052,1.51867479271051));
#46367=CARTESIAN_POINT('Ctrl Pts',(5.91723991022772,-10.195136726905,1.51394323955814));
#46368=CARTESIAN_POINT('Ctrl Pts',(5.91990336636591,-10.1927090997186,1.50923960424323));
#46369=CARTESIAN_POINT('Ctrl Pts',(5.92247184573428,-10.1903465860769,1.5045695429203));
#46370=CARTESIAN_POINT('Ctrl Pts',(5.92381837363261,-10.1891080359184,1.50212125856353));
#46371=CARTESIAN_POINT('Ctrl Pts',(5.92487882671067,-10.1881259571778,1.50016163694302));
#46372=CARTESIAN_POINT('Ctrl Pts',(5.9260665578843,-10.1870235681627,1.49794011890751));
#46373=CARTESIAN_POINT('Ctrl Pts',(5.92714440399162,-10.186023168632,1.49592412857225));
#46374=CARTESIAN_POINT('Ctrl Pts',(5.92832754104918,-10.1849235979202,1.49369260689465));
#46375=CARTESIAN_POINT('Ctrl Pts',(5.92989598840333,-10.1834528208751,1.49066569306805));
#46376=CARTESIAN_POINT('Ctrl Pts',(5.93909904534128,-10.1748228564377,1.47290490548488));
#46377=CARTESIAN_POINT('Ctrl Pts',(5.94727709077157,-10.1668954013321,1.45510029582112));
#46378=CARTESIAN_POINT('Ctrl Pts',(5.95446910596299,-10.159602320606,1.43744398035853));
#46379=CARTESIAN_POINT('Ctrl Pts',(5.96185599887856,-10.1521116236435,1.41930924230051));
#46380=CARTESIAN_POINT('Ctrl Pts',(5.96820359292578,-10.1452898169574,1.40133156463171));
#46381=CARTESIAN_POINT('Ctrl Pts',(5.97359534977732,-10.1390731519335,1.38368381110519));
#46382=CARTESIAN_POINT('Ctrl Pts',(5.97925150630115,-10.1325516355892,1.36517065129693));
#46383=CARTESIAN_POINT('Ctrl Pts',(5.98385679554753,-10.1266957972089,1.34702100805308));
#46384=CARTESIAN_POINT('Ctrl Pts',(5.98753741331365,-10.1214478149248,1.32938740197709));
#46385=CARTESIAN_POINT('Ctrl Pts',(5.99132844747022,-10.1160423962271,1.31122479798355));
#46386=CARTESIAN_POINT('Ctrl Pts',(5.99413962519572,-10.1112817793758,1.29360957474132));
#46387=CARTESIAN_POINT('Ctrl Pts',(5.9961226619511,-10.1071217563007,1.27665700852777));
#46388=CARTESIAN_POINT('Ctrl Pts',(5.99820305528237,-10.10275749818,1.25887216132167));
#46389=CARTESIAN_POINT('Ctrl Pts',(5.99937303010722,-10.0990542664404,1.24181635888134));
#46390=CARTESIAN_POINT('Ctrl Pts',(5.99980556935907,-10.0959821632958,1.22556956840182));
#46391=CARTESIAN_POINT('Ctrl Pts',(5.99993672661163,-10.0950506209991,1.2206431151534));
#46392=CARTESIAN_POINT('Ctrl Pts',(6.00000000770566,-10.094177247548,1.2157907116249));
#46393=CARTESIAN_POINT('Ctrl Pts',(5.99999999999901,-10.0933615553116,1.21101376485454));
#46394=CARTESIAN_POINT('Ctrl Pts',(5.99968359779795,-10.0074384078293,1.15797266224462));
#46395=CARTESIAN_POINT('Ctrl Pts',(5.99968359779795,-10.4048995152158,1.32597657845856));
#46396=CARTESIAN_POINT('Ctrl Pts',(5.99968359779795,-11.3019001480193,1.63774436815911));
#46397=CARTESIAN_POINT('Ctrl Pts',(5.99968359779795,-12.7412947791966,1.91665429258608));
#46398=CARTESIAN_POINT('Ctrl Pts',(5.99968359779795,-14.29016833524,1.9708926670458));
#46399=CARTESIAN_POINT('Ctrl Pts',(5.99968359779795,-15.8279016039224,1.7842043053716));
#46400=CARTESIAN_POINT('Ctrl Pts',(5.99968359779795,-17.3191350716031,1.36096628041763));
#46401=CARTESIAN_POINT('Ctrl Pts',(5.99968359779795,-18.6017699378808,0.768028796234896));
#46402=CARTESIAN_POINT('Ctrl Pts',(5.99968359779795,-19.3570916146985,0.286012646059891));
#46403=CARTESIAN_POINT('Ctrl Pts',(5.99968359779795,-19.663819703818,0.0645701956650116));
#46404=CARTESIAN_POINT('Ctrl Pts',(6.00710253473281,-9.93485458739443,1.32967571533749));
#46405=CARTESIAN_POINT('Ctrl Pts',(6.00710253473281,-10.3398263101573,1.50085626859094));
#46406=CARTESIAN_POINT('Ctrl Pts',(6.00710253473281,-11.2536100219151,1.81845838195038));
#46407=CARTESIAN_POINT('Ctrl Pts',(6.00710253473281,-12.7202225074092,2.10263700633451));
#46408=CARTESIAN_POINT('Ctrl Pts',(6.00710253473281,-14.2981186671284,2.1578944512487));
#46409=CARTESIAN_POINT('Ctrl Pts',(6.00710253473281,-15.8649160622648,1.96767950897587));
#46410=CARTESIAN_POINT('Ctrl Pts',(6.00710253473281,-17.3841034287348,1.53650155762526));
#46411=CARTESIAN_POINT('Ctrl Pts',(6.00710253473281,-18.6909640914977,0.932370814900383));
#46412=CARTESIAN_POINT('Ctrl Pts',(6.00710253473281,-19.460427013042,0.441331865624406));
#46413=CARTESIAN_POINT('Ctrl Pts',(6.00710253473281,-19.7729404670082,0.215710140185089));
#46414=CARTESIAN_POINT('Ctrl Pts',(5.90028450533773,-9.87522756015876,1.47072839845487));
#46415=CARTESIAN_POINT('Ctrl Pts',(5.90028450533773,-10.2863691933082,1.64451853359839));
#46416=CARTESIAN_POINT('Ctrl Pts',(5.90028450533773,-11.2139400700279,1.96691349712163));
#46417=CARTESIAN_POINT('Ctrl Pts',(5.90028450533773,-12.7029118048803,2.25542031632971));
#46418=CARTESIAN_POINT('Ctrl Pts',(5.90028450533773,-14.304649801108,2.3115149194609));
#46419=CARTESIAN_POINT('Ctrl Pts',(5.90028450533773,-15.8953231433789,2.11840291946901));
#46420=CARTESIAN_POINT('Ctrl Pts',(5.90028450533773,-17.4374744138533,1.68070238216881));
#46421=CARTESIAN_POINT('Ctrl Pts',(5.90028450533773,-18.7642363744345,1.0673764671802));
#46422=CARTESIAN_POINT('Ctrl Pts',(5.90028450533773,-19.5453162152736,0.568925360697917));
#46423=CARTESIAN_POINT('Ctrl Pts',(5.90028450533773,-19.8625823001286,0.339870394288303));
#46424=CARTESIAN_POINT('Ctrl Pts',(5.72238425036396,-9.85296650859829,1.52338876401701));
#46425=CARTESIAN_POINT('Ctrl Pts',(5.72238425036396,-10.2664116054559,1.69815315596464));
#46426=CARTESIAN_POINT('Ctrl Pts',(5.72238425036396,-11.1991297585749,2.02233747390619));
#46427=CARTESIAN_POINT('Ctrl Pts',(5.72238425036396,-12.6964490570393,2.31246017390902));
#46428=CARTESIAN_POINT('Ctrl Pts',(5.72238425036396,-14.307088123404,2.36886732024849));
#46429=CARTESIAN_POINT('Ctrl Pts',(5.72238425036396,-15.906675270626,2.17467373771829));
#46430=CARTESIAN_POINT('Ctrl Pts',(5.72238425036396,-17.4573998454323,1.73453806943007));
#46431=CARTESIAN_POINT('Ctrl Pts',(5.72238425036396,-18.7915917222315,1.11777924467817));
#46432=CARTESIAN_POINT('Ctrl Pts',(5.72238425036396,-19.5770086037039,0.616560896193298));
#46433=CARTESIAN_POINT('Ctrl Pts',(5.72238425036396,-19.8960490275765,0.38622416951656));
#46434=CARTESIAN_POINT('Ctrl Pts',(5.73278343850724,-10.3449559316229,1.71288935426486));
#46435=CARTESIAN_POINT('Ctrl Pts',(5.73338951373976,-10.6015227247303,1.80593970663245));
#46436=CARTESIAN_POINT('Ctrl Pts',(5.73395354980591,-10.8620213512442,1.88890386447321));
#46437=CARTESIAN_POINT('Ctrl Pts',(5.7344755567973,-11.125573150665,1.96144081361503));
#46438=CARTESIAN_POINT('Ctrl Pts',(5.73532468768319,-11.5542838319682,2.07943418324701));
#46439=CARTESIAN_POINT('Ctrl Pts',(5.73606260779809,-11.9910756848763,2.16983732042539));
#46440=CARTESIAN_POINT('Ctrl Pts',(5.73668937956405,-12.4324023067721,2.23164721150446));
#46441=CARTESIAN_POINT('Ctrl Pts',(5.73681687420498,-12.5221746645008,2.24422025690401));
#46442=CARTESIAN_POINT('Ctrl Pts',(5.73693976982774,-12.6121344962671,2.25561012995919));
#46443=CARTESIAN_POINT('Ctrl Pts',(5.73705806698001,-12.7022516999475,2.26580830619289));
#46444=CARTESIAN_POINT('Ctrl Pts',(5.73707478318901,-12.7149858865471,2.26724937930471));
#46445=CARTESIAN_POINT('Ctrl Pts',(5.73709140757734,-12.7277232153531,2.26866665698201));
#46446=CARTESIAN_POINT('Ctrl Pts',(5.73710794014652,-12.7404635980934,2.27006013275583));
#46447=CARTESIAN_POINT('Ctrl Pts',(5.73767502819834,-13.177474854341,2.31785811582091));
#46448=CARTESIAN_POINT('Ctrl Pts',(5.73813408904666,-13.6180836599348,2.33765181685216));
#46449=CARTESIAN_POINT('Ctrl Pts',(5.73848518400464,-14.0587011175929,2.3291771912748));
#46450=CARTESIAN_POINT('Ctrl Pts',(5.73855071735787,-14.140944222582,2.32759536670342));
#46451=CARTESIAN_POINT('Ctrl Pts',(5.73861248915111,-14.223187483881,2.32502866307856));
#46452=CARTESIAN_POINT('Ctrl Pts',(5.73867049970327,-14.3054073624453,2.32147534064942));
#46453=CARTESIAN_POINT('Ctrl Pts',(5.73897977956717,-14.7437578332544,2.30253101006965));
#46454=CARTESIAN_POINT('Ctrl Pts',(5.73918215133214,-15.1814478225317,2.25554262168904));
#46455=CARTESIAN_POINT('Ctrl Pts',(5.73927764637247,-15.6148698966946,2.18075633105717));
#46456=CARTESIAN_POINT('Ctrl Pts',(5.73929840890395,-15.709104523217,2.16449629589329));
#46457=CARTESIAN_POINT('Ctrl Pts',(5.73931411909929,-15.8031372038809,2.14692221903379));
#46458=CARTESIAN_POINT('Ctrl Pts',(5.73932477707789,-15.8969305343161,2.12803663990889));
#46459=CARTESIAN_POINT('Ctrl Pts',(5.73937358607066,-16.3264639532701,2.04154874857584));
#46460=CARTESIAN_POINT('Ctrl Pts',(5.73931644016915,-16.7509816658227,1.9275547088644));
#46461=CARTESIAN_POINT('Ctrl Pts',(5.73915333029904,-17.1669777326464,1.7867581306035));
#46462=CARTESIAN_POINT('Ctrl Pts',(5.73911747341489,-17.2584272737588,1.75580643778949));
#46463=CARTESIAN_POINT('Ctrl Pts',(5.73907649554377,-17.3494647971327,1.72355950598733));
#46464=CARTESIAN_POINT('Ctrl Pts',(5.739030396378,-17.4400527221644,1.69002486412558));
#46465=CARTESIAN_POINT('Ctrl Pts',(5.73900084492746,-17.4981232868037,1.66852778725571));
#46466=CARTESIAN_POINT('Ctrl Pts',(5.73896918896426,-17.5560090938688,1.646501547335));
#46467=CARTESIAN_POINT('Ctrl Pts',(5.73893542839204,-17.6137011364924,1.62395006942777));
#46468=CARTESIAN_POINT('Ctrl Pts',(5.73869640176937,-18.0221638252673,1.46428442260826));
#46469=CARTESIAN_POINT('Ctrl Pts',(5.73835187053754,-18.4209177953517,1.27828845729314));
#46470=CARTESIAN_POINT('Ctrl Pts',(5.73790179920334,-18.8067387748802,1.06736605898228));
#46471=CARTESIAN_POINT('Ctrl Pts',(5.73786596836643,-18.8374545471248,1.05057421848748));
#46472=CARTESIAN_POINT('Ctrl Pts',(5.73782946860637,-18.868088324797,1.03362440477691));
#46473=CARTESIAN_POINT('Ctrl Pts',(5.73779229989976,-18.898638467726,1.01651733151422));
#46474=CARTESIAN_POINT('Ctrl Pts',(5.73741169653613,-19.211468485665,0.841342830757322));
#46475=CARTESIAN_POINT('Ctrl Pts',(5.73696095091125,-19.5155308117973,0.649677901256858));
#46476=CARTESIAN_POINT('Ctrl Pts',(5.73644003521419,-19.8089444558075,0.442538425468125));
#46477=CARTESIAN_POINT('Ctrl Pts',(5.99999999999901,-10.0933615553116,1.21101376485454));
#46478=CARTESIAN_POINT('Ctrl Pts',(5.99999999999902,-10.2342115358103,1.26888262128331));
#46479=CARTESIAN_POINT('Ctrl Pts',(6.00000000007117,-10.3759192504903,1.32333077848203));
#46480=CARTESIAN_POINT('Ctrl Pts',(5.9999999982386,-10.5185579008191,1.37443737920613));
#46481=CARTESIAN_POINT('Ctrl Pts',(5.99999999639773,-10.6618425531298,1.42577543869178));
#46482=CARTESIAN_POINT('Ctrl Pts',(5.99999999249222,-10.8060670351755,1.47374173423722));
#46483=CARTESIAN_POINT('Ctrl Pts',(5.99999999189388,-10.9513242537834,1.51836744200924));
#46484=CARTESIAN_POINT('Ctrl Pts',(5.99999999151874,-11.042396086891,1.54634639582287));
#46485=CARTESIAN_POINT('Ctrl Pts',(5.9999999928441,-11.1338742268903,1.57301121591701));
#46486=CARTESIAN_POINT('Ctrl Pts',(5.99999999533728,-11.2257841171048,1.59835945117828));
#46487=CARTESIAN_POINT('Ctrl Pts',(5.99999999728275,-11.2975031128956,1.61813915033543));
#46488=CARTESIAN_POINT('Ctrl Pts',(5.99999999999971,-11.3694850404562,1.63711702887793));
#46489=CARTESIAN_POINT('Ctrl Pts',(5.99999999999971,-11.4417456110861,1.65529145736262));
#46490=CARTESIAN_POINT('Ctrl Pts',(5.99999999999971,-11.6167974858284,1.69931917193611));
#46491=CARTESIAN_POINT('Ctrl Pts',(5.99999998490599,-11.7934508492852,1.73870094298862));
#46492=CARTESIAN_POINT('Ctrl Pts',(5.99999998011058,-11.9712350857339,1.77327579437879));
#46493=CARTESIAN_POINT('Ctrl Pts',(5.9999999753187,-12.1488888962661,1.80782528099663));
#46494=CARTESIAN_POINT('Ctrl Pts',(5.99999998033521,-12.3276714858777,1.8375747837877));
#46495=CARTESIAN_POINT('Ctrl Pts',(5.99999998873906,-12.5070997365936,1.86241385083192));
#46496=CARTESIAN_POINT('Ctrl Pts',(5.99999999244222,-12.5861646634751,1.87335916747977));
#46497=CARTESIAN_POINT('Ctrl Pts',(5.9999999964315,-12.6653548222305,1.88335168086257));
#46498=CARTESIAN_POINT('Ctrl Pts',(5.99999999855252,-12.7446283783657,1.89238511809521));
#46499=CARTESIAN_POINT('Ctrl Pts',(5.99999999944807,-12.7780997308221,1.89619926970197));
#46500=CARTESIAN_POINT('Ctrl Pts',(5.99999999999971,-12.8115859483216,1.89984246629865));
#46501=CARTESIAN_POINT('Ctrl Pts',(5.99999999999971,-12.8450837113497,1.90331467554893));
#46502=CARTESIAN_POINT('Ctrl Pts',(5.99999999999971,-13.0549406604288,1.92506738898285));
#46503=CARTESIAN_POINT('Ctrl Pts',(5.99999998498977,-13.2652658520439,1.94004065756617));
#46504=CARTESIAN_POINT('Ctrl Pts',(5.99999998424828,-13.4758154446101,1.94828024097899));
#46505=CARTESIAN_POINT('Ctrl Pts',(5.9999999835058,-13.686645927915,1.95653081668414));
#46506=CARTESIAN_POINT('Ctrl Pts',(5.99999999341929,-13.8977019825745,1.95802978030323));
#46507=CARTESIAN_POINT('Ctrl Pts',(5.99999999806903,-14.108744973676,1.95277140513812));
#46508=CARTESIAN_POINT('Ctrl Pts',(5.99999999924309,-14.162033264823,1.9514436670062));
#46509=CARTESIAN_POINT('Ctrl Pts',(5.99999999999972,-14.2153207296733,1.94968484831666));
#46510=CARTESIAN_POINT('Ctrl Pts',(5.99999999999972,-14.2686035217176,1.94749433026555));
#46511=CARTESIAN_POINT('Ctrl Pts',(5.99999999999972,-14.2755281186275,1.94720965196801));
#46512=CARTESIAN_POINT('Ctrl Pts',(5.99999999998697,-14.2824526370692,1.94691772879533));
#46513=CARTESIAN_POINT('Ctrl Pts',(5.99999999996268,-14.2893770551291,1.94661855921418));
#46514=CARTESIAN_POINT('Ctrl Pts',(5.99999999919951,-14.5068769322331,1.93722147391849));
#46515=CARTESIAN_POINT('Ctrl Pts',(5.99999999014405,-14.7242778297529,1.92067056310208));
#46516=CARTESIAN_POINT('Ctrl Pts',(5.99999998974401,-14.9409228014816,1.89701138721353));
#46517=CARTESIAN_POINT('Ctrl Pts',(5.99999998934372,-15.1577057951409,1.87333713834586));
#46518=CARTESIAN_POINT('Ctrl Pts',(5.99999999677977,-15.3737313428998,1.84254561761958));
#46519=CARTESIAN_POINT('Ctrl Pts',(5.99999999936865,-15.5883455253423,1.80473432426097));
#46520=CARTESIAN_POINT('Ctrl Pts',(5.99999999976083,-15.6208564573964,1.79900646240549));
#46521=CARTESIAN_POINT('Ctrl Pts',(5.99999999999972,-15.6533350188477,1.79311760774684));
#46522=CARTESIAN_POINT('Ctrl Pts',(5.99999999999972,-15.6857789575284,1.78706820160289));
#46523=CARTESIAN_POINT('Ctrl Pts',(5.99999999999972,-15.7315477507526,1.77853428031619));
#46524=CARTESIAN_POINT('Ctrl Pts',(5.99999999951876,-15.777247151839,1.76967947395661));
#46525=CARTESIAN_POINT('Ctrl Pts',(5.99999999869846,-15.8228747191234,1.76050412644273));
#46526=CARTESIAN_POINT('Ctrl Pts',(5.99999999491949,-16.0330725133978,1.7182349912707));
#46527=CARTESIAN_POINT('Ctrl Pts',(5.99999998426348,-16.2417469407301,1.66916709667107));
#46528=CARTESIAN_POINT('Ctrl Pts',(5.9999999840381,-16.4486448314297,1.61336408257583));
#46529=CARTESIAN_POINT('Ctrl Pts',(5.99999998381272,-16.6555427221293,1.5575610684806));
#46530=CARTESIAN_POINT('Ctrl Pts',(5.99999999999972,-16.8606646284446,1.49502273906511));
#46531=CARTESIAN_POINT('Ctrl Pts',(5.99999999999972,-17.0637382052462,1.42576403766304));
#46532=CARTESIAN_POINT('Ctrl Pts',(5.99999999999972,-17.1461081213509,1.39767159198959));
#46533=CARTESIAN_POINT('Ctrl Pts',(5.9999999959448,-17.228147456194,1.36848536385057));
#46534=CARTESIAN_POINT('Ctrl Pts',(5.99999999152483,-17.3098017704308,1.33821950546152));
#46535=CARTESIAN_POINT('Ctrl Pts',(5.99999998224927,-17.4811578307823,1.27470494036867));
#46536=CARTESIAN_POINT('Ctrl Pts',(5.99999997346263,-17.6508169321434,1.20643267167925));
#46537=CARTESIAN_POINT('Ctrl Pts',(5.99999997653249,-17.8183278080572,1.13361882186231));
#46538=CARTESIAN_POINT('Ctrl Pts',(5.99999997960618,-17.9860479662972,1.06071400092609));
#46539=CARTESIAN_POINT('Ctrl Pts',(5.99999999486857,-18.15161412349,0.983256456991716));
#46540=CARTESIAN_POINT('Ctrl Pts',(5.99999999914226,-18.3145968762394,0.901509651121568));
#46541=CARTESIAN_POINT('Ctrl Pts',(5.9999999996837,-18.335245252142,0.89115310266497));
#46542=CARTESIAN_POINT('Ctrl Pts',(5.99999999999972,-18.3558521987823,0.880727768035456));
#46543=CARTESIAN_POINT('Ctrl Pts',(5.99999999999972,-18.376416875006,0.870234233398874));
#46544=CARTESIAN_POINT('Ctrl Pts',(5.99999999999972,-18.4906080449267,0.811965920116257));
#46545=CARTESIAN_POINT('Ctrl Pts',(5.99999999304432,-18.6034685434981,0.751564739808506));
#46546=CARTESIAN_POINT('Ctrl Pts',(5.99999999143185,-18.7150743302283,0.689018754849032));
#46547=CARTESIAN_POINT('Ctrl Pts',(5.999999989508,-18.8482324949303,0.614394411338742));
#46548=CARTESIAN_POINT('Ctrl Pts',(5.99999999273616,-18.9796053836656,0.536717940997866));
#46549=CARTESIAN_POINT('Ctrl Pts',(5.99999999547183,-19.1092808530767,0.455953080560843));
#46550=CARTESIAN_POINT('Ctrl Pts',(5.99999999819522,-19.238374241603,0.375550753466731));
#46551=CARTESIAN_POINT('Ctrl Pts',(5.99999999961476,-19.3657858118951,0.292087468462894));
#46552=CARTESIAN_POINT('Ctrl Pts',(5.99999999985073,-19.4915752850365,0.205483546894013));
#46553=CARTESIAN_POINT('Ctrl Pts',(5.99999999991369,-19.5251424039942,0.182373154069339));
#46554=CARTESIAN_POINT('Ctrl Pts',(5.99999999993326,-19.5585938461359,0.15903888480154));
#46555=CARTESIAN_POINT('Ctrl Pts',(5.99999999993295,-19.591930363142,0.135478724431447));
#46556=CARTESIAN_POINT('Ctrl Pts',(-5.8435303439,-10.0864263463971,1.57297215988872));
#46557=CARTESIAN_POINT('Ctrl Pts',(-3.895686895933,-10.6220924815581,2.52887995839878));
#46558=CARTESIAN_POINT('Ctrl Pts',(0.0001666015754012,-11.1575607682146,
3.48561785406667));
#46559=CARTESIAN_POINT('Ctrl Pts',(3.896020099084,-10.6220466822612,2.5287981273656));
#46560=CARTESIAN_POINT('Ctrl Pts',(5.844030148626,-10.0862888918595,1.57272686930798));
#46561=CARTESIAN_POINT('Ctrl Pts',(-5.8435303439,-10.8186462754844,1.86224935014598));
#46562=CARTESIAN_POINT('Ctrl Pts',(-3.895686895933,-11.3231586997723,2.74792625098423));
#46563=CARTESIAN_POINT('Ctrl Pts',(0.0001666015754012,-11.8270683815162,
3.63586015557252));
#46564=CARTESIAN_POINT('Ctrl Pts',(3.896020099084,-11.3231155997237,2.74785030484635));
#46565=CARTESIAN_POINT('Ctrl Pts',(5.844030148626,-10.8185168151363,1.86202208116965));
#46566=CARTESIAN_POINT('Ctrl Pts',(-5.8435303439,-12.4568735769095,2.30089098965536));
#46567=CARTESIAN_POINT('Ctrl Pts',(-3.895686895933,-12.8710977176598,3.06727942798209));
#46568=CARTESIAN_POINT('Ctrl Pts',(0.0001666015754012,-13.2856328777696,
3.8324424554894));
#46569=CARTESIAN_POINT('Ctrl Pts',(3.896020099084,-12.8710622619296,3.067213982596));
#46570=CARTESIAN_POINT('Ctrl Pts',(5.844030148626,-12.4567672849836,2.3006943306413));
#46571=CARTESIAN_POINT('Ctrl Pts',(-5.8435303439,-15.0614254536644,2.34071384846666));
#46572=CARTESIAN_POINT('Ctrl Pts',(-3.895686895933,-15.2991206270769,3.03320173188209));
#46573=CARTESIAN_POINT('Ctrl Pts',(0.0001666015754012,-15.5368879417648,
3.72636712889203));
#46574=CARTESIAN_POINT('Ctrl Pts',(3.896020099084,-15.2991002905297,3.03314244454918));
#46575=CARTESIAN_POINT('Ctrl Pts',(5.844030148626,-15.0613644599276,2.34053615271556));
#46576=CARTESIAN_POINT('Ctrl Pts',(-5.8435303439,-17.685813504417,1.67939836341819));
#46577=CARTESIAN_POINT('Ctrl Pts',(-3.895686895933,-17.7477953301944,2.42360808198115));
#46578=CARTESIAN_POINT('Ctrl Pts',(0.0001666015754012,-17.8092308921404,
3.16660406935368));
#46579=CARTESIAN_POINT('Ctrl Pts',(3.896020099084,-17.747790075531,2.42354453257711));
#46580=CARTESIAN_POINT('Ctrl Pts',(5.844030148626,-17.6857975995771,1.67920739556743));
#46581=CARTESIAN_POINT('Ctrl Pts',(-5.8435303439,-19.259293374411,0.803936086515145));
#46582=CARTESIAN_POINT('Ctrl Pts',(-3.895686895933,-19.2409363781689,1.65690460410087));
#46583=CARTESIAN_POINT('Ctrl Pts',(0.0001666015754012,-19.2238042759609,
2.51236030102749));
#46584=CARTESIAN_POINT('Ctrl Pts',(3.896020099084,-19.2409378435011,1.65683143587068));
#46585=CARTESIAN_POINT('Ctrl Pts',(5.844030148626,-19.2592980849162,0.803717210669497));
#46586=CARTESIAN_POINT('Ctrl Pts',(-5.8435303439,-19.9729830806857,0.275591947000292));
#46587=CARTESIAN_POINT('Ctrl Pts',(-3.895686895933,-19.9313477701919,1.19822030152823));
#46588=CARTESIAN_POINT('Ctrl Pts',(0.0001666015754012,-19.8897492247631,
2.12096520787675));
#46589=CARTESIAN_POINT('Ctrl Pts',(3.896020099084,-19.9313513281736,1.1981413779533));
#46590=CARTESIAN_POINT('Ctrl Pts',(5.844030148626,-19.9729937645153,0.275355196075999));
#46591=CARTESIAN_POINT('Ctrl Pts',(-5.73278975426698,-10.3449510844138,
1.7128961701427));
#46592=CARTESIAN_POINT('Ctrl Pts',(-5.37911661672383,-10.4448068797057,
1.88163075288831));
#46593=CARTESIAN_POINT('Ctrl Pts',(-5.01642977825625,-10.5335803034939,
2.03722749340925));
#46594=CARTESIAN_POINT('Ctrl Pts',(-4.64634172525782,-10.611675775621,2.17794544599532));
#46595=CARTESIAN_POINT('Ctrl Pts',(-4.3719281748242,-10.6695821457552,2.28228524477033));
#46596=CARTESIAN_POINT('Ctrl Pts',(-4.09344547188132,-10.7216176124039,
2.37844082849794));
#46597=CARTESIAN_POINT('Ctrl Pts',(-3.81155096772038,-10.7679708202799,
2.46571664042017));
#46598=CARTESIAN_POINT('Ctrl Pts',(-3.57259918982531,-10.8072627584682,
2.53969719030044));
#46599=CARTESIAN_POINT('Ctrl Pts',(-3.33119591680233,-10.8424716474326,
2.60729655139232));
#46600=CARTESIAN_POINT('Ctrl Pts',(-3.08774152507161,-10.8737346886791,
2.66812502300776));
#46601=CARTESIAN_POINT('Ctrl Pts',(-3.04398962084052,-10.8793530617011,
2.67905668641183));
#46602=CARTESIAN_POINT('Ctrl Pts',(-3.00017147216096,-10.88484406648,2.68976978813144));
#46603=CARTESIAN_POINT('Ctrl Pts',(-2.95628940287459,-10.8902085973293,
2.70026223126147));
#46604=CARTESIAN_POINT('Ctrl Pts',(-2.75785502552652,-10.9144669642695,
2.74770897780801));
#46605=CARTESIAN_POINT('Ctrl Pts',(-2.55810778692668,-10.9362004020262,
2.79065903858132));
#46606=CARTESIAN_POINT('Ctrl Pts',(-2.35731447366229,-10.955388545368,2.82889657577336));
#46607=CARTESIAN_POINT('Ctrl Pts',(-2.16336116913836,-10.9739230460858,
2.86583155420807));
#46608=CARTESIAN_POINT('Ctrl Pts',(-1.96843184497064,-10.9900826889669,
2.89836954757001));
#46609=CARTESIAN_POINT('Ctrl Pts',(-1.77276694175945,-11.0038727784303,
2.92635796653381));
#46610=CARTESIAN_POINT('Ctrl Pts',(-1.58019158343941,-11.0174451226581,
2.9539044489244));
#46611=CARTESIAN_POINT('Ctrl Pts',(-1.38690369223543,-11.0287220802415,
2.97704375250748));
#46612=CARTESIAN_POINT('Ctrl Pts',(-1.19313249798695,-11.0377328161332,
2.99567340172542));
#46613=CARTESIAN_POINT('Ctrl Pts',(-0.994964448639617,-11.0469480143043,
3.01472577563405));
#46614=CARTESIAN_POINT('Ctrl Pts',(-0.796290914181298,-11.0537927389847,
3.02906107575225));
#46615=CARTESIAN_POINT('Ctrl Pts',(-0.597357085544801,-11.0583261912699,
3.0386198665503));
#46616=CARTESIAN_POINT('Ctrl Pts',(-0.408582158378835,-11.0626281349404,
3.04769052109439));
#46617=CARTESIAN_POINT('Ctrl Pts',(-0.219572842985093,-11.0648489562389,
3.05246026215182));
#46618=CARTESIAN_POINT('Ctrl Pts',(-0.0305386525764808,-11.0650644686467,
3.05292360453938));
#46619=CARTESIAN_POINT('Ctrl Pts',(-0.0203657988837101,-11.0650760664227,
3.05294853925784));
#46620=CARTESIAN_POINT('Ctrl Pts',(-0.0101928731518484,-11.0650818628657,
3.05296101346823));
#46621=CARTESIAN_POINT('Ctrl Pts',(-1.99080335683277E-5,-11.0650818718951,
3.05296103009418));
#46622=CARTESIAN_POINT('Ctrl Pts',(-1.32720223513428E-5,-11.065081871901,
3.05296103010502));
#46623=CARTESIAN_POINT('Ctrl Pts',(-6.63601115180548E-6,-11.0650818719044,
3.05296103011057));
#46624=CARTESIAN_POINT('Ctrl Pts',(3.19744231092045E-14,-11.0650818719054,
3.05296103011081));
#46625=CARTESIAN_POINT('Ctrl Pts',(0.189388142373251,-11.0650818994384,
3.05296103706175));
#46626=CARTESIAN_POINT('Ctrl Pts',(0.378762758287906,-11.0630739549068,
3.04863958591605));
#46627=CARTESIAN_POINT('Ctrl Pts',(0.567913157339342,-11.0589804436018,
3.03999975310335));
#46628=CARTESIAN_POINT('Ctrl Pts',(0.769315340839379,-11.0546217844652,
3.03080029488239));
#46629=CARTESIAN_POINT('Ctrl Pts',(0.970463320504467,-11.0478984432597,
3.01670457339992));
#46630=CARTESIAN_POINT('Ctrl Pts',(1.17110275584932,-11.0387476846565,2.99777185791181));
#46631=CARTESIAN_POINT('Ctrl Pts',(1.36689625026887,-11.0298179396119,2.97929641454797));
#46632=CARTESIAN_POINT('Ctrl Pts',(1.56220546893065,-11.018576867138,2.95621526529146));
#46633=CARTESIAN_POINT('Ctrl Pts',(1.75679405869412,-11.0049935453993,2.92863254316764));
#46634=CARTESIAN_POINT('Ctrl Pts',(1.95860682728074,-10.9909059374361,2.90002580150961));
#46635=CARTESIAN_POINT('Ctrl Pts',(2.15964446646054,-10.9742989289985,2.8665770390857));
#46636=CARTESIAN_POINT('Ctrl Pts',(2.3596433095925,-10.9551663818215,2.82845300631155));
#46637=CARTESIAN_POINT('Ctrl Pts',(2.55964215272445,-10.9360338346445,2.7903289735374));
#46638=CARTESIAN_POINT('Ctrl Pts',(2.75860219980856,-10.9143759250434,2.74753000555756));
#46639=CARTESIAN_POINT('Ctrl Pts',(2.95625978420382,-10.8902128218895,2.70026948337304));
#46640=CARTESIAN_POINT('Ctrl Pts',(3.19866256794929,-10.8605797395752,2.64231024961106));
#46641=CARTESIAN_POINT('Ctrl Pts',(3.43911507177877,-10.8270851551401,2.5776139620524));
#46642=CARTESIAN_POINT('Ctrl Pts',(3.67722557626171,-10.7895899938813,2.50655383829733));
#46643=CARTESIAN_POINT('Ctrl Pts',(3.96182040203707,-10.7447749660477,2.42162124120941));
#46644=CARTESIAN_POINT('Ctrl Pts',(4.2430695535221,-10.6942449885152,2.32759836386369));
#46645=CARTESIAN_POINT('Ctrl Pts',(4.52030419347271,-10.6378030703474,2.22518608067058));
#46646=CARTESIAN_POINT('Ctrl Pts',(4.88748869107178,-10.5630483522153,2.08954573371057));
#46647=CARTESIAN_POINT('Ctrl Pts',(5.24763102041744,-10.4779235063923,1.93919512435998));
#46648=CARTESIAN_POINT('Ctrl Pts',(5.59917725319807,-10.3820335990965,1.77581546490113));
#46649=CARTESIAN_POINT('Ctrl Pts',(5.64385361771994,-10.3698473998065,1.75505230904618));
#46650=CARTESIAN_POINT('Ctrl Pts',(5.68839114945533,-10.3574873916263,1.73407867881818));
#46651=CARTESIAN_POINT('Ctrl Pts',(5.73278665894458,-10.3449528049755,1.71289795467394));
#46652=CARTESIAN_POINT('Ctrl Pts',(-5.84445822842855,-10.3331482537831,
1.66691354819033));
#46653=CARTESIAN_POINT('Ctrl Pts',(-5.38771312971971,-10.4717359418486,
1.89165575395626));
#46654=CARTESIAN_POINT('Ctrl Pts',(-4.3554965874562,-10.7317200894033,2.33408242690297));
#46655=CARTESIAN_POINT('Ctrl Pts',(-2.68987671632907,-10.9928689957095,
2.82006056998998));
#46656=CARTESIAN_POINT('Ctrl Pts',(-0.896046561860736,-11.1236914322874,
3.0802434618201));
#46657=CARTESIAN_POINT('Ctrl Pts',(0.899212367975122,-11.1235788104192,
3.08001404244163));
#46658=CARTESIAN_POINT('Ctrl Pts',(2.69302899897811,-10.9925148949045,2.81937246391085));
#46659=CARTESIAN_POINT('Ctrl Pts',(4.35754598382318,-10.7312667792372,2.33328151229503));
#46660=CARTESIAN_POINT('Ctrl Pts',(5.38875361144458,-10.4714240747359,1.8911487048757));
#46661=CARTESIAN_POINT('Ctrl Pts',(5.84456702674697,-10.3331152084568,1.66686006128739));
#46662=CARTESIAN_POINT('Ctrl Pts',(-5.72526670899364,-10.051662855528,1.59453804482822));
#46663=CARTESIAN_POINT('Ctrl Pts',(-5.27774229481278,-10.1879516186282,
1.81303528671515));
#46664=CARTESIAN_POINT('Ctrl Pts',(-4.26639310686917,-10.4437163668707,
2.24334241603749));
#46665=CARTESIAN_POINT('Ctrl Pts',(-2.63466707886049,-10.7007617776932,
2.71620795356878));
#46666=CARTESIAN_POINT('Ctrl Pts',(-0.877615543970877,-10.8295728779202,
2.96940634106978));
#46667=CARTESIAN_POINT('Ctrl Pts',(0.880716270486781,-10.8294619741478,
2.96918307565484));
#46668=CARTESIAN_POINT('Ctrl Pts',(2.63775495090047,-10.7004131618419,2.71553833995515));
#46669=CARTESIAN_POINT('Ctrl Pts',(4.26840102530109,-10.4432703029748,2.24256325387882));
#46670=CARTESIAN_POINT('Ctrl Pts',(5.27876176978872,-10.1876449150383,1.81254230777516));
#46671=CARTESIAN_POINT('Ctrl Pts',(5.72537331154816,-10.0516303572414,1.59448604041269));
#46672=CARTESIAN_POINT('Ctrl Pts',(-5.71930850295601,-9.77801082274168,
1.74867595839893));
#46673=CARTESIAN_POINT('Ctrl Pts',(-5.27308497670522,-9.91296458113766,
1.96485547901025));
#46674=CARTESIAN_POINT('Ctrl Pts',(-4.26441701469436,-10.1663983984807,
2.39093719126511));
#46675=CARTESIAN_POINT('Ctrl Pts',(-2.63505179740053,-10.4215122664498,
2.86008785287843));
#46676=CARTESIAN_POINT('Ctrl Pts',(-0.878095819546688,-10.5495459780576,
3.1117583958528));
#46677=CARTESIAN_POINT('Ctrl Pts',(0.881197899559866,-10.5494356793196,
3.11153631405035));
#46678=CARTESIAN_POINT('Ctrl Pts',(2.63813754839394,-10.4211659428768,2.85942274077247));
#46679=CARTESIAN_POINT('Ctrl Pts',(4.26642002857102,-10.1659561458811,2.39016514377892));
#46680=CARTESIAN_POINT('Ctrl Pts',(5.27410150328015,-9.91266085860032,1.96436771771184));
#46681=CARTESIAN_POINT('Ctrl Pts',(5.71941478998875,-9.77797863935038,1.74862451318204));
#46682=CARTESIAN_POINT('Ctrl Pts',(-5.8304606616367,-9.69020667453587,2.02906075227467));
#46683=CARTESIAN_POINT('Ctrl Pts',(-5.37677190025951,-9.82565779738564,
2.24835754410253));
#46684=CARTESIAN_POINT('Ctrl Pts',(-4.35085467555363,-10.0801654743651,
2.68085673877077));
#46685=CARTESIAN_POINT('Ctrl Pts',(-2.69078117464156,-10.3367762696711,
3.15810692828297));
#46686=CARTESIAN_POINT('Ctrl Pts',(-0.89717515569234,-10.4657722550533,
3.41470022626425));
#46687=CARTESIAN_POINT('Ctrl Pts',(0.900344142508115,-10.4656610546937,
3.41447358771451));
#46688=CARTESIAN_POINT('Ctrl Pts',(2.69392847455747,-10.3364275545085,3.15742939829163));
#46689=CARTESIAN_POINT('Ctrl Pts',(4.35289254910898,-10.0797211187514,2.68007253983937));
#46690=CARTESIAN_POINT('Ctrl Pts',(5.3778054549422,-9.82535293419236,2.24786275370891));
#46691=CARTESIAN_POINT('Ctrl Pts',(5.83056871866019,-9.69017436905015,2.02900857919085));
#46692=CARTESIAN_POINT('Ctrl Pts',(-5.72001725923566,-9.72697394243655,
2.05943194359944));
#46693=CARTESIAN_POINT('Ctrl Pts',(-5.48693272988403,-9.79479243900217,
2.1698632189192));
#46694=CARTESIAN_POINT('Ctrl Pts',(-5.24893985465217,-9.8578898842069,2.27505821719543));
#46695=CARTESIAN_POINT('Ctrl Pts',(-5.00626021853139,-9.91632228116233,
2.37435968097908));
#46696=CARTESIAN_POINT('Ctrl Pts',(-4.81288427723629,-9.96288333566201,
2.45348669113162));
#46697=CARTESIAN_POINT('Ctrl Pts',(-4.61653254429665,-10.0064820069781,
2.5288708354457));
#46698=CARTESIAN_POINT('Ctrl Pts',(-4.41732289584036,-10.0471397417556,
2.60015753014603));
#46699=CARTESIAN_POINT('Ctrl Pts',(-4.40009339203155,-10.0506562009313,
2.60632306674215));
#46700=CARTESIAN_POINT('Ctrl Pts',(-4.38284251386637,-10.0541506570791,
2.6124579399829));
#46701=CARTESIAN_POINT('Ctrl Pts',(-4.36557037135436,-10.0576231265581,
2.61856191382665));
#46702=CARTESIAN_POINT('Ctrl Pts',(-4.13177327318589,-10.1046267502896,
2.70118579045179));
#46703=CARTESIAN_POINT('Ctrl Pts',(-3.89408346669447,-10.1475966538231,
2.77817366986499));
#46704=CARTESIAN_POINT('Ctrl Pts',(-3.65276146729705,-10.1865292264382,
2.84906061991673));
#46705=CARTESIAN_POINT('Ctrl Pts',(-3.53210046759834,-10.2059955127458,
2.8845040949426));
#46706=CARTESIAN_POINT('Ctrl Pts',(-3.41053208906834,-10.2244515842033,
2.9184231578225));
#46707=CARTESIAN_POINT('Ctrl Pts',(-3.28809316452347,-10.2418917665002,
2.95076478016178));
#46708=CARTESIAN_POINT('Ctrl Pts',(-3.22687370225103,-10.2506118576487,
2.96693559133142));
#46709=CARTESIAN_POINT('Ctrl Pts',(-3.16543659837793,-10.2590779517068,
2.98271203496152));
#46710=CARTESIAN_POINT('Ctrl Pts',(-3.10378680031152,-10.2672889927752,
2.99808788577522));
#46711=CARTESIAN_POINT('Ctrl Pts',(-3.07296190127832,-10.2713945133094,
3.00577581118207));
#46712=CARTESIAN_POINT('Ctrl Pts',(-3.04208382849723,-10.2754362692712,
3.01336358796922));
#46713=CARTESIAN_POINT('Ctrl Pts',(-3.01115321055681,-10.2794141145398,
3.02085044997317));
#46714=CARTESIAN_POINT('Ctrl Pts',(-2.98624862142243,-10.2826169798121,
3.02687869106661));
#46715=CARTESIAN_POINT('Ctrl Pts',(-2.96051439371824,-10.2858783416408,
3.03303033589897));
#46716=CARTESIAN_POINT('Ctrl Pts',(-2.93587242134819,-10.2889564309938,
3.03884835934926));
#46717=CARTESIAN_POINT('Ctrl Pts',(-2.929909936501,-10.2897012196353,3.04025611503302));
#46718=CARTESIAN_POINT('Ctrl Pts',(-2.92401146545564,-10.2904353978881,
3.04164453878627));
#46719=CARTESIAN_POINT('Ctrl Pts',(-2.91820435563567,-10.2911557637968,
3.04300753181412));
#46720=CARTESIAN_POINT('Ctrl Pts',(-2.83088075353848,-10.3019881654436,
3.06350334892712));
#46721=CARTESIAN_POINT('Ctrl Pts',(-2.74333417703633,-10.3123017606963,
3.08311072788639));
#46722=CARTESIAN_POINT('Ctrl Pts',(-2.65557894832266,-10.3221031860875,
3.10181531402008));
#46723=CARTESIAN_POINT('Ctrl Pts',(-2.39760263918788,-10.3509166890975,
3.15680166828517));
#46724=CARTESIAN_POINT('Ctrl Pts',(-2.13782516201486,-10.3753059013279,
3.20398885075858));
#46725=CARTESIAN_POINT('Ctrl Pts',(-1.8767291264866,-10.3953879991318,3.24316256673323));
#46726=CARTESIAN_POINT('Ctrl Pts',(-1.61583159188067,-10.4154548293161,
3.28230650049101));
#46727=CARTESIAN_POINT('Ctrl Pts',(-1.35361695580228,-10.431221027104,3.31344948606628));
#46728=CARTESIAN_POINT('Ctrl Pts',(-1.09054431580665,-10.4427785152057,
3.3363382803531));
#46729=CARTESIAN_POINT('Ctrl Pts',(-1.02152917496517,-10.445810535826,3.34234298445849));
#46730=CARTESIAN_POINT('Ctrl Pts',(-0.952454888250652,-10.4485527672398,
3.34777937920162));
#46731=CARTESIAN_POINT('Ctrl Pts',(-0.883329562900901,-10.4510065925464,
3.35264239616797));
#46732=CARTESIAN_POINT('Ctrl Pts',(-0.621402695948059,-10.4603045274398,
3.37106914195888));
#46733=CARTESIAN_POINT('Ctrl Pts',(-0.358743620959177,-10.465463405017,
3.38126706659519));
#46734=CARTESIAN_POINT('Ctrl Pts',(-0.0958570272718549,-10.4664724902806,
3.38326282124112));
#46735=CARTESIAN_POINT('Ctrl Pts',(-0.0639000864720908,-10.466595156399,
3.38350542856536));
#46736=CARTESIAN_POINT('Ctrl Pts',(-0.0319397761689494,-10.4666564718144,
3.38362677429207));
#46737=CARTESIAN_POINT('Ctrl Pts',(2.300178284668E-5,-10.4666563938114,
3.38362685957177));
#46738=CARTESIAN_POINT('Ctrl Pts',(0.260337415711732,-10.4666557585314,
3.38362755411516));
#46739=CARTESIAN_POINT('Ctrl Pts',(0.520480755586545,-10.4625880719849,
3.37557893746241));
#46740=CARTESIAN_POINT('Ctrl Pts',(0.77997268513999,-10.4544603514888,3.35948138375795));
#46741=CARTESIAN_POINT('Ctrl Pts',(0.81547805772961,-10.4533482639375,3.35727881182039));
#46742=CARTESIAN_POINT('Ctrl Pts',(0.850971231436825,-10.452160130752,3.3549254805135));
#46743=CARTESIAN_POINT('Ctrl Pts',(0.886450970381633,-10.4508959359216,
3.35242132307833));
#46744=CARTESIAN_POINT('Ctrl Pts',(1.08153280298439,-10.4439448857833,3.33865246129671));
#46745=CARTESIAN_POINT('Ctrl Pts',(1.27620873109396,-10.4346949219051,3.32032490351649));
#46746=CARTESIAN_POINT('Ctrl Pts',(1.47030049461408,-10.4231094685303,3.29755584435938));
#46747=CARTESIAN_POINT('Ctrl Pts',(1.71399050157766,-10.408563466359,3.268968375814));
#46748=CARTESIAN_POINT('Ctrl Pts',(1.95674662779223,-10.3903532933778,3.23333124378285));
#46749=CARTESIAN_POINT('Ctrl Pts',(2.19819766295024,-10.368396071073,3.19083022181142));
#46750=CARTESIAN_POINT('Ctrl Pts',(2.31892318052924,-10.3574174599205,3.1695797108257));
#46751=CARTESIAN_POINT('Ctrl Pts',(2.43932260395416,-10.345501247044,3.14661428567981));
#46752=CARTESIAN_POINT('Ctrl Pts',(2.55935059295051,-10.3326319233828,3.12196359574265));
#46753=CARTESIAN_POINT('Ctrl Pts',(2.59249782324256,-10.3290778987035,3.11515599942251));
#46754=CARTESIAN_POINT('Ctrl Pts',(2.62561677822834,-10.3254511436961,3.10821993941185));
#46755=CARTESIAN_POINT('Ctrl Pts',(2.65870640247661,-10.3217513385284,3.10115598276616));
#46756=CARTESIAN_POINT('Ctrl Pts',(2.68552647536097,-10.3187525421834,3.09543044684989));
#46757=CARTESIAN_POINT('Ctrl Pts',(2.71232727914222,-10.3157057549886,3.08962088827545));
#46758=CARTESIAN_POINT('Ctrl Pts',(2.73910840455801,-10.3126107653246,3.08372779963449));
#46759=CARTESIAN_POINT('Ctrl Pts',(2.76901975340948,-10.3091540280107,3.0771459167817));
#46760=CARTESIAN_POINT('Ctrl Pts',(2.79890649941338,-10.305637192199,3.07045976831403));
#46761=CARTESIAN_POINT('Ctrl Pts',(2.82876795903543,-10.3020600177251,3.06366991148607));
#46762=CARTESIAN_POINT('Ctrl Pts',(2.85294750930066,-10.2991634925353,3.05817199924254));
#46763=CARTESIAN_POINT('Ctrl Pts',(2.8763080945304,-10.2963257491386,3.05279238073469));
#46764=CARTESIAN_POINT('Ctrl Pts',(2.90079864213134,-10.2933080492701,3.0470793056848));
#46765=CARTESIAN_POINT('Ctrl Pts',(2.90655363219694,-10.2925989253645,3.04573680037655));
#46766=CARTESIAN_POINT('Ctrl Pts',(2.9123709587508,-10.2918797545079,3.04437569618811));
#46767=CARTESIAN_POINT('Ctrl Pts',(2.9182757973104,-10.2911472306701,3.04298978108805));
#46768=CARTESIAN_POINT('Ctrl Pts',(3.17624357856515,-10.2591450773108,2.98244258072667));
#46769=CARTESIAN_POINT('Ctrl Pts',(3.43059704783037,-10.2227651596086,2.91473261962076));
#46770=CARTESIAN_POINT('Ctrl Pts',(3.68103189504611,-10.1820138635033,2.84048532916211));
#46771=CARTESIAN_POINT('Ctrl Pts',(3.93146674226184,-10.141262567398,2.76623803870345));
#46772=CARTESIAN_POINT('Ctrl Pts',(4.17798321528555,-10.0961399671612,2.68545293148422));
#46773=CARTESIAN_POINT('Ctrl Pts',(4.42027976008899,-10.0466389069888,2.59870198645564));
#46774=CARTESIAN_POINT('Ctrl Pts',(4.67259159069087,-9.99509172905041,2.50836520610923));
#46775=CARTESIAN_POINT('Ctrl Pts',(4.92032803560847,-9.93879687513458,2.41155906436459));
#46776=CARTESIAN_POINT('Ctrl Pts',(5.16324371845964,-9.87774347039952,2.30887781548181));
#46777=CARTESIAN_POINT('Ctrl Pts',(5.35177735600155,-9.83035821991295,2.22918403395236));
#46778=CARTESIAN_POINT('Ctrl Pts',(5.53740701620603,-9.78010618807128,2.1459500771757));
#46779=CARTESIAN_POINT('Ctrl Pts',(5.72001441299688,-9.72697459952105,2.05943398518195));
#46780=CARTESIAN_POINT('Origin',(5.6,9.91330329119712,16.8993688492374));
#46781=CARTESIAN_POINT('',(5.99999999995608,9.91329603789449,16.8993703023573));
#46782=CARTESIAN_POINT('',(5.59336167795831,10.1144355810365,17.2450590896867));
#46783=CARTESIAN_POINT('Origin',(5.6,9.91330329119712,16.8993688492374));
#46784=CARTESIAN_POINT('',(5.736443493912,10.2877312271804,16.9337809062588));
#46785=CARTESIAN_POINT('Origin',(5.59997427807905,9.91328074797341,16.8993778521222));
#46786=CARTESIAN_POINT('Origin',(5.599999999773,9.91330329131382,16.8993688489353));
#46787=CARTESIAN_POINT('Ctrl Pts',(5.99999999997507,9.91330135657847,16.8993650110572));
#46788=CARTESIAN_POINT('Ctrl Pts',(5.99999999997507,9.83522888887418,16.9447895967211));
#46789=CARTESIAN_POINT('Ctrl Pts',(5.99999999997507,9.75700380943156,16.989952878335));
#46790=CARTESIAN_POINT('Ctrl Pts',(5.99999999997507,9.67862816205461,17.0348534691249));
#46791=CARTESIAN_POINT('Ctrl Pts',(6.00000263486327,10.032695805171,17.1045706743813));
#46792=CARTESIAN_POINT('Ctrl Pts',(6.00000263486327,9.95416474484471,17.1502620775629));
#46793=CARTESIAN_POINT('Ctrl Pts',(6.00000263486327,9.87548026973953,17.1956905916351));
#46794=CARTESIAN_POINT('Ctrl Pts',(6.00000263486327,9.79664425061367,17.240854924572));
#46795=CARTESIAN_POINT('Ctrl Pts',(5.83074066841791,10.1164175341797,17.2484649101538));
#46796=CARTESIAN_POINT('Ctrl Pts',(5.83074066841791,10.0375648997121,17.2943434110114));
#46797=CARTESIAN_POINT('Ctrl Pts',(5.83074066841791,9.95855828735685,17.339957911285));
#46798=CARTESIAN_POINT('Ctrl Pts',(5.83074066841791,9.87939944652955,17.3853071853885));
#46799=CARTESIAN_POINT('Ctrl Pts',(5.59336110044213,10.1144359114724,17.2450590549684));
#46800=CARTESIAN_POINT('Ctrl Pts',(5.59336110044213,10.0355908883956,17.2909331273823));
#46801=CARTESIAN_POINT('Ctrl Pts',(5.59336110044213,9.95659190076084,17.3365432255189));
#46802=CARTESIAN_POINT('Ctrl Pts',(5.59336110044213,9.8774407008502,17.3818881222188));
#46803=CARTESIAN_POINT('',(5.59336169566021,9.87744142947385,17.3818877157234));
#46804=CARTESIAN_POINT('Origin',(5.59336169595361,7.4927251628836,13.0987219083732));
#46805=CARTESIAN_POINT('',(6.,9.67863108609234,17.0348569101268));
#46806=CARTESIAN_POINT('Origin',(5.6,9.67863108611231,17.0348569102122));
#46807=CARTESIAN_POINT('Ctrl Pts',(5.99999999999163,9.91329301289976,16.8993720623907));
#46808=CARTESIAN_POINT('Ctrl Pts',(5.99999999999168,9.88722393978031,16.9145397247202));
#46809=CARTESIAN_POINT('Ctrl Pts',(5.9999999999997,9.86114407693772,16.9296767195884));
#46810=CARTESIAN_POINT('Ctrl Pts',(5.9999999999997,9.83508082014215,16.9447638792478));
#46811=CARTESIAN_POINT('Ctrl Pts',(5.9999999999997,9.80901756334656,16.9598510389072));
#46812=CARTESIAN_POINT('Ctrl Pts',(5.9999999999997,9.78297091259799,16.9748883633578));
#46813=CARTESIAN_POINT('Ctrl Pts',(5.9999999999997,9.75690044719229,16.9899010654912));
#46814=CARTESIAN_POINT('Ctrl Pts',(5.9999999999997,9.73082998178661,17.0049137676245));
#46815=CARTESIAN_POINT('Ctrl Pts',(5.9999999999997,9.7047357017238,17.0199018474406));
#46816=CARTESIAN_POINT('Ctrl Pts',(5.9999999999997,9.67863108609234,17.0348569101268));
#46817=CARTESIAN_POINT('Origin',(5.6,9.67863108603356,17.0348569100686));
#46818=CARTESIAN_POINT('',(5.73644276526939,9.52121697668264,17.3763304375098));
#46819=CARTESIAN_POINT('Origin',(5.6,9.67863108603356,17.0348569100686));
#46820=CARTESIAN_POINT('Origin',(5.600000004204,9.67863108709891,17.0348569087034));
#46821=CARTESIAN_POINT('Ctrl Pts',(5.99928507671022,9.77920217854224,17.0543525003981));
#46822=CARTESIAN_POINT('Ctrl Pts',(5.99928507671022,9.74894839966019,17.0407709830063));
#46823=CARTESIAN_POINT('Ctrl Pts',(5.99928507671022,9.27203920735655,16.8237867818179));
#46824=CARTESIAN_POINT('Ctrl Pts',(5.99928507671022,8.38193522943825,16.330354291202));
#46825=CARTESIAN_POINT('Ctrl Pts',(5.99928507671022,7.21246426313331,15.4323267873748));
#46826=CARTESIAN_POINT('Ctrl Pts',(5.99928507671022,6.18849730659679,14.3709116157364));
#46827=CARTESIAN_POINT('Ctrl Pts',(5.99928507671022,5.3327105314028,13.1688951809427));
#46828=CARTESIAN_POINT('Ctrl Pts',(5.99928507671022,4.66383020186651,11.8527237226933));
#46829=CARTESIAN_POINT('Ctrl Pts',(5.99928507671022,4.224790911033,10.5321726316798));
#46830=CARTESIAN_POINT('Ctrl Pts',(5.99928507671022,4.05899861711237,9.64833292798276));
#46831=CARTESIAN_POINT('Ctrl Pts',(5.99928507671022,4.00882230478759,9.24471639752885));
#46832=CARTESIAN_POINT('Ctrl Pts',(6.0106308763342,9.70160290773497,17.2272498486038));
#46833=CARTESIAN_POINT('Ctrl Pts',(6.0106308763342,9.67076783714877,17.2134071734354));
#46834=CARTESIAN_POINT('Ctrl Pts',(6.0106308763342,9.18470187459673,16.9922547580898));
#46835=CARTESIAN_POINT('Ctrl Pts',(6.0106308763342,8.27768603745146,16.4894560547017));
#46836=CARTESIAN_POINT('Ctrl Pts',(6.0106308763342,7.08568030104689,15.5741219743995));
#46837=CARTESIAN_POINT('Ctrl Pts',(6.0106308763342,6.04221997992615,14.4924954167108));
#46838=CARTESIAN_POINT('Ctrl Pts',(6.0106308763342,5.16996731271864,13.2673652494844));
#46839=CARTESIAN_POINT('Ctrl Pts',(6.0106308763342,4.4883276541397,11.9260693537073));
#46840=CARTESIAN_POINT('Ctrl Pts',(6.0106308763342,4.04084623666606,10.5801434939708));
#46841=CARTESIAN_POINT('Ctrl Pts',(6.0106308763342,3.87189639823667,9.67946934988362));
#46842=CARTESIAN_POINT('Ctrl Pts',(6.0106308763342,3.82075680084142,9.26809143104854));
#46843=CARTESIAN_POINT('Ctrl Pts',(5.90351527979004,9.63722337780829,17.3706925625164));
#46844=CARTESIAN_POINT('Ctrl Pts',(5.90351527979004,9.60590604384287,17.3566332201771));
#46845=CARTESIAN_POINT('Ctrl Pts',(5.90351527979004,9.11224325005284,17.1320226838286));
#46846=CARTESIAN_POINT('Ctrl Pts',(5.90351527979004,8.19119664256615,16.6214533871243));
#46847=CARTESIAN_POINT('Ctrl Pts',(5.90351527979004,6.98049513891304,15.6917610629));
#46848=CARTESIAN_POINT('Ctrl Pts',(5.90351527979004,5.92086232498848,14.5933663124247));
#46849=CARTESIAN_POINT('Ctrl Pts',(5.90351527979004,5.03494888009271,13.3490600471091));
#46850=CARTESIAN_POINT('Ctrl Pts',(5.90351527979004,4.34272356011029,11.9869198900282));
#46851=CARTESIAN_POINT('Ctrl Pts',(5.90351527979004,3.88823820897759,10.6199420839871));
#46852=CARTESIAN_POINT('Ctrl Pts',(5.90351527979004,3.71666874243767,9.70530139939471));
#46853=CARTESIAN_POINT('Ctrl Pts',(5.90351527979004,3.66472996433574,9.28748431521313));
#46854=CARTESIAN_POINT('Ctrl Pts',(5.72195022899939,9.61342435717959,17.42371867364));
#46855=CARTESIAN_POINT('Ctrl Pts',(5.72195022899939,9.5819287461083,17.4095792364841));
#46856=CARTESIAN_POINT('Ctrl Pts',(5.72195022899939,9.08545765061893,17.1836903451488));
#46857=CARTESIAN_POINT('Ctrl Pts',(5.72195022899939,8.15922432316945,16.6702485125462));
#46858=CARTESIAN_POINT('Ctrl Pts',(5.72195022899939,6.94161160176299,15.7352484120208));
#46859=CARTESIAN_POINT('Ctrl Pts',(5.72195022899939,5.87600034267062,14.6306550054462));
#46860=CARTESIAN_POINT('Ctrl Pts',(5.72195022899939,4.98503695207054,13.379259959662));
#46861=CARTESIAN_POINT('Ctrl Pts',(5.72195022899939,4.28889845698094,12.0094143563736));
#46862=CARTESIAN_POINT('Ctrl Pts',(5.72195022899939,3.83182397912037,10.634654329726));
#46863=CARTESIAN_POINT('Ctrl Pts',(5.72195022899939,3.65928612117585,9.71485066885913));
#46864=CARTESIAN_POINT('Ctrl Pts',(5.72195022899939,3.60705191193102,9.2946532344466));
#46865=CARTESIAN_POINT('',(5.999995708873,3.99788407334609,9.34660788812901));
#46866=CARTESIAN_POINT('Ctrl Pts',(5.99999999999973,9.67863108609234,17.0348569101268));
#46867=CARTESIAN_POINT('Ctrl Pts',(5.99999999999973,9.53996482697851,16.9709229523272));
#46868=CARTESIAN_POINT('Ctrl Pts',(6.00000000003745,9.40322990797334,16.9040238345851));
#46869=CARTESIAN_POINT('Ctrl Pts',(5.99999999795223,9.26832001839706,16.8341585314163));
#46870=CARTESIAN_POINT('Ctrl Pts',(5.99999999586008,9.13296247354946,16.7640614026095));
#46871=CARTESIAN_POINT('Ctrl Pts',(5.99999999148617,8.99944169513547,16.6909781287824));
#46872=CARTESIAN_POINT('Ctrl Pts',(5.99999999087358,8.86767321977893,16.614860483692));
#46873=CARTESIAN_POINT('Ctrl Pts',(5.99999999026198,8.73611954089724,16.5388669183695));
#46874=CARTESIAN_POINT('Ctrl Pts',(5.99999999695625,8.60631206863277,16.4598486138468));
#46875=CARTESIAN_POINT('Ctrl Pts',(5.99999999953313,8.47819538350943,16.3777143843333));
#46876=CARTESIAN_POINT('Ctrl Pts',(5.99999999982103,8.46388161372689,16.368537980406));
#46877=CARTESIAN_POINT('Ctrl Pts',(5.99999999999973,8.44958898200459,16.359322640206));
#46878=CARTESIAN_POINT('Ctrl Pts',(5.99999999999973,8.43531743665976,16.3500682051006));
#46879=CARTESIAN_POINT('Ctrl Pts',(5.99999999999973,8.41951507644111,16.3398211075634));
#46880=CARTESIAN_POINT('Ctrl Pts',(5.99999999977974,8.40373799579134,16.3295268932048));
#46881=CARTESIAN_POINT('Ctrl Pts',(5.99999999940211,8.38798676299758,16.3191857879634));
#46882=CARTESIAN_POINT('Ctrl Pts',(5.99999999572733,8.23470703683931,16.218553551723));
#46883=CARTESIAN_POINT('Ctrl Pts',(5.99999998184256,8.08387696920508,16.1134769902102));
#46884=CARTESIAN_POINT('Ctrl Pts',(5.99999998033334,7.93593246473448,16.0042029928132));
#46885=CARTESIAN_POINT('Ctrl Pts',(5.99999997882271,7.78785045815604,15.8948274343273));
#46886=CARTESIAN_POINT('Ctrl Pts',(5.99999998731003,7.64265976295762,15.7812468735777));
#46887=CARTESIAN_POINT('Ctrl Pts',(5.99999999411985,7.5007707703766,15.6637536647565));
#46888=CARTESIAN_POINT('Ctrl Pts',(5.99999999739301,7.43257160181644,15.6072803682216));
#46889=CARTESIAN_POINT('Ctrl Pts',(5.99999999999973,7.36513478078999,15.5499037886171));
#46890=CARTESIAN_POINT('Ctrl Pts',(5.99999999999973,7.29850328839949,15.4916598064483));
#46891=CARTESIAN_POINT('Ctrl Pts',(5.99999999999973,7.27238327152499,15.4688277529777));
#46892=CARTESIAN_POINT('Ctrl Pts',(5.99999999960413,7.24638785264082,15.4458614503161));
#46893=CARTESIAN_POINT('Ctrl Pts',(5.99999999898864,7.22051776537669,15.4227616312461));
#46894=CARTESIAN_POINT('Ctrl Pts',(5.99999999507859,7.05617055376932,15.276013349571));
#46895=CARTESIAN_POINT('Ctrl Pts',(5.99999998615654,6.89687872218253,15.1238800776715));
#46896=CARTESIAN_POINT('Ctrl Pts',(5.99999998771983,6.74283048209746,14.9666009211881));
#46897=CARTESIAN_POINT('Ctrl Pts',(5.99999998928313,6.58878224201239,14.8093217647046));
#46898=CARTESIAN_POINT('Ctrl Pts',(5.99999999999973,6.43997714680652,14.6468962856073));
#46899=CARTESIAN_POINT('Ctrl Pts',(5.99999999999973,6.29664110038306,14.4795249794001));
#46900=CARTESIAN_POINT('Ctrl Pts',(5.99999999999973,6.26385436913115,14.4412404154483));
#46901=CARTESIAN_POINT('Ctrl Pts',(5.99999999934668,6.23135170199707,14.4026986427203));
#46902=CARTESIAN_POINT('Ctrl Pts',(5.99999999845572,6.19913907434236,14.363905280557));
#46903=CARTESIAN_POINT('Ctrl Pts',(5.99999999449761,6.05603309717716,14.1915641086601));
#46904=CARTESIAN_POINT('Ctrl Pts',(5.99999998895131,5.91865446118546,14.0142547237431));
#46905=CARTESIAN_POINT('Ctrl Pts',(5.99999999115152,5.78742187753508,13.8325315583979));
#46906=CARTESIAN_POINT('Ctrl Pts',(5.99999999312719,5.66958213385772,13.6693540103466));
#46907=CARTESIAN_POINT('Ctrl Pts',(5.99999999999973,5.55669768563095,13.5026183339827));
#46908=CARTESIAN_POINT('Ctrl Pts',(5.99999999999973,5.44904317681685,13.3327476292601));
#46909=CARTESIAN_POINT('Ctrl Pts',(5.99999999999973,5.41325256681909,13.2762727429805));
#46910=CARTESIAN_POINT('Ctrl Pts',(5.99999999913626,5.37804226723512,13.2194505286227));
#46911=CARTESIAN_POINT('Ctrl Pts',(5.99999999780773,5.34341678808384,13.1622879102264));
#46912=CARTESIAN_POINT('Ctrl Pts',(5.99999999336881,5.22772507043026,12.971294408622));
#46913=CARTESIAN_POINT('Ctrl Pts',(5.99999998477713,5.11855861819962,12.7765024096211));
#46914=CARTESIAN_POINT('Ctrl Pts',(5.99999998688352,5.01608477820067,12.5781968544433));
#46915=CARTESIAN_POINT('Ctrl Pts',(5.99999998863007,4.93111681483905,12.4137683608206));
#46916=CARTESIAN_POINT('Ctrl Pts',(5.99999999999973,4.85075089138975,12.2469236106697));
#46917=CARTESIAN_POINT('Ctrl Pts',(5.99999999999973,4.77510784589458,12.0778154581379));
#46918=CARTESIAN_POINT('Ctrl Pts',(5.99999999999973,4.74092204835138,12.001389436056));
#46919=CARTESIAN_POINT('Ctrl Pts',(5.99999999683353,4.70768988233517,11.924503809641));
#46920=CARTESIAN_POINT('Ctrl Pts',(5.99999999319074,4.67543337998425,11.8471991538665));
#46921=CARTESIAN_POINT('Ctrl Pts',(5.99999998466666,4.59995360841245,11.6663073232577));
#46922=CARTESIAN_POINT('Ctrl Pts',(5.99999997595978,4.52981981238128,11.4831198183697));
#46923=CARTESIAN_POINT('Ctrl Pts',(5.99999997954453,4.4651956975605,11.2981805868859));
#46924=CARTESIAN_POINT('Ctrl Pts',(5.99999998312928,4.40057158273971,11.1132413554021));
#46925=CARTESIAN_POINT('Ctrl Pts',(5.99999999999973,4.34145727180275,10.9265509189428));
#46926=CARTESIAN_POINT('Ctrl Pts',(5.99999999999973,4.2879615125261,10.7386680750648));
#46927=CARTESIAN_POINT('Ctrl Pts',(5.99999999999973,4.2606285677341,10.6426718415593));
#46928=CARTESIAN_POINT('Ctrl Pts',(5.99999999545167,4.23478514967479,10.5463642320464));
#46929=CARTESIAN_POINT('Ctrl Pts',(5.99999999307292,4.2104123041608,10.4497165385551));
#46930=CARTESIAN_POINT('Ctrl Pts',(5.99999998940938,4.17287556936319,10.3008689681184));
#46931=CARTESIAN_POINT('Ctrl Pts',(5.99999999031161,4.13882446531637,10.151215309579));
#46932=CARTESIAN_POINT('Ctrl Pts',(5.99999999276242,4.10822755632143,10.0006714395986));
#46933=CARTESIAN_POINT('Ctrl Pts',(5.99999999520027,4.0777923342782,9.85092310682235));
#46934=CARTESIAN_POINT('Ctrl Pts',(5.99999999786782,4.05077479935226,9.70029349538257));
#46935=CARTESIAN_POINT('Ctrl Pts',(5.99999999875693,4.02719432996178,9.54868945906619));
#46936=CARTESIAN_POINT('Ctrl Pts',(5.99999999915083,4.01674728370481,9.48152309550002));
#46937=CARTESIAN_POINT('Ctrl Pts',(5.99999999931875,4.00697554674536,9.4141653731669));
#46938=CARTESIAN_POINT('Ctrl Pts',(5.99999999931447,3.99788407309719,9.34660788816251));
#46939=CARTESIAN_POINT('',(5.732785250275,3.68906751028189,9.81543787979773));
#46940=CARTESIAN_POINT('Ctrl Pts',(5.73644276397758,9.52121697613018,17.3763304378322));
#46941=CARTESIAN_POINT('Ctrl Pts',(5.73708792253423,9.11866917743972,17.1904707590909));
#46942=CARTESIAN_POINT('Ctrl Pts',(5.7376256311299,8.72821037826326,16.9787094793335));
#46943=CARTESIAN_POINT('Ctrl Pts',(5.73805595545524,8.35333662058844,16.7430677587439));
#46944=CARTESIAN_POINT('Ctrl Pts',(5.73812189676484,8.29589235108936,16.7069588921571));
#46945=CARTESIAN_POINT('Ctrl Pts',(5.7381853165236,8.23881395572367,16.6702892265697));
#46946=CARTESIAN_POINT('Ctrl Pts',(5.73824621493853,8.18211392296712,16.6330659762314));
#46947=CARTESIAN_POINT('Ctrl Pts',(5.7386514731337,7.80479453019456,16.3853579321291));
#46948=CARTESIAN_POINT('Ctrl Pts',(5.73894507723332,7.44423382954565,16.1131376200729));
#46949=CARTESIAN_POINT('Ctrl Pts',(5.73912707304862,7.10336506027343,15.8189084737335));
#46950=CARTESIAN_POINT('Ctrl Pts',(5.73915087280096,7.05878935244757,15.7804318702914));
#46951=CARTESIAN_POINT('Ctrl Pts',(5.73917276389451,7.01455034381636,15.7415788431653));
#46952=CARTESIAN_POINT('Ctrl Pts',(5.73919274639104,6.97065454663181,15.7023549458792));
#46953=CARTESIAN_POINT('Ctrl Pts',(5.73934700322414,6.63179665406559,15.3995622407664));
#46954=CARTESIAN_POINT('Ctrl Pts',(5.73938752574635,6.31339410984921,15.0746719519374));
#46955=CARTESIAN_POINT('Ctrl Pts',(5.73931432087574,6.01802949013874,14.7306311257563));
#46956=CARTESIAN_POINT('Ctrl Pts',(5.73930537009204,5.98191516059527,14.688565140381));
#46957=CARTESIAN_POINT('Ctrl Pts',(5.73929471903226,5.94614520943738,14.646212803436));
#46958=CARTESIAN_POINT('Ctrl Pts',(5.73928236766916,5.91072432464435,14.6035794599326));
#46959=CARTESIAN_POINT('Ctrl Pts',(5.7391813575988,5.62105054233214,14.2549218265221));
#46960=CARTESIAN_POINT('Ctrl Pts',(5.73896663328804,5.35472454602451,13.8874741273139));
#46961=CARTESIAN_POINT('Ctrl Pts',(5.73863815938408,5.11384108228221,13.5046257890557));
#46962=CARTESIAN_POINT('Ctrl Pts',(5.73859603620214,5.08295041533258,13.4555296812299));
#46963=CARTESIAN_POINT('Ctrl Pts',(5.73855204233368,5.05247812384846,13.4061802442968));
#46964=CARTESIAN_POINT('Ctrl Pts',(5.73850617766587,5.02242859618563,13.3565845722194));
#46965=CARTESIAN_POINT('Ctrl Pts',(5.73815298353459,4.7910235228329,12.9746587641395));
#46966=CARTESIAN_POINT('Ctrl Pts',(5.73768884855725,4.58469079279698,12.5781343479219));
#46967=CARTESIAN_POINT('Ctrl Pts',(5.73711370893166,4.40507707792291,12.1703805322858));
#46968=CARTESIAN_POINT('Ctrl Pts',(5.73703020600002,4.37899945939716,12.1111798834711));
#46969=CARTESIAN_POINT('Ctrl Pts',(5.73694436300226,4.35348502659766,12.0517424478515));
#46970=CARTESIAN_POINT('Ctrl Pts',(5.73685617975238,4.32853878647124,11.9920784594305));
#46971=CARTESIAN_POINT('Ctrl Pts',(5.73622837166435,4.15093758284581,11.5673091914781));
#46972=CARTESIAN_POINT('Ctrl Pts',(5.73548194665821,4.00213608247109,11.1310612655917));
#46973=CARTESIAN_POINT('Ctrl Pts',(5.73461683945432,3.88305444394366,10.6872940893152));
#46974=CARTESIAN_POINT('Ctrl Pts',(5.73452245510481,3.87006247839285,10.6388784986493));
#46975=CARTESIAN_POINT('Ctrl Pts',(5.73442665808298,3.85742426259303,10.5903733553511));
#46976=CARTESIAN_POINT('Ctrl Pts',(5.73432944831777,3.84514098508373,10.5417837646067));
#46977=CARTESIAN_POINT('Ctrl Pts',(5.73384873488381,3.78439876953865,10.3015026676433));
#46978=CARTESIAN_POINT('Ctrl Pts',(5.73333347371323,3.73233632290025,10.05915688844));
#46979=CARTESIAN_POINT('Ctrl Pts',(5.73278365815454,3.68907196536841,9.81543709253676));
#46980=CARTESIAN_POINT('Ctrl Pts',(5.99999999931447,3.99788407309719,9.3466078881625));
#46981=CARTESIAN_POINT('Ctrl Pts',(5.99999921905452,3.98578558819822,9.35665170909537));
#46982=CARTESIAN_POINT('Ctrl Pts',(5.99933245555486,3.97325817756116,9.36759536657576));
#46983=CARTESIAN_POINT('Ctrl Pts',(5.99783142449878,3.96039551133393,9.37944935506896));
#46984=CARTESIAN_POINT('Ctrl Pts',(5.99639504223158,3.94808683483931,9.39079279716379));
#46985=CARTESIAN_POINT('Ctrl Pts',(5.99419378268927,3.93547109215435,9.40296993155199));
#46986=CARTESIAN_POINT('Ctrl Pts',(5.99108408909626,3.92267709122614,9.41598364189161));
#46987=CARTESIAN_POINT('Ctrl Pts',(5.98929042384455,3.91529753622859,9.42348992485284));
#46988=CARTESIAN_POINT('Ctrl Pts',(5.98719466025372,3.90785956790051,9.43127440764121));
#46989=CARTESIAN_POINT('Ctrl Pts',(5.98477186618435,3.90039536693395,9.43933646513942));
#46990=CARTESIAN_POINT('Ctrl Pts',(5.98071484714981,3.88789640724855,9.4528365480154));
#46991=CARTESIAN_POINT('Ctrl Pts',(5.97573805800257,3.87531381301812,9.46710865485213));
#46992=CARTESIAN_POINT('Ctrl Pts',(5.96972968522987,3.86280213529356,9.48211836184687));
#46993=CARTESIAN_POINT('Ctrl Pts',(5.96758326184623,3.85833247958935,9.48748041032386));
#46994=CARTESIAN_POINT('Ctrl Pts',(5.96530538179708,3.85387229884052,9.49293650756601));
#46995=CARTESIAN_POINT('Ctrl Pts',(5.96289174885348,3.84943004700347,9.49848479322591));
#46996=CARTESIAN_POINT('Ctrl Pts',(5.95830675299446,3.84099143734185,9.50902445164523));
#46997=CARTESIAN_POINT('Ctrl Pts',(5.95323089635072,3.83261536357627,9.51989644938458));
#46998=CARTESIAN_POINT('Ctrl Pts',(5.94763509895936,3.82435832537359,9.53108169525198));
#46999=CARTESIAN_POINT('Ctrl Pts',(5.94483720026369,3.82022980627226,9.53667431818568));
#47000=CARTESIAN_POINT('Ctrl Pts',(5.94190933196359,3.81613107762387,9.54234524794495));
#47001=CARTESIAN_POINT('Ctrl Pts',(5.93884846234065,3.81207003683764,9.54809147636354));
#47002=CARTESIAN_POINT('Ctrl Pts',(5.93731802752919,3.81003951644452,9.55096459057283));
#47003=CARTESIAN_POINT('Ctrl Pts',(5.93575434414046,3.80801841801275,9.55385652942552));
#47004=CARTESIAN_POINT('Ctrl Pts',(5.93415706120959,3.80600775380745,9.55676689546259));
#47005=CARTESIAN_POINT('Ctrl Pts',(5.93309249680217,3.80466767716424,9.55870660948305));
#47006=CARTESIAN_POINT('Ctrl Pts',(5.93174397974193,3.80300201583821,9.56113909554917));
#47007=CARTESIAN_POINT('Ctrl Pts',(5.93064736237428,3.80167271211161,9.56309525086169));
#47008=CARTESIAN_POINT('Ctrl Pts',(5.93009860423359,3.80100751542319,9.5640741302629));
#47009=CARTESIAN_POINT('Ctrl Pts',(5.92961384298516,3.80042591251214,9.56493376387943));
#47010=CARTESIAN_POINT('Ctrl Pts',(5.92926407743291,3.80000808667201,9.56555286688789));
#47011=CARTESIAN_POINT('Ctrl Pts',(5.9237222231917,3.79338785237691,9.57536223379416));
#47012=CARTESIAN_POINT('Ctrl Pts',(5.91756027126521,3.78661920970786,9.58594208419168));
#47013=CARTESIAN_POINT('Ctrl Pts',(5.91064191769737,3.77975689027944,9.59724510500674));
#47014=CARTESIAN_POINT('Ctrl Pts',(5.90401867363957,3.77318729016703,9.60806598380606));
#47015=CARTESIAN_POINT('Ctrl Pts',(5.89670135644846,3.76653153860572,9.61954976307286));
#47016=CARTESIAN_POINT('Ctrl Pts',(5.88856867051108,3.75988379433895,9.63164686285785));
#47017=CARTESIAN_POINT('Ctrl Pts',(5.88075741804393,3.75349879322067,9.64326584104889));
#47018=CARTESIAN_POINT('Ctrl Pts',(5.87219301358668,3.74712115240292,9.65545068612455));
#47019=CARTESIAN_POINT('Ctrl Pts',(5.86277924073904,3.74088016718042,9.66814856503587));
#47020=CARTESIAN_POINT('Ctrl Pts',(5.8538529024773,3.73496233316379,9.68018896203755));
#47021=CARTESIAN_POINT('Ctrl Pts',(5.844162003248,3.72916776719875,9.69269062627937));
#47022=CARTESIAN_POINT('Ctrl Pts',(5.83364789820362,3.72364591984021,9.70559998642325));
#47023=CARTESIAN_POINT('Ctrl Pts',(5.82342631893895,3.71827770255262,9.71815017946487));
#47024=CARTESIAN_POINT('Ctrl Pts',(5.8124258371083,3.71316782542568,9.73108564878583));
#47025=CARTESIAN_POINT('Ctrl Pts',(5.80062802127563,3.70848480610254,9.74434929261022));
#47026=CARTESIAN_POINT('Ctrl Pts',(5.78926063509769,3.70397264131883,9.75712902774231));
#47027=CARTESIAN_POINT('Ctrl Pts',(5.77715249409862,3.69985766044913,9.77021329910403));
#47028=CARTESIAN_POINT('Ctrl Pts',(5.76433060935114,3.69630904301238,9.78354493083899));
#47029=CARTESIAN_POINT('Ctrl Pts',(5.75424393196645,3.69351742852269,9.79403261427793));
#47030=CARTESIAN_POINT('Ctrl Pts',(5.74371633829686,3.69107690256356,9.80467322214807));
#47031=CARTESIAN_POINT('Ctrl Pts',(5.73278365815454,3.68907196536841,9.81543709253676));
#47032=CARTESIAN_POINT('Ctrl Pts',(6.05076794927297,4.09458203878362,9.54441225412628));
#47033=CARTESIAN_POINT('Ctrl Pts',(6.05141961089931,4.06988665095652,9.55471205249664));
#47034=CARTESIAN_POINT('Ctrl Pts',(6.04716305939897,4.00788049666569,9.58295885528607));
#47035=CARTESIAN_POINT('Ctrl Pts',(6.01566649547382,3.90953592463721,9.63753455351153));
#47036=CARTESIAN_POINT('Ctrl Pts',(5.94752439895274,3.8106474887844,9.70652326956244));
#47037=CARTESIAN_POINT('Ctrl Pts',(5.84910136934098,3.73282443315672,9.77805722652396));
#47038=CARTESIAN_POINT('Ctrl Pts',(5.76414048183063,3.69951678478747,9.8252049164694));
#47039=CARTESIAN_POINT('Ctrl Pts',(5.71687785318494,3.68927674302881,9.84788773253446));
#47040=CARTESIAN_POINT('Ctrl Pts',(5.71192604303504,3.68828956961732,9.85022763652081));
#47041=CARTESIAN_POINT('Ctrl Pts',(5.91195109670203,3.98202506659494,9.28408186263919));
#47042=CARTESIAN_POINT('Ctrl Pts',(5.91254930560179,3.95979988492668,9.29334225786693));
#47043=CARTESIAN_POINT('Ctrl Pts',(5.9086455165599,3.9037959614243,9.3189084546854));
#47044=CARTESIAN_POINT('Ctrl Pts',(5.87945207765067,3.81435590889244,9.36894703351106));
#47045=CARTESIAN_POINT('Ctrl Pts',(5.81592785132783,3.724038797409,9.43278746526276));
#47046=CARTESIAN_POINT('Ctrl Pts',(5.72395388473843,3.65290980473349,9.4993131445599));
#47047=CARTESIAN_POINT('Ctrl Pts',(5.64456392614967,3.62258130620308,9.54323751898402));
#47048=CARTESIAN_POINT('Ctrl Pts',(5.6004601945523,3.61331530819896,9.56435979366266));
#47049=CARTESIAN_POINT('Ctrl Pts',(5.59584005632463,3.61242305635906,9.56653858267162));
#47050=CARTESIAN_POINT('Ctrl Pts',(6.02852321580189,3.87156862597752,9.01219535140232));
#47051=CARTESIAN_POINT('Ctrl Pts',(6.02946140921585,3.83732372353067,9.02648434185954));
#47052=CARTESIAN_POINT('Ctrl Pts',(6.02330612970468,3.7527205708333,9.0650283490567));
#47053=CARTESIAN_POINT('Ctrl Pts',(5.98006479999682,3.62281406661669,9.13695627061525));
#47054=CARTESIAN_POINT('Ctrl Pts',(5.88925135176173,3.49510413587073,9.22578449759683));
#47055=CARTESIAN_POINT('Ctrl Pts',(5.75973990848393,3.39553695641023,9.31721776716681));
#47056=CARTESIAN_POINT('Ctrl Pts',(5.64791312656201,3.35283377232076,9.37793571390397));
#47057=CARTESIAN_POINT('Ctrl Pts',(5.58525613648115,3.33967210674828,9.40750191109257));
#47058=CARTESIAN_POINT('Ctrl Pts',(5.57868611740273,3.33840311444834,9.41055623991342));
#47059=CARTESIAN_POINT('Ctrl Pts',(6.32407110292224,3.8356169056028,8.9069743206792));
#47060=CARTESIAN_POINT('Ctrl Pts',(6.32551985797543,3.78274129227489,8.92906365643331));
#47061=CARTESIAN_POINT('Ctrl Pts',(6.31598468883757,3.65368426869858,8.98773692499536));
#47062=CARTESIAN_POINT('Ctrl Pts',(6.25155285603629,3.46046613433746,9.09363216926371));
#47063=CARTESIAN_POINT('Ctrl Pts',(6.1194312004155,3.27391026506049,9.22120475071504));
#47064=CARTESIAN_POINT('Ctrl Pts',(5.93300158659274,3.12941390447521,9.35113453270944));
#47065=CARTESIAN_POINT('Ctrl Pts',(5.77199259259683,3.06709381628777,9.43765473932759));
#47066=CARTESIAN_POINT('Ctrl Pts',(5.68123186418643,3.04772038523933,9.48013432491254));
#47067=CARTESIAN_POINT('Ctrl Pts',(5.67170855993161,3.04584994414088,9.48452693128353));
#47068=CARTESIAN_POINT('',(5.72001553113216,3.07996593912288,9.45352621454216));
#47069=CARTESIAN_POINT('Origin',(5.89875807498483,3.22462412373647,9.89750210812564));
#47070=CARTESIAN_POINT('',(5.99999998860547,3.2142420421365,9.29218348100167));
#47071=CARTESIAN_POINT('Ctrl Pts',(6.00000005199697,3.21424211020075,9.29218367777145));
#47072=CARTESIAN_POINT('Ctrl Pts',(5.95914560526162,3.18372948881454,9.32022546602934));
#47073=CARTESIAN_POINT('Ctrl Pts',(5.91541907063108,3.15725519634921,9.34766265780539));
#47074=CARTESIAN_POINT('Ctrl Pts',(5.86878902309948,3.13479935800112,9.37455777546322));
#47075=CARTESIAN_POINT('Ctrl Pts',(5.82215897557027,3.11234351965418,9.40145289311967));
#47076=CARTESIAN_POINT('Ctrl Pts',(5.77262518198777,3.09390594889867,9.42780540507949));
#47077=CARTESIAN_POINT('Ctrl Pts',(5.72001606109867,3.0799663679684,9.45352753087965));
#47078=CARTESIAN_POINT('Ctrl Pts',(5.99998738510668,3.99788407452638,9.34660788723015));
#47079=CARTESIAN_POINT('Ctrl Pts',(5.99998486187692,3.97178788320407,9.33570712756464));
#47080=CARTESIAN_POINT('Ctrl Pts',(5.99998575125159,3.94579597545338,9.32564379782521));
#47081=CARTESIAN_POINT('Ctrl Pts',(5.9999822017208,3.91991001575388,9.31645115807804));
#47082=CARTESIAN_POINT('Ctrl Pts',(5.9999810788976,3.91172150915836,9.31354325000456));
#47083=CARTESIAN_POINT('Ctrl Pts',(5.99997928834179,3.90354373511738,9.31072213040201));
#47084=CARTESIAN_POINT('Ctrl Pts',(5.99997621692483,3.89537702176094,9.30798798286405));
#47085=CARTESIAN_POINT('Ctrl Pts',(5.99996211490638,3.85788060115839,9.29543449389021));
#47086=CARTESIAN_POINT('Ctrl Pts',(5.99992503046496,3.82061959459092,9.28471765012796));
#47087=CARTESIAN_POINT('Ctrl Pts',(5.99991423108138,3.78357227620041,9.27578205250742));
#47088=CARTESIAN_POINT('Ctrl Pts',(5.99990487784501,3.75148597024292,9.26804302221802));
#47089=CARTESIAN_POINT('Ctrl Pts',(5.99990278201534,3.71956006053042,9.26166526912885));
#47090=CARTESIAN_POINT('Ctrl Pts',(5.99990421744023,3.68780888196962,9.25664785673608));
#47091=CARTESIAN_POINT('Ctrl Pts',(5.99990515161368,3.66714523844375,9.25338252846148));
#47092=CARTESIAN_POINT('Ctrl Pts',(5.9999079344194,3.64655501788334,9.25069311330917));
#47093=CARTESIAN_POINT('Ctrl Pts',(5.9999154152975,3.62603165865102,9.24858460933612));
#47094=CARTESIAN_POINT('Ctrl Pts',(5.99991831505916,3.6180763291548,9.24776730434917));
#47095=CARTESIAN_POINT('Ctrl Pts',(5.99992637047819,3.60986152187724,9.24700704859185));
#47096=CARTESIAN_POINT('Ctrl Pts',(5.99993172018324,3.60175615292464,9.2463534189002));
#47097=CARTESIAN_POINT('Ctrl Pts',(5.99993713803719,3.59354753118767,9.24569146274173));
#47098=CARTESIAN_POINT('Ctrl Pts',(5.99993950798768,3.58545148438002,9.24513890584738));
#47099=CARTESIAN_POINT('Ctrl Pts',(5.99994451737532,3.57786718423949,9.24469687939468));
#47100=CARTESIAN_POINT('Ctrl Pts',(5.9999453511632,3.57660481486588,9.24462330627048));
#47101=CARTESIAN_POINT('Ctrl Pts',(5.99994629295721,3.57535665077325,9.24455268656537));
#47102=CARTESIAN_POINT('Ctrl Pts',(5.99994741064896,3.57412456268449,9.24448490010183));
#47103=CARTESIAN_POINT('Ctrl Pts',(5.99997420500839,3.54458778655221,9.24285985915166));
#47104=CARTESIAN_POINT('Ctrl Pts',(5.99996028565624,3.51545795299334,9.24253338015036));
#47105=CARTESIAN_POINT('Ctrl Pts',(5.99993572430989,3.48674258613422,9.2434249525757));
#47106=CARTESIAN_POINT('Ctrl Pts',(5.99991395264873,3.46128871938452,9.24421525993356));
#47107=CARTESIAN_POINT('Ctrl Pts',(5.99988491856864,3.43615941743387,9.24596289046136));
#47108=CARTESIAN_POINT('Ctrl Pts',(5.99986830472523,3.4113487813846,9.2486445826423));
#47109=CARTESIAN_POINT('Ctrl Pts',(5.99985059014699,3.38489433959829,9.25150394785762));
#47110=CARTESIAN_POINT('Ctrl Pts',(5.99984847396056,3.35880084002476,9.2554250847677));
#47111=CARTESIAN_POINT('Ctrl Pts',(5.99986814609541,3.33305940975811,9.26042190483073));
#47112=CARTESIAN_POINT('Ctrl Pts',(5.99988721410813,3.30810848685332,9.26526527487156));
#47113=CARTESIAN_POINT('Ctrl Pts',(5.99992732030962,3.28348762440651,9.2711201492481));
#47114=CARTESIAN_POINT('Ctrl Pts',(5.99996104571581,3.25920753570425,9.27802936166073));
#47115=CARTESIAN_POINT('Ctrl Pts',(5.99998205295688,3.24408369483654,9.28233304565181));
#47116=CARTESIAN_POINT('Ctrl Pts',(5.99999988351111,3.22909250348764,9.28704637806825));
#47117=CARTESIAN_POINT('Ctrl Pts',(5.99999988746152,3.2142419772354,9.29218329337644));
#47118=CARTESIAN_POINT('Ctrl Pts',(5.84420570955861,3.72282131685335,9.78165001835963));
#47119=CARTESIAN_POINT('Ctrl Pts',(5.38996562765094,3.59817429287799,10.0127664874412));
#47120=CARTESIAN_POINT('Ctrl Pts',(4.3608413144944,3.34562052197065,10.4582067183885));
#47121=CARTESIAN_POINT('Ctrl Pts',(2.69718314813897,3.05501779598387,10.9280508734159));
#47122=CARTESIAN_POINT('Ctrl Pts',(0.90123277416832,2.89428850134492,11.17270495048));
#47123=CARTESIAN_POINT('Ctrl Pts',(-0.898128982031577,2.8941485408364,11.1729135901656));
#47124=CARTESIAN_POINT('Ctrl Pts',(-2.69409800732445,3.05460699185379,10.9286891589027));
#47125=CARTESIAN_POINT('Ctrl Pts',(-4.35891886514342,3.3451779127716,10.4589598300149));
#47126=CARTESIAN_POINT('Ctrl Pts',(-5.38910342437971,3.59793551935265,10.0132112031376));
#47127=CARTESIAN_POINT('Ctrl Pts',(-5.84432165449578,3.72285318444294,9.78159102714844));
#47128=CARTESIAN_POINT('Ctrl Pts',(5.7253835366412,3.64453122286361,9.50229947997997));
#47129=CARTESIAN_POINT('Ctrl Pts',(5.28028699998817,3.52410865238856,9.72834256843305));
#47130=CARTESIAN_POINT('Ctrl Pts',(4.27190667605031,3.27990049730564,10.1641115674878));
#47131=CARTESIAN_POINT('Ctrl Pts',(2.64199881102779,2.99858776068898,10.6238561265337));
#47132=CARTESIAN_POINT('Ctrl Pts',(0.882754176675387,2.84291319818067,10.8632628192133));
#47133=CARTESIAN_POINT('Ctrl Pts',(-0.87971398644993,2.84277761987843,10.8634669836749));
#47134=CARTESIAN_POINT('Ctrl Pts',(-2.63897651280263,2.99818993802861,10.6244807187979));
#47135=CARTESIAN_POINT('Ctrl Pts',(-4.27002301198306,3.27947228142262,10.1648484281922));
#47136=CARTESIAN_POINT('Ctrl Pts',(-5.27944214962427,3.52387798467926,9.72877751971192));
#47137=CARTESIAN_POINT('Ctrl Pts',(-5.72549714712437,3.64456200849647,9.50224178643512));
#47138=CARTESIAN_POINT('Ctrl Pts',(5.71943787886701,3.37475784113534,9.34269929423411));
#47139=CARTESIAN_POINT('Ctrl Pts',(5.2756326248328,3.25566510720836,9.56644456769944));
#47140=CARTESIAN_POINT('Ctrl Pts',(4.26992144284517,3.01394111402995,9.99809686394945));
#47141=CARTESIAN_POINT('Ctrl Pts',(2.64237893294683,2.73488110526287,10.4543085477678));
#47142=CARTESIAN_POINT('Ctrl Pts',(0.88323656858176,2.58014446259695,10.6922727548935));
#47143=CARTESIAN_POINT('Ctrl Pts',(-0.880195053418905,2.58000959282474,
10.6924758250735));
#47144=CARTESIAN_POINT('Ctrl Pts',(-2.63935872061311,2.73448597878072,10.4549289906926));
#47145=CARTESIAN_POINT('Ctrl Pts',(-4.26804245262757,3.0135169461685,9.99882719418305));
#47146=CARTESIAN_POINT('Ctrl Pts',(-5.27479024948778,3.25543701995469,9.56687507681326));
#47147=CARTESIAN_POINT('Ctrl Pts',(-5.71955116480935,3.37478829409326,9.34264218643082));
#47148=CARTESIAN_POINT('Ctrl Pts',(5.83022605357272,3.08847457867854,9.40636717847527));
#47149=CARTESIAN_POINT('Ctrl Pts',(5.37902222649196,2.96695450753855,9.63208058929464));
#47150=CARTESIAN_POINT('Ctrl Pts',(4.35617397923863,2.72024194468582,10.0678408530508));
#47151=CARTESIAN_POINT('Ctrl Pts',(2.69807744090008,2.43493622270342,10.5293778616329));
#47152=CARTESIAN_POINT('Ctrl Pts',(0.902367232240108,2.27641231756555,10.7706401107682));
#47153=CARTESIAN_POINT('Ctrl Pts',(-0.899260324091646,2.27627402306329,
10.7708461773899));
#47154=CARTESIAN_POINT('Ctrl Pts',(-2.69499720433024,2.43453175827675,10.5300063904455));
#47155=CARTESIAN_POINT('Ctrl Pts',(-4.35426251968476,2.71980885391328,10.0685786090101));
#47156=CARTESIAN_POINT('Ctrl Pts',(-5.37816584285293,2.96672180164854,9.63251485973078));
#47157=CARTESIAN_POINT('Ctrl Pts',(-5.83034123540271,3.08850566402354,9.40630956456854));
#47158=CARTESIAN_POINT('',(-5.73278815913615,3.68906842472479,9.8154377369168));
#47159=CARTESIAN_POINT('',(-5.72001815309143,3.07996731954463,9.4535247212504));
#47160=CARTESIAN_POINT('Origin',(-5.89877627455651,3.22461269371084,9.89752154741546));
#47161=CARTESIAN_POINT('Ctrl Pts',(5.72001489176857,3.07996542174506,9.45352462645422));
#47162=CARTESIAN_POINT('Ctrl Pts',(5.48799480950505,3.01852056718121,9.56695266265951));
#47163=CARTESIAN_POINT('Ctrl Pts',(5.25105331740395,2.95922638303655,9.6737593363739));
#47164=CARTESIAN_POINT('Ctrl Pts',(5.0094050840325,2.90266822363824,9.77366018116699));
#47165=CARTESIAN_POINT('Ctrl Pts',(4.81759303552342,2.8577743038163,9.85295803251148));
#47166=CARTESIAN_POINT('Ctrl Pts',(4.62281550529396,2.81460478293779,9.92790410854663));
#47167=CARTESIAN_POINT('Ctrl Pts',(4.42518538965302,2.7734680793389,9.99833953918084));
#47168=CARTESIAN_POINT('Ctrl Pts',(4.40774373489348,2.76983759933948,10.0045557500047));
#47169=CARTESIAN_POINT('Ctrl Pts',(4.39027986594403,2.76622296211083,10.0107368187201));
#47170=CARTESIAN_POINT('Ctrl Pts',(4.37279389617178,2.76262438737662,10.0168826343622));
#47171=CARTESIAN_POINT('Ctrl Pts',(4.14017952315663,2.71475285285797,10.0986398986647));
#47172=CARTESIAN_POINT('Ctrl Pts',(3.90365739658418,2.66969955791451,10.1741666705095));
#47173=CARTESIAN_POINT('Ctrl Pts',(3.66348127988705,2.62785752322128,10.2432234915449));
#47174=CARTESIAN_POINT('Ctrl Pts',(3.54339322153849,2.60693650587466,10.2777519020626));
#47175=CARTESIAN_POINT('Ctrl Pts',(3.42239233379337,2.58681718649473,10.3106624654352));
#47176=CARTESIAN_POINT('Ctrl Pts',(3.3005145956988,2.56754188749553,10.3419232420058));
#47177=CARTESIAN_POINT('Ctrl Pts',(3.23957572665152,2.55790423799593,10.357553630291));
#47178=CARTESIAN_POINT('Ctrl Pts',(3.17841763997856,2.54847758767506,10.3727715469446));
#47179=CARTESIAN_POINT('Ctrl Pts',(3.11704519208393,2.53926669940264,10.3875729011152));
#47180=CARTESIAN_POINT('Ctrl Pts',(3.07988353782467,2.53368941094271,10.3965352747067));
#47181=CARTESIAN_POINT('Ctrl Pts',(3.04193898898731,2.52808742398809,10.4055108688518));
#47182=CARTESIAN_POINT('Ctrl Pts',(3.00449108092427,2.52265192508638,10.4141944648429));
#47183=CARTESIAN_POINT('Ctrl Pts',(2.98009379312151,2.51911070107907,10.4198518219962));
#47184=CARTESIAN_POINT('Ctrl Pts',(2.95590762246372,2.51563964095862,10.4253861653091));
#47185=CARTESIAN_POINT('Ctrl Pts',(2.93228963345293,2.51228602752607,10.4307231081398));
#47186=CARTESIAN_POINT('Ctrl Pts',(2.84332746939896,2.4996539313631,10.4508258350669));
#47187=CARTESIAN_POINT('Ctrl Pts',(2.7541295169341,2.48755127785995,10.4700011812909));
#47188=CARTESIAN_POINT('Ctrl Pts',(2.66471106197608,2.47599474546089,10.4882474435908));
#47189=CARTESIAN_POINT('Ctrl Pts',(2.40601906227546,2.44256112734122,10.5410347802055));
#47190=CARTESIAN_POINT('Ctrl Pts',(2.14548351135197,2.41369694976508,10.5860489111368));
#47191=CARTESIAN_POINT('Ctrl Pts',(1.8835937526012,2.38964917037043,10.6232802084062));
#47192=CARTESIAN_POINT('Ctrl Pts',(1.62209049315631,2.36563688090897,10.660456559386));
#47193=CARTESIAN_POINT('Ctrl Pts',(1.35923647871264,2.34642645776671,10.6898731463566));
#47194=CARTESIAN_POINT('Ctrl Pts',(1.09549640146985,2.33228549305395,10.7114791845455));
#47195=CARTESIAN_POINT('Ctrl Pts',(1.02640032222961,2.32858076516981,10.7171396535284));
#47196=CARTESIAN_POINT('Ctrl Pts',(0.95724333138418,2.32522411743047,10.7222638094589));
#47197=CARTESIAN_POINT('Ctrl Pts',(0.888033601990727,2.32222065282843,10.7268502548576));
#47198=CARTESIAN_POINT('Ctrl Pts',(0.625306294401089,2.31081918983688,10.744260877057));
#47199=CARTESIAN_POINT('Ctrl Pts',(0.361819606584868,2.30450503961765,10.7539262208446));
#47200=CARTESIAN_POINT('Ctrl Pts',(0.0980851516409874,2.30324908729893,
10.7558476291474));
#47201=CARTESIAN_POINT('Ctrl Pts',(0.0653985927216461,2.30309342785173,
10.7560857634697));
#47202=CARTESIAN_POINT('Ctrl Pts',(0.0327082200821129,2.30301550054985,
10.7562048927606));
#47203=CARTESIAN_POINT('Ctrl Pts',(1.50025002827934E-5,2.30301528050426,
10.7562049732159));
#47204=CARTESIAN_POINT('Ctrl Pts',(-0.260402583971723,2.30301352773274,
10.7562056140815));
#47205=CARTESIAN_POINT('Ctrl Pts',(-0.520628077614817,2.30794945072763,
10.7486542432409));
#47206=CARTESIAN_POINT('Ctrl Pts',(-0.780180801991693,2.31782837820034,
10.7335597513319));
#47207=CARTESIAN_POINT('Ctrl Pts',(-0.81512385878719,2.31915835816717,10.7315276105045));
#47208=CARTESIAN_POINT('Ctrl Pts',(-0.850054718196095,2.32057797102278,
10.7293586884452));
#47209=CARTESIAN_POINT('Ctrl Pts',(-0.884972201923496,2.3220872693386,10.7270529467002));
#47210=CARTESIAN_POINT('Ctrl Pts',(-1.08302033513938,2.33064784364132,10.7139750327288));
#47211=CARTESIAN_POINT('Ctrl Pts',(-1.2806384511707,2.34209289818217,10.6964967557869));
#47212=CARTESIAN_POINT('Ctrl Pts',(-1.47763989231892,2.3562977959534,10.674647479821));
#47213=CARTESIAN_POINT('Ctrl Pts',(-1.72250309886319,2.37395379276554,10.6474898928383));
#47214=CARTESIAN_POINT('Ctrl Pts',(-1.966400611854,2.3959245489063,10.6135703251249));
#47215=CARTESIAN_POINT('Ctrl Pts',(-2.20895642300066,2.4220042870364,10.5729124602434));
#47216=CARTESIAN_POINT('Ctrl Pts',(-2.33023432857398,2.43504415610144,10.5525835278027));
#47217=CARTESIAN_POINT('Ctrl Pts',(-2.45117699628968,2.44910990931528,10.530569817162));
#47218=CARTESIAN_POINT('Ctrl Pts',(-2.57173853619459,2.46416754251723,10.5068730018646));
#47219=CARTESIAN_POINT('Ctrl Pts',(-2.6017328859219,2.46791371162457,10.500977501807));
#47220=CARTESIAN_POINT('Ctrl Pts',(-2.63170369420663,2.47172120300045,10.4949778228535));
#47221=CARTESIAN_POINT('Ctrl Pts',(-2.66165016511053,2.47558955193389,10.4888739720703));
#47222=CARTESIAN_POINT('Ctrl Pts',(-2.6918882402914,2.4794955689818,10.4827106849347));
#47223=CARTESIAN_POINT('Ctrl Pts',(-2.7221015017876,2.48346363461805,10.4764411873324));
#47224=CARTESIAN_POINT('Ctrl Pts',(-2.75228934779513,2.48749300356865,10.4700655732347));
#47225=CARTESIAN_POINT('Ctrl Pts',(-2.78882912694254,2.4923702065172,10.4623484432678));
#47226=CARTESIAN_POINT('Ctrl Pts',(-2.82462118325018,2.49724024702851,10.4546297236668));
#47227=CARTESIAN_POINT('Ctrl Pts',(-2.86096121657739,2.5022776069016,10.446631522554));
#47228=CARTESIAN_POINT('Ctrl Pts',(-2.88437730122785,2.50552348298931,10.4414777971124));
#47229=CARTESIAN_POINT('Ctrl Pts',(-2.908020652911,2.50883932056307,10.4362071803145));
#47230=CARTESIAN_POINT('Ctrl Pts',(-2.93223485551304,2.51227720699284,10.4307356970442));
#47231=CARTESIAN_POINT('Ctrl Pts',(-3.18816992375771,2.54861438119102,10.3729041645668));
#47232=CARTESIAN_POINT('Ctrl Pts',(-3.44048848520818,2.58887347579288,10.3078290569615));
#47233=CARTESIAN_POINT('Ctrl Pts',(-3.68889603981782,2.63253044431277,10.2358289104327));
#47234=CARTESIAN_POINT('Ctrl Pts',(-3.93730359442746,2.67618741283266,10.1638287639039));
#47235=CARTESIAN_POINT('Ctrl Pts',(-4.18180036782967,2.72324271279475,10.0849034043995));
#47236=CARTESIAN_POINT('Ctrl Pts',(-4.42209432422583,2.77321168723325,9.99933375784427));
#47237=CARTESIAN_POINT('Ctrl Pts',(-4.67323483047252,2.8254361947711,9.90990161116226));
#47238=CARTESIAN_POINT('Ctrl Pts',(-4.91978515228066,2.88084356156688,9.81321196147461));
#47239=CARTESIAN_POINT('Ctrl Pts',(-5.16150816290815,2.93892462402289,9.70955603679204));
#47240=CARTESIAN_POINT('Ctrl Pts',(-5.35067345013844,2.98437714769289,9.62843797229831));
#47241=CARTESIAN_POINT('Ctrl Pts',(-5.53688233523973,3.03146792259273,9.54305277196725));
#47242=CARTESIAN_POINT('Ctrl Pts',(-5.72001751640012,3.07996680432955,9.4535231397943));
#47243=CARTESIAN_POINT('Ctrl Pts',(5.7327878508998,3.68906023344589,9.8154391656489));
#47244=CARTESIAN_POINT('Ctrl Pts',(5.30941801079182,3.57389352473303,10.0199549438219));
#47245=CARTESIAN_POINT('Ctrl Pts',(4.87321266289563,3.46710832616739,10.2012597279903));
#47246=CARTESIAN_POINT('Ctrl Pts',(4.42676988928123,3.37162421611693,10.3585398299166));
#47247=CARTESIAN_POINT('Ctrl Pts',(3.97538576906854,3.27508326270317,10.5175607495749));
#47248=CARTESIAN_POINT('Ctrl Pts',(3.51353578308825,3.19009467841088,10.6520220699274));
#47249=CARTESIAN_POINT('Ctrl Pts',(3.04423925012539,3.11963046164668,10.7611848420038));
#47250=CARTESIAN_POINT('Ctrl Pts',(3.01496106880174,3.11523438375063,10.7679952213911));
#47251=CARTESIAN_POINT('Ctrl Pts',(2.98565389961434,3.11089484111177,10.7747071184131));
#47252=CARTESIAN_POINT('Ctrl Pts',(2.95631847406784,3.10661255698121,10.7813203473808));
#47253=CARTESIAN_POINT('Ctrl Pts',(2.85795171409622,3.09225331700585,10.8034956488935));
#47254=CARTESIAN_POINT('Ctrl Pts',(2.75926725078899,3.07853787660286,10.8245615546286));
#47255=CARTESIAN_POINT('Ctrl Pts',(2.66029265310875,3.06549352193883,10.8445110040261));
#47256=CARTESIAN_POINT('Ctrl Pts',(2.18170270998425,3.00241777216995,10.9409762191043));
#47257=CARTESIAN_POINT('Ctrl Pts',(1.69632932885789,2.95503173038643,11.0113404250582));
#47258=CARTESIAN_POINT('Ctrl Pts',(1.2078115150959,2.9253399419601,11.0551347613053));
#47259=CARTESIAN_POINT('Ctrl Pts',(1.10052561963786,2.91881917645405,11.0647526594615));
#47260=CARTESIAN_POINT('Ctrl Pts',(0.993088047838054,2.91315189485321,11.0730888880343));
#47261=CARTESIAN_POINT('Ctrl Pts',(0.885537321098461,2.90835946256806,11.080138173233));
#47262=CARTESIAN_POINT('Ctrl Pts',(0.395429725259918,2.88652039614146,11.1122616960193));
#47263=CARTESIAN_POINT('Ctrl Pts',(-0.0970276312894777,2.88284672761108,
11.1176640421829));
#47264=CARTESIAN_POINT('Ctrl Pts',(-0.587926624973332,2.89733815422664,
11.096349233134));
#47265=CARTESIAN_POINT('Ctrl Pts',(-0.686185169594239,2.90023876414242,
11.0920828521819));
#47266=CARTESIAN_POINT('Ctrl Pts',(-0.784381279689713,2.90386721875651,
11.0867459208781));
#47267=CARTESIAN_POINT('Ctrl Pts',(-0.882483612659545,2.90822362826941,
11.0803382472665));
#47268=CARTESIAN_POINT('Ctrl Pts',(-1.37227578455157,2.92997372546261,11.0483468737689));
#47269=CARTESIAN_POINT('Ctrl Pts',(-1.85973068428807,2.96986769642306,10.989669217233));
#47270=CARTESIAN_POINT('Ctrl Pts',(-2.34120806414937,3.02589889861017,10.9047837983762));
#47271=CARTESIAN_POINT('Ctrl Pts',(-2.44684847556357,3.03819264178203,10.8861591839162));
#47272=CARTESIAN_POINT('Ctrl Pts',(-2.55220111103462,3.05126331203751,10.8662727383614));
#47273=CARTESIAN_POINT('Ctrl Pts',(-2.65722748483552,3.06508983926093,10.845129205313));
#47274=CARTESIAN_POINT('Ctrl Pts',(-2.75721742290147,3.07825332906549,10.8249995894508));
#47275=CARTESIAN_POINT('Ctrl Pts',(-2.85691164015495,3.09210192194813,10.8037305593992));
#47276=CARTESIAN_POINT('Ctrl Pts',(-2.9562817073028,3.10660749829929,10.7813293867526));
#47277=CARTESIAN_POINT('Ctrl Pts',(-3.42652729613442,3.17525174387923,10.6753210793812));
#47278=CARTESIAN_POINT('Ctrl Pts',(-3.88951476256729,3.25860776287227,10.5439630996004));
#47279=CARTESIAN_POINT('Ctrl Pts',(-4.3422241853442,3.35370329731909,10.3879967801771));
#47280=CARTESIAN_POINT('Ctrl Pts',(-4.36944131534789,3.35942049116041,10.3786200025392));
#47281=CARTESIAN_POINT('Ctrl Pts',(-4.39662129094512,3.36518012041666,10.3691542639388));
#47282=CARTESIAN_POINT('Ctrl Pts',(-4.42376345396193,3.37098154034238,10.3595997198319));
#47283=CARTESIAN_POINT('Ctrl Pts',(-4.8712542026576,3.46662910330382,10.2020746879022));
#47284=CARTESIAN_POINT('Ctrl Pts',(-5.30846866553962,3.57363557563167,10.0204148208704));
#47285=CARTESIAN_POINT('Ctrl Pts',(-5.73279070742533,3.68906129430703,9.81543899687841));
#47286=CARTESIAN_POINT('Ctrl Pts',(-5.843530256068,9.74782190829776,17.4349067435944));
#47287=CARTESIAN_POINT('Ctrl Pts',(-3.895686837379,8.92798468161957,17.8601636720695));
#47288=CARTESIAN_POINT('Ctrl Pts',(0.0001633689302756,8.10806558103108,
18.285510362917));
#47289=CARTESIAN_POINT('Ctrl Pts',(3.896013575239,8.92805344962997,17.8601279975215));
#47290=CARTESIAN_POINT('Ctrl Pts',(5.844020362859,9.74802820036948,17.434799738045));
#47291=CARTESIAN_POINT('Ctrl Pts',(-5.843530256068,8.93341759983096,17.0810053948035));
#47292=CARTESIAN_POINT('Ctrl Pts',(-3.895686837379,8.18554671757756,17.4915920160191));
#47293=CARTESIAN_POINT('Ctrl Pts',(0.0001633689302756,7.43613494371508,
17.9044826735906));
#47294=CARTESIAN_POINT('Ctrl Pts',(3.896013575239,8.18560957201543,17.4915573861792));
#47295=CARTESIAN_POINT('Ctrl Pts',(5.844020362859,8.93360578330469,17.0809020807058));
#47296=CARTESIAN_POINT('Ctrl Pts',(-5.843530256068,7.38850508713007,16.1560629905898));
#47297=CARTESIAN_POINT('Ctrl Pts',(-3.895686837379,6.77499149589132,16.5818456722199));
#47298=CARTESIAN_POINT('Ctrl Pts',(0.0001633689302756,6.16225640317841,
17.0065480575296));
#47299=CARTESIAN_POINT('Ctrl Pts',(3.896013575239,6.77504288702132,16.5818100517117));
#47300=CARTESIAN_POINT('Ctrl Pts',(5.844020362859,7.38865946288593,16.1559558527372));
#47301=CARTESIAN_POINT('Ctrl Pts',(-5.843530256068,5.5035950496088,14.2139340091217));
#47302=CARTESIAN_POINT('Ctrl Pts',(-3.895686837379,5.02273055192306,14.7660279927807));
#47303=CARTESIAN_POINT('Ctrl Pts',(0.0001633689302756,4.54131578037147,
15.3185227509534));
#47304=CARTESIAN_POINT('Ctrl Pts',(3.896013575239,5.02277092898996,14.7659816541094));
#47305=CARTESIAN_POINT('Ctrl Pts',(5.844020362859,5.50371604744243,14.2137950881263));
#47306=CARTESIAN_POINT('Ctrl Pts',(-5.843530256068,4.23580635710636,11.9384138467925));
#47307=CARTESIAN_POINT('Ctrl Pts',(-3.895686837379,3.77920659141981,12.6803367266932));
#47308=CARTESIAN_POINT('Ctrl Pts',(0.0001633689302756,3.32382395062254,
13.4219156363165));
#47309=CARTESIAN_POINT('Ctrl Pts',(3.896013575239,3.77924478513343,12.6802745292127));
#47310=CARTESIAN_POINT('Ctrl Pts',(5.844020362859,4.23592124932683,11.9382271599712));
#47311=CARTESIAN_POINT('Ctrl Pts',(-5.843530256068,3.79656748423947,10.3003457878546));
#47312=CARTESIAN_POINT('Ctrl Pts',(-3.895686837379,3.28180496518032,11.180104908631));
#47313=CARTESIAN_POINT('Ctrl Pts',(0.0001633689302756,2.76478687832676,
12.0604698112373));
#47314=CARTESIAN_POINT('Ctrl Pts',(3.896013575239,3.28184832836377,11.1800310709341));
#47315=CARTESIAN_POINT('Ctrl Pts',(5.844020362859,3.79669701166332,10.3001244179095));
#47316=CARTESIAN_POINT('Ctrl Pts',(-5.843530256068,3.68097897297366,9.52158538067259));
#47317=CARTESIAN_POINT('Ctrl Pts',(-3.895686837379,3.1209714929087,10.4634399073288));
#47318=CARTESIAN_POINT('Ctrl Pts',(0.0001633689302756,2.56014667279914,
11.4055373579833));
#47319=CARTESIAN_POINT('Ctrl Pts',(3.896013575239,3.12101853023684,10.4633608920186));
#47320=CARTESIAN_POINT('Ctrl Pts',(5.844020362859,3.68111988520519,9.52134838592816));
#47321=CARTESIAN_POINT('',(-5.73644346265606,9.52121765609472,17.3763289909641));
#47322=CARTESIAN_POINT('Ctrl Pts',(-5.7364438776242,9.52121721553873,17.3763301032173));
#47323=CARTESIAN_POINT('Ctrl Pts',(-5.68283410133726,9.49933861028788,17.3876652899307));
#47324=CARTESIAN_POINT('Ctrl Pts',(-5.62362602122325,9.47550628802813,17.4000397186838));
#47325=CARTESIAN_POINT('Ctrl Pts',(-5.55871833523674,9.44988973305887,17.413361706295));
#47326=CARTESIAN_POINT('Ctrl Pts',(-5.49483785882197,9.42467857800582,17.4264728641257));
#47327=CARTESIAN_POINT('Ctrl Pts',(-5.42543674955886,9.39773917888359,17.4405018460537));
#47328=CARTESIAN_POINT('Ctrl Pts',(-5.35041843921672,9.36927739071634,17.4553379787743));
#47329=CARTESIAN_POINT('Ctrl Pts',(-5.28279634620865,9.34362171175151,17.4687113851085));
#47330=CARTESIAN_POINT('Ctrl Pts',(-5.21061007458706,9.31672951463994,17.4827403793437));
#47331=CARTESIAN_POINT('Ctrl Pts',(-5.13378889523013,9.28878373746725,17.497327002931));
#47332=CARTESIAN_POINT('Ctrl Pts',(-5.05114656189602,9.25872035843925,17.5130189334483));
#47333=CARTESIAN_POINT('Ctrl Pts',(-4.96313255951284,9.22743587270336,17.529358901209));
#47334=CARTESIAN_POINT('Ctrl Pts',(-4.86963668391357,9.19519757921132,17.5462092461735));
#47335=CARTESIAN_POINT('Ctrl Pts',(-4.82248599479802,9.17893955986752,17.5547070047305));
#47336=CARTESIAN_POINT('Ctrl Pts',(-4.77394112144133,9.16243967649653,17.5633341890093));
#47337=CARTESIAN_POINT('Ctrl Pts',(-4.72398792920224,9.14573668509423,17.5720707845653));
#47338=CARTESIAN_POINT('Ctrl Pts',(-4.64948483055452,9.12082487144674,17.585101051729));
#47339=CARTESIAN_POINT('Ctrl Pts',(-4.57184842120784,9.09546050181848,17.5983752821524));
#47340=CARTESIAN_POINT('Ctrl Pts',(-4.49102962369258,9.06978519776136,17.6118209922886));
#47341=CARTESIAN_POINT('Ctrl Pts',(-4.45062022493494,9.05694754573281,17.6185438473567));
#47342=CARTESIAN_POINT('Ctrl Pts',(-4.40941525324104,9.04403240896086,17.6253094358827));
#47343=CARTESIAN_POINT('Ctrl Pts',(-4.36740858903266,9.03105903615374,17.6321079195241));
#47344=CARTESIAN_POINT('Ctrl Pts',(-4.34640525692848,9.02457234975017,17.6355071613449));
#47345=CARTESIAN_POINT('Ctrl Pts',(-4.32520149790406,9.0180711103512,17.6389146148433));
#47346=CARTESIAN_POINT('Ctrl Pts',(-4.3037965478717,9.01155783669579,17.6423290072939));
#47347=CARTESIAN_POINT('Ctrl Pts',(-4.29309407285551,9.00830119986808,17.6440362035192));
#47348=CARTESIAN_POINT('Ctrl Pts',(-4.2823412998427,9.00504155485615,17.645745133715));
#47349=CARTESIAN_POINT('Ctrl Pts',(-4.27153813267531,9.00177922108494,17.6474556350356));
#47350=CARTESIAN_POINT('Ctrl Pts',(-4.26343575729977,8.99933247075653,17.648738511026));
#47351=CARTESIAN_POINT('Ctrl Pts',(-4.25530503519258,8.99688420803268,17.6500222707106));
#47352=CARTESIAN_POINT('Ctrl Pts',(-4.24714592572875,8.99443456916128,17.6513068446019));
#47353=CARTESIAN_POINT('Ctrl Pts',(-4.24442622257414,8.99361802287081,17.6517350358991));
#47354=CARTESIAN_POINT('Ctrl Pts',(-4.24040661896544,8.99241275500541,17.6523670902657));
#47355=CARTESIAN_POINT('Ctrl Pts',(-4.23897735232055,8.99198447672772,17.652591687306));
#47356=CARTESIAN_POINT('Ctrl Pts',(-4.15849608766392,8.96786834868632,17.665238630342));
#47357=CARTESIAN_POINT('Ctrl Pts',(-4.07249650548149,8.94277842041226,17.6783932118544));
#47358=CARTESIAN_POINT('Ctrl Pts',(-3.98088600231545,8.91699602800316,17.6919117243921));
#47359=CARTESIAN_POINT('Ctrl Pts',(-3.89040600132535,8.89153179835609,17.7052634142697));
#47360=CARTESIAN_POINT('Ctrl Pts',(-3.79445270593128,8.86539204381246,17.7189701335298));
#47361=CARTESIAN_POINT('Ctrl Pts',(-3.69293689881025,8.83889286121126,17.7328696811413));
#47362=CARTESIAN_POINT('Ctrl Pts',(-3.66359282295988,8.83123302924741,17.7368874729607));
#47363=CARTESIAN_POINT('Ctrl Pts',(-3.63378397028016,8.8235434582015,17.7409212220854));
#47364=CARTESIAN_POINT('Ctrl Pts',(-3.60350818595862,8.81583250498245,17.744966629995));
#47365=CARTESIAN_POINT('Ctrl Pts',(-3.49990877451926,8.78944672396864,17.7588094382941));
#47366=CARTESIAN_POINT('Ctrl Pts',(-3.39084132813128,8.76280714218299,17.7727908127734));
#47367=CARTESIAN_POINT('Ctrl Pts',(-3.27622403179247,8.73628098812355,17.7867233140545));
#47368=CARTESIAN_POINT('Ctrl Pts',(-3.25749145032406,8.7319456621489,17.7890003849997));
#47369=CARTESIAN_POINT('Ctrl Pts',(-3.23861062517755,8.72761346586328,17.7912760977316));
#47370=CARTESIAN_POINT('Ctrl Pts',(-3.21958119918262,8.7232861203216,17.7935495717162));
#47371=CARTESIAN_POINT('Ctrl Pts',(-3.15184970057834,8.7078837850859,17.801641555156));
#47372=CARTESIAN_POINT('Ctrl Pts',(-3.08223598429778,8.69254251698729,17.8097053219785));
#47373=CARTESIAN_POINT('Ctrl Pts',(-3.01072583053028,8.67734391900242,17.8176992250224));
#47374=CARTESIAN_POINT('Ctrl Pts',(-2.96889170568906,8.66845259361696,17.8223757348645));
#47375=CARTESIAN_POINT('Ctrl Pts',(-2.92568006515535,8.65945929280977,17.8271077760883));
#47376=CARTESIAN_POINT('Ctrl Pts',(-2.88236683521321,8.6506496230998,17.8317452466546));
#47377=CARTESIAN_POINT('Ctrl Pts',(-2.85164156799341,8.64440027489098,17.8350349464198));
#47378=CARTESIAN_POINT('Ctrl Pts',(-2.82086517985766,8.63824239100087,17.8382775516242));
#47379=CARTESIAN_POINT('Ctrl Pts',(-2.79049313147201,8.63226377058535,17.8414269193232));
#47380=CARTESIAN_POINT('Ctrl Pts',(-2.49774374027982,8.5746371836463,17.8717829712043));
#47381=CARTESIAN_POINT('Ctrl Pts',(-2.21879412928721,8.52884151832713,17.8959619875009));
#47382=CARTESIAN_POINT('Ctrl Pts',(-1.95462250685991,8.49248912601094,17.9151940729285));
#47383=CARTESIAN_POINT('Ctrl Pts',(-1.73091164750199,8.46170449876731,17.9314805548706));
#47384=CARTESIAN_POINT('Ctrl Pts',(-1.51779862260439,8.43769072216954,17.9442201273955));
#47385=CARTESIAN_POINT('Ctrl Pts',(-1.3158774973236,8.41902980884336,17.9541436669417));
#47386=CARTESIAN_POINT('Ctrl Pts',(-1.27935766618023,8.41565476127117,17.9559384568037));
#47387=CARTESIAN_POINT('Ctrl Pts',(-1.24320393342112,8.41245493284762,17.9576410685465));
#47388=CARTESIAN_POINT('Ctrl Pts',(-1.20741981363967,8.40942211174052,17.9592557342648));
#47389=CARTESIAN_POINT('Ctrl Pts',(-1.05114003191732,8.39617688945994,17.9663074546243));
#47390=CARTESIAN_POINT('Ctrl Pts',(-0.901869672502831,8.38610981159634,
17.9716853664282));
#47391=CARTESIAN_POINT('Ctrl Pts',(-0.759755495368958,8.37855170967793,
17.9757326033567));
#47392=CARTESIAN_POINT('Ctrl Pts',(-0.689409738587004,8.37481048969545,
17.9777359639669));
#47393=CARTESIAN_POINT('Ctrl Pts',(-0.620817387436509,8.37168470694852,
17.9794129221181));
#47394=CARTESIAN_POINT('Ctrl Pts',(-0.553996241471728,8.36909742699286,
17.9808028777138));
#47395=CARTESIAN_POINT('Ctrl Pts',(-0.453088831378307,8.36519034465025,
17.9829018662492));
#47396=CARTESIAN_POINT('Ctrl Pts',(-0.356216007876087,8.36251015480873,
17.9843469301776));
#47397=CARTESIAN_POINT('Ctrl Pts',(-0.263414058300233,8.36080599351406,
17.9852672871028));
#47398=CARTESIAN_POINT('Ctrl Pts',(-0.217013083512306,8.35995391286673,
17.9857274655654));
#47399=CARTESIAN_POINT('Ctrl Pts',(-0.171629597781392,8.3593461703712,17.9860563598658));
#47400=CARTESIAN_POINT('Ctrl Pts',(-0.127266766540642,8.35895266383208,
17.9862689842807));
#47401=CARTESIAN_POINT('Ctrl Pts',(-0.105085350920267,8.35875591056252,
17.9863752964882));
#47402=CARTESIAN_POINT('Ctrl Pts',(-0.0831590989529071,8.35861272470365,
17.9864525259354));
#47403=CARTESIAN_POINT('Ctrl Pts',(-0.0614883185709054,8.358519476498,17.9865025015845));
#47404=CARTESIAN_POINT('Ctrl Pts',(-0.040712076886637,8.35843007744438,
17.9865504143105));
#47405=CARTESIAN_POINT('Ctrl Pts',(-0.0212663475724724,8.35838682250874,
17.9865732018906));
#47406=CARTESIAN_POINT('Ctrl Pts',(1.636912875435E-12,8.35838583196835,
17.9865726564898));
#47407=CARTESIAN_POINT('Ctrl Pts',(0.000915640623919675,8.3583857893198,
17.9865726330071));
#47408=CARTESIAN_POINT('Ctrl Pts',(0.00183465631929605,8.3583858335768,
17.98657256177));
#47409=CARTESIAN_POINT('Ctrl Pts',(0.00275729860215538,8.35838596679082,
17.9865724416797));
#47410=CARTESIAN_POINT('Ctrl Pts',(0.129186119377432,8.35840422098474,17.9865559858236));
#47411=CARTESIAN_POINT('Ctrl Pts',(0.262648467165869,8.36008917059176,17.9856368970372));
#47412=CARTESIAN_POINT('Ctrl Pts',(0.403015392074524,8.3640381883428,17.9835101130247));
#47413=CARTESIAN_POINT('Ctrl Pts',(0.546996654915845,8.36808889019544,17.9813285659963));
#47414=CARTESIAN_POINT('Ctrl Pts',(0.698242647626174,8.37452182263524,17.9778762910046));
#47415=CARTESIAN_POINT('Ctrl Pts',(0.856614200546237,8.3840309130267,17.9727981879443));
#47416=CARTESIAN_POINT('Ctrl Pts',(0.980582325233258,8.39147432114877,17.9688232132614));
#47417=CARTESIAN_POINT('Ctrl Pts',(1.10891645992642,8.40080359578708,17.963851511902));
#47418=CARTESIAN_POINT('Ctrl Pts',(1.24154985587638,8.41237122005545,17.9577024643033));
#47419=CARTESIAN_POINT('Ctrl Pts',(1.46301935575659,8.43168668689672,17.9474348655085));
#47420=CARTESIAN_POINT('Ctrl Pts',(1.69642619692483,8.45723519738743,17.933885327057));
#47421=CARTESIAN_POINT('Ctrl Pts',(1.9411391977435,8.49068447227641,17.916196228235));
#47422=CARTESIAN_POINT('Ctrl Pts',(1.95457768306835,8.49252134889604,17.9152248262493));
#47423=CARTESIAN_POINT('Ctrl Pts',(1.96805026425494,8.49438206284401,17.9142409349655));
#47424=CARTESIAN_POINT('Ctrl Pts',(1.98155683677488,8.49626689386396,17.9132444105436));
#47425=CARTESIAN_POINT('Ctrl Pts',(2.11128655275263,8.51437056839158,17.9036728608387));
#47426=CARTESIAN_POINT('Ctrl Pts',(2.2441485498313,8.53469810982091,17.8929357036826));
#47427=CARTESIAN_POINT('Ctrl Pts',(2.38002393604269,8.55749304688889,17.8809078074937));
#47428=CARTESIAN_POINT('Ctrl Pts',(2.44796162914838,8.56889051542288,17.8748938593993));
#47429=CARTESIAN_POINT('Ctrl Pts',(2.51665241842725,8.5809047741614,17.8685572531071));
#47430=CARTESIAN_POINT('Ctrl Pts',(2.58608015528761,8.59356557582336,17.86188244989));
#47431=CARTESIAN_POINT('Ctrl Pts',(2.6207940237178,8.59989597665434,17.8585450482815));
#47432=CARTESIAN_POINT('Ctrl Pts',(2.65569212925892,8.60638801177433,17.8551231000482));
#47433=CARTESIAN_POINT('Ctrl Pts',(2.69077230290425,8.61304536776699,17.8516147019052));
#47434=CARTESIAN_POINT('Ctrl Pts',(2.70831238972691,8.61637404576332,17.8498605028337));
#47435=CARTESIAN_POINT('Ctrl Pts',(2.72589799362908,8.61974405384018,17.848084691545));
#47436=CARTESIAN_POINT('Ctrl Pts',(2.74352883870858,8.6231558510227,17.846287032341));
#47437=CARTESIAN_POINT('Ctrl Pts',(2.75878964495409,8.62610901495311,17.8447310247484));
#47438=CARTESIAN_POINT('Ctrl Pts',(2.77549105180195,8.6293697107186,17.8430131339223));
#47439=CARTESIAN_POINT('Ctrl Pts',(2.78998005552623,8.63222120238673,17.8415109419287));
#47440=CARTESIAN_POINT('Ctrl Pts',(2.79223023162701,8.63266404569917,17.8412776480055));
#47441=CARTESIAN_POINT('Ctrl Pts',(2.79442704718602,8.63309692748931,17.8410496048427));
#47442=CARTESIAN_POINT('Ctrl Pts',(2.79655681911697,8.63351706784238,17.8408282768086));
#47443=CARTESIAN_POINT('Ctrl Pts',(3.06216252883609,8.68591313665962,17.813226265189));
#47444=CARTESIAN_POINT('Ctrl Pts',(3.32574192769713,8.74545004698172,17.7819422058441));
#47445=CARTESIAN_POINT('Ctrl Pts',(3.58705296384314,8.81170933478502,17.7471902317705));
#47446=CARTESIAN_POINT('Ctrl Pts',(3.85046129536175,8.87850042292769,17.7121593366245));
#47447=CARTESIAN_POINT('Ctrl Pts',(4.1115647060592,8.95212217125134,17.6736046824906));
#47448=CARTESIAN_POINT('Ctrl Pts',(4.37011526901556,9.03209869294817,17.6317706874632));
#47449=CARTESIAN_POINT('Ctrl Pts',(4.63268827870015,9.11331946371704,17.5892858525593));
#47450=CARTESIAN_POINT('Ctrl Pts',(4.89262838997619,9.20109425021854,17.5434188750952));
#47451=CARTESIAN_POINT('Ctrl Pts',(5.14967592346197,9.29487661277545,17.4944509967036));
#47452=CARTESIAN_POINT('Ctrl Pts',(5.3470087682887,9.36687240338649,17.4568588415987));
#47453=CARTESIAN_POINT('Ctrl Pts',(5.54263687795273,9.44240774729819,17.4174397040541));
#47454=CARTESIAN_POINT('Ctrl Pts',(5.73644276397646,9.52121697613148,17.3763304378294));
#47455=CARTESIAN_POINT('Ctrl Pts',(-5.73644356954166,9.52121823625822,17.3763277345534));
#47456=CARTESIAN_POINT('Ctrl Pts',(-5.73766037024742,8.76684683000269,17.0280907334631));
#47457=CARTESIAN_POINT('Ctrl Pts',(-5.73849618482897,8.0551635985718,16.5887330587425));
#47458=CARTESIAN_POINT('Ctrl Pts',(-5.73940756701334,6.75884967989494,15.5535369773042));
#47459=CARTESIAN_POINT('Ctrl Pts',(-5.73948313454875,6.1741609243319,14.9577815461622));
#47460=CARTESIAN_POINT('Ctrl Pts',(-5.73887402246562,5.16463991420442,13.6459927306558));
#47461=CARTESIAN_POINT('Ctrl Pts',(-5.73818934284707,4.74008688875323,12.9297575973714));
#47462=CARTESIAN_POINT('Ctrl Pts',(-5.73605973645603,4.07387565941445,11.4195453010467));
#47463=CARTESIAN_POINT('Ctrl Pts',(-5.73461480968354,3.83284551922558,10.6253394017529));
#47464=CARTESIAN_POINT('Ctrl Pts',(-5.732787930129,3.6890690658187,9.81543762359093));
#47465=CARTESIAN_POINT('Ctrl Pts',(-5.69266556774236,9.93047362171998,17.3532063511374));
#47466=CARTESIAN_POINT('Ctrl Pts',(-5.6579015041144,9.91591389121002,17.3608578763875));
#47467=CARTESIAN_POINT('Ctrl Pts',(-5.54372918028431,9.86855194591315,17.3857823389823));
#47468=CARTESIAN_POINT('Ctrl Pts',(-5.34117686668635,9.78714465878113,17.4287935841603));
#47469=CARTESIAN_POINT('Ctrl Pts',(-5.07577939191893,9.68537211231267,17.4827627766661));
#47470=CARTESIAN_POINT('Ctrl Pts',(-4.78282515662344,9.57897707244638,17.5393277358742));
#47471=CARTESIAN_POINT('Ctrl Pts',(-4.45930905771319,9.46872628426622,17.5980540214943));
#47472=CARTESIAN_POINT('Ctrl Pts',(-4.10061553946611,9.35538603621517,17.6585190484757));
#47473=CARTESIAN_POINT('Ctrl Pts',(-3.70134298965158,9.240249772823,17.7200282654163));
#47474=CARTESIAN_POINT('Ctrl Pts',(-3.25666212546635,9.12573356196013,17.7812939172411));
#47475=CARTESIAN_POINT('Ctrl Pts',(-2.76257283843288,9.01548172265967,17.8403746545893));
#47476=CARTESIAN_POINT('Ctrl Pts',(-2.21448293063478,8.91409697651722,17.8948143734171));
#47477=CARTESIAN_POINT('Ctrl Pts',(-1.60537183769643,8.82721888555496,17.9415936924642));
#47478=CARTESIAN_POINT('Ctrl Pts',(-0.938804294879647,8.76361682732247,
17.9759748015788));
#47479=CARTESIAN_POINT('Ctrl Pts',(-0.236508776851559,8.73273231277665,
17.9927966994848));
#47480=CARTESIAN_POINT('Ctrl Pts',(0.464364601057791,8.7390534224892,17.9893367439343));
#47481=CARTESIAN_POINT('Ctrl Pts',(1.12896559560388,8.77908287968296,17.9676008051861));
#47482=CARTESIAN_POINT('Ctrl Pts',(1.73422006975932,8.84413599471573,17.9324762362283));
#47483=CARTESIAN_POINT('Ctrl Pts',(2.27384587622857,8.92486790916139,17.8890293045475));
#47484=CARTESIAN_POINT('Ctrl Pts',(2.75210517025956,9.01417457107673,17.8410806225033));
#47485=CARTESIAN_POINT('Ctrl Pts',(3.17956446862062,9.10813528834538,17.790722121323));
#47486=CARTESIAN_POINT('Ctrl Pts',(3.56234892002592,9.2036241030006,17.7396175800791));
#47487=CARTESIAN_POINT('Ctrl Pts',(3.90388903432242,9.29788224441845,17.6892335714503));
#47488=CARTESIAN_POINT('Ctrl Pts',(4.20698277150655,9.38866585517398,17.6407615423958));
#47489=CARTESIAN_POINT('Ctrl Pts',(4.47552350916443,9.47468692044263,17.5948833416307));
#47490=CARTESIAN_POINT('Ctrl Pts',(4.71437364865999,9.55559720416526,17.5517812500452));
#47491=CARTESIAN_POINT('Ctrl Pts',(4.92834373472514,9.63159157290231,17.5113505406579));
#47492=CARTESIAN_POINT('Ctrl Pts',(5.12117579191109,9.70292314754304,17.473458081615));
#47493=CARTESIAN_POINT('Ctrl Pts',(5.29544459285597,9.7697118950186,17.4380436592871));
#47494=CARTESIAN_POINT('Ctrl Pts',(5.45302136069345,9.83200747379042,17.4050853286124));
#47495=CARTESIAN_POINT('Ctrl Pts',(5.58355472894296,9.88505281103088,17.3770970955391));
#47496=CARTESIAN_POINT('Ctrl Pts',(5.66171727448349,9.91751314502851,17.3600175469933));
#47497=CARTESIAN_POINT('Ctrl Pts',(5.69263920831806,9.93046917053698,17.3532089777586));
#47498=CARTESIAN_POINT('Ctrl Pts',(-5.75649916779056,9.81444719502755,17.4266144013715));
#47499=CARTESIAN_POINT('Ctrl Pts',(-5.7214030273039,9.79970756314098,17.4342702770646));
#47500=CARTESIAN_POINT('Ctrl Pts',(-5.60614021198355,9.751757100279,17.4592032236821));
#47501=CARTESIAN_POINT('Ctrl Pts',(-5.40164894963342,9.66931649258382,17.5021948859192));
#47502=CARTESIAN_POINT('Ctrl Pts',(-5.13368112666671,9.5661995361647,17.5560703775035));
#47503=CARTESIAN_POINT('Ctrl Pts',(-4.83783506996195,9.45834443418207,17.612479415478));
#47504=CARTESIAN_POINT('Ctrl Pts',(-4.51104954847754,9.34652609944795,17.6709960258764));
#47505=CARTESIAN_POINT('Ctrl Pts',(-4.14863414602988,9.23151944235374,17.7312040879216));
#47506=CARTESIAN_POINT('Ctrl Pts',(-3.7450998233873,9.11463384419983,17.7924131442713));
#47507=CARTESIAN_POINT('Ctrl Pts',(-3.29553136104131,8.99831906675384,17.8533393247946));
#47508=CARTESIAN_POINT('Ctrl Pts',(-2.79585032997637,8.88627539459825,17.9120464571609));
#47509=CARTESIAN_POINT('Ctrl Pts',(-2.2413830036986,8.78318279794773,17.9660866201541));
#47510=CARTESIAN_POINT('Ctrl Pts',(-1.62500802087657,8.69478332220193,18.0124555046676));
#47511=CARTESIAN_POINT('Ctrl Pts',(-0.950336100124751,8.63001825070586,
18.046463119548));
#47512=CARTESIAN_POINT('Ctrl Pts',(-0.239411452652046,8.59853301614872,
18.0630351699963));
#47513=CARTESIAN_POINT('Ctrl Pts',(0.470068367886107,8.60498147064549,18.0596354408429));
#47514=CARTESIAN_POINT('Ctrl Pts',(1.14282032180368,8.64577151992081,18.0381873663481));
#47515=CARTESIAN_POINT('Ctrl Pts',(1.75540154176908,8.71200012569824,18.0034225013884));
#47516=CARTESIAN_POINT('Ctrl Pts',(2.30143868154968,8.79413603665911,17.9603447467543));
#47517=CARTESIAN_POINT('Ctrl Pts',(2.78525552176593,8.884943982301,17.9127452134487));
#47518=CARTESIAN_POINT('Ctrl Pts',(3.21756459439386,8.98043601974661,17.8627089971835));
#47519=CARTESIAN_POINT('Ctrl Pts',(3.60458630020787,9.07743638428598,17.8118963803323));
#47520=CARTESIAN_POINT('Ctrl Pts',(3.94981603920815,9.17314581293368,17.761771322737));
#47521=CARTESIAN_POINT('Ctrl Pts',(4.25610869089316,9.26529062369714,17.7135235168905));
#47522=CARTESIAN_POINT('Ctrl Pts',(4.52742310264509,9.35256886962024,17.6678347552335));
#47523=CARTESIAN_POINT('Ctrl Pts',(4.76869242281635,9.43463232895327,17.6248884916112));
#47524=CARTESIAN_POINT('Ctrl Pts',(4.98479244422413,9.51168301727899,17.5845813156777));
#47525=CARTESIAN_POINT('Ctrl Pts',(5.17951571606055,9.58398125229581,17.5467807593111));
#47526=CARTESIAN_POINT('Ctrl Pts',(5.35547336783225,9.65165209884505,17.5114269323108));
#47527=CARTESIAN_POINT('Ctrl Pts',(5.51456429154051,9.714749875375,17.4784991695837));
#47528=CARTESIAN_POINT('Ctrl Pts',(5.64634618110254,9.76846300224162,17.4505149960062));
#47529=CARTESIAN_POINT('Ctrl Pts',(5.72525518795606,9.80132673659468,17.4334297817267));
#47530=CARTESIAN_POINT('Ctrl Pts',(5.75647210570228,9.81444369343647,17.4266190648295));
#47531=CARTESIAN_POINT('Ctrl Pts',(-5.8136196818267,9.67439307521046,17.423196759913));
#47532=CARTESIAN_POINT('Ctrl Pts',(-5.77819705101768,9.65952057934147,17.4308417919519));
#47533=CARTESIAN_POINT('Ctrl Pts',(-5.66186629691354,9.61113998799483,17.4557318756997));
#47534=CARTESIAN_POINT('Ctrl Pts',(-5.45549726793896,9.5279688855426,17.49860525688));
#47535=CARTESIAN_POINT('Ctrl Pts',(-5.18506580571852,9.42394225964876,17.5522463207665));
#47536=CARTESIAN_POINT('Ctrl Pts',(-4.8864742352847,9.31513196562998,17.60833774815));
#47537=CARTESIAN_POINT('Ctrl Pts',(-4.55661570512959,9.20231551898028,17.6664644876122));
#47538=CARTESIAN_POINT('Ctrl Pts',(-4.19074002650286,9.08627222891287,17.7262188124506));
#47539=CARTESIAN_POINT('Ctrl Pts',(-3.78329010947872,8.96832213491303,17.7869166097969));
#47540=CARTESIAN_POINT('Ctrl Pts',(-3.3292874134522,8.85093759828555,17.8472819386104));
#47541=CARTESIAN_POINT('Ctrl Pts',(-2.82459972125377,8.73785509947674,17.9053904110669));
#47542=CARTESIAN_POINT('Ctrl Pts',(-2.26449815904256,8.63380219603441,17.9588116307512));
#47543=CARTESIAN_POINT('Ctrl Pts',(-1.641790113482,8.54458023606658,18.0045692580133));
#47544=CARTESIAN_POINT('Ctrl Pts',(-0.960140287992341,8.47921865788041,
18.0380445444115));
#47545=CARTESIAN_POINT('Ctrl Pts',(-0.241865765967301,8.44745231309993,
18.0542799882141));
#47546=CARTESIAN_POINT('Ctrl Pts',(0.47489962410608,8.45395708095796,18.0509594735994));
#47547=CARTESIAN_POINT('Ctrl Pts',(1.15461838952617,8.49511618875115,18.0299067692742));
#47548=CARTESIAN_POINT('Ctrl Pts',(1.77352632071982,8.56195700003843,17.9956606052727));
#47549=CARTESIAN_POINT('Ctrl Pts',(2.32516508944598,8.64485754784285,17.9531364356432));
#47550=CARTESIAN_POINT('Ctrl Pts',(2.81389481841379,8.7365111091626,17.9060786654344));
#47551=CARTESIAN_POINT('Ctrl Pts',(3.25054101924557,8.8328888560205,17.856557408933));
#47552=CARTESIAN_POINT('Ctrl Pts',(3.64139477649633,8.93078312520244,17.8062236353288));
#47553=CARTESIAN_POINT('Ctrl Pts',(3.98999701973634,9.02736771692221,17.7565340796509));
#47554=CARTESIAN_POINT('Ctrl Pts',(4.29924266837349,9.12034820868826,17.70867337501));
#47555=CARTESIAN_POINT('Ctrl Pts',(4.57314066591343,9.20841173545414,17.6633218271144));
#47556=CARTESIAN_POINT('Ctrl Pts',(4.81668173982086,9.29120827097723,17.6206641928624));
#47557=CARTESIAN_POINT('Ctrl Pts',(5.03479661627034,9.36894315808525,17.5805992095702));
#47558=CARTESIAN_POINT('Ctrl Pts',(5.23132099554413,9.44188068092139,17.542995771987));
#47559=CARTESIAN_POINT('Ctrl Pts',(5.40889737384632,9.51014887211331,17.5077946817537));
#47560=CARTESIAN_POINT('Ctrl Pts',(5.56944911388493,9.57380459823179,17.4749769061113));
#47561=CARTESIAN_POINT('Ctrl Pts',(5.70244460066286,9.62799566795384,17.4470585904865));
#47562=CARTESIAN_POINT('Ctrl Pts',(5.78208503328795,9.66115432803744,17.4300028520173));
#47563=CARTESIAN_POINT('Ctrl Pts',(5.81359216861889,9.6743893639485,17.4232038071368));
#47564=CARTESIAN_POINT('Ctrl Pts',(-5.8478684852305,9.55010345183306,17.3442497677672));
#47565=CARTESIAN_POINT('Ctrl Pts',(-5.8122174502477,9.53518258073926,17.3518718998449));
#47566=CARTESIAN_POINT('Ctrl Pts',(-5.6951438548994,9.48665146739425,17.3766801397573));
#47567=CARTESIAN_POINT('Ctrl Pts',(-5.48749011694532,9.40325841727438,17.4193704823528));
#47568=CARTESIAN_POINT('Ctrl Pts',(-5.21539943495581,9.29901279673593,17.4727034262668));
#47569=CARTESIAN_POINT('Ctrl Pts',(-4.91498607989269,9.19002071642843,17.528406250694));
#47570=CARTESIAN_POINT('Ctrl Pts',(-4.58312097072923,9.07705601563583,17.586074177172));
#47571=CARTESIAN_POINT('Ctrl Pts',(-4.21502610849078,8.96089695073282,17.6453074158685));
#47572=CARTESIAN_POINT('Ctrl Pts',(-3.80511493093653,8.8428659429201,17.705428641255));
#47573=CARTESIAN_POINT('Ctrl Pts',(-3.34838603991078,8.72544050156519,17.765171621273));
#47574=CARTESIAN_POINT('Ctrl Pts',(-2.84069310071325,8.61236336019298,17.8226269922694));
#47575=CARTESIAN_POINT('Ctrl Pts',(-2.27729398891054,8.50836664329447,17.8753862184402));
#47576=CARTESIAN_POINT('Ctrl Pts',(-1.65097445000958,8.4192511995751,17.9205058456566));
#47577=CARTESIAN_POINT('Ctrl Pts',(-0.965445840894169,8.35402624679165,
17.95344150259));
#47578=CARTESIAN_POINT('Ctrl Pts',(-0.243178106984612,8.32237670105204,
17.9693493410763));
#47579=CARTESIAN_POINT('Ctrl Pts',(0.477492972615759,8.32885109541683,17.9661044996576));
#47580=CARTESIAN_POINT('Ctrl Pts',(1.16102514354678,8.36988481208941,17.9454421695092));
#47581=CARTESIAN_POINT('Ctrl Pts',(1.78347110439172,8.43660345553906,17.9117260313382));
#47582=CARTESIAN_POINT('Ctrl Pts',(2.33831781818648,8.51941531978428,17.8697821884199));
#47583=CARTESIAN_POINT('Ctrl Pts',(2.82992627541635,8.61102198917264,17.8233044445839));
#47584=CARTESIAN_POINT('Ctrl Pts',(3.26917005567782,8.70739159011194,17.7743440670996));
#47585=CARTESIAN_POINT('Ctrl Pts',(3.66236643292317,8.80531143237798,17.7245395595451));
#47586=CARTESIAN_POINT('Ctrl Pts',(4.01306968578505,8.90194951063851,17.6753378872775));
#47587=CARTESIAN_POINT('Ctrl Pts',(4.32418661918743,8.99500558484918,17.6279167669807));
#47588=CARTESIAN_POINT('Ctrl Pts',(4.59974676804594,9.08316196710642,17.5829540145801));
#47589=CARTESIAN_POINT('Ctrl Pts',(4.8447690100173,9.16606552695142,17.5406354503353));
#47590=CARTESIAN_POINT('Ctrl Pts',(5.06421316646418,9.2439201861955,17.500862178041));
#47591=CARTESIAN_POINT('Ctrl Pts',(5.26193851816834,9.31698985470052,17.4635047652742));
#47592=CARTESIAN_POINT('Ctrl Pts',(5.44060507020823,9.38540257085393,17.4285048762992));
#47593=CARTESIAN_POINT('Ctrl Pts',(5.60215053677798,9.44921492438462,17.3958449989642));
#47594=CARTESIAN_POINT('Ctrl Pts',(5.73598092677608,9.50355945699389,17.3680354126988));
#47595=CARTESIAN_POINT('Ctrl Pts',(5.81613053647907,9.53682145263586,17.3510357885404));
#47596=CARTESIAN_POINT('Ctrl Pts',(5.84784089921826,9.55009843600966,17.3442588686793));
#47597=CARTESIAN_POINT('',(-5.593361696257,9.87744143006053,17.3818877156668));
#47598=CARTESIAN_POINT('Ctrl Pts',(-5.593361696257,9.87744143006053,17.3818877156668));
#47599=CARTESIAN_POINT('Ctrl Pts',(-5.53989250492938,9.85546719473476,17.3934537221547));
#47600=CARTESIAN_POINT('Ctrl Pts',(-5.47940098467193,9.83101975551148,17.4063389204174));
#47601=CARTESIAN_POINT('Ctrl Pts',(-5.37813021089118,9.79076334881011,17.4276019464024));
#47602=CARTESIAN_POINT('Ctrl Pts',(-5.34261770406517,9.77675424696755,17.4350079149863));
#47603=CARTESIAN_POINT('Ctrl Pts',(-5.28671557047751,9.75493420233089,17.4465521226116));
#47604=CARTESIAN_POINT('Ctrl Pts',(-5.25810616034651,9.74382322934089,17.4524326696608));
#47605=CARTESIAN_POINT('Ctrl Pts',(-5.22850923520978,9.73243139520307,17.4584647215534));
#47606=CARTESIAN_POINT('Ctrl Pts',(-5.20855850400624,9.72477709790203,17.4625183010151));
#47607=CARTESIAN_POINT('Ctrl Pts',(-5.19652326399056,9.72017680466359,17.4649549275125));
#47608=CARTESIAN_POINT('Ctrl Pts',(-5.12232129828262,9.69189636800157,17.4799357695392));
#47609=CARTESIAN_POINT('Ctrl Pts',(-5.04967091216259,9.66472261805258,17.4943429868338));
#47610=CARTESIAN_POINT('Ctrl Pts',(-4.93065570807978,9.62125919422881,17.5174112254402));
#47611=CARTESIAN_POINT('Ctrl Pts',(-4.86863819981268,9.59885699467281,17.5293067125793));
#47612=CARTESIAN_POINT('Ctrl Pts',(-4.79189210427276,9.57167794713725,17.5437478377285));
#47613=CARTESIAN_POINT('Ctrl Pts',(-4.75242097252906,9.55784774956845,17.5510983793266));
#47614=CARTESIAN_POINT('Ctrl Pts',(-4.73526946950167,9.5518711876235,17.5542752647172));
#47615=CARTESIAN_POINT('Ctrl Pts',(-4.72378284443704,9.54787610858598,17.5563989725316));
#47616=CARTESIAN_POINT('Ctrl Pts',(-4.71687145441156,9.54547754923709,17.5576740663135));
#47617=CARTESIAN_POINT('Ctrl Pts',(-4.56330035732465,9.49226685040711,17.5859623330004));
#47618=CARTESIAN_POINT('Ctrl Pts',(-4.38742083376464,9.43392133780629,17.6170101124104));
#47619=CARTESIAN_POINT('Ctrl Pts',(-4.08315840430196,9.34023826849138,17.6669296812749));
#47620=CARTESIAN_POINT('Ctrl Pts',(-3.97499707046061,9.30801566536103,17.6841092574927));
#47621=CARTESIAN_POINT('Ctrl Pts',(-3.80264428366793,9.25895958677314,17.7102778110509));
#47622=CARTESIAN_POINT('Ctrl Pts',(-3.71394019376392,9.23425373108708,17.7234604296094));
#47623=CARTESIAN_POINT('Ctrl Pts',(-3.60602861998748,9.20531488374581,17.7389081362217));
#47624=CARTESIAN_POINT('Ctrl Pts',(-3.55096696587716,9.19084300277489,17.746634997581));
#47625=CARTESIAN_POINT('Ctrl Pts',(-3.527132142568,9.18464310672296,17.7499456364573));
#47626=CARTESIAN_POINT('Ctrl Pts',(-3.51118960001799,9.18051068563473,17.7521523639014));
#47627=CARTESIAN_POINT('Ctrl Pts',(-3.50199535539259,9.17813690347825,17.7534200272329));
#47628=CARTESIAN_POINT('Ctrl Pts',(-3.2766948368566,9.12014890156824,17.7843882334437));
#47629=CARTESIAN_POINT('Ctrl Pts',(-3.0302774314496,9.06193661034056,17.815508643134));
#47630=CARTESIAN_POINT('Ctrl Pts',(-2.61873506037185,8.97833393532695,17.8602667918085));
#47631=CARTESIAN_POINT('Ctrl Pts',(-2.47456822618473,8.95110744004314,17.8748540188011));
#47632=CARTESIAN_POINT('Ctrl Pts',(-2.24783890916224,8.91224181782533,17.8956959311803));
#47633=CARTESIAN_POINT('Ctrl Pts',(-2.17051595919777,8.89961674957794,17.9024694686771));
#47634=CARTESIAN_POINT('Ctrl Pts',(-2.0123770373549,8.87520800329911,17.915571987208));
#47635=CARTESIAN_POINT('Ctrl Pts',(-1.93359205714849,8.86370156201463,17.9217519816094));
#47636=CARTESIAN_POINT('Ctrl Pts',(-1.51062468461165,8.8059715377584,17.9527772412711));
#47637=CARTESIAN_POINT('Ctrl Pts',(-1.1559767799876,8.77006019485985,17.9721409225942));
#47638=CARTESIAN_POINT('Ctrl Pts',(-0.599593913159634,8.73782855337055,
17.9895832486352));
#47639=CARTESIAN_POINT('Ctrl Pts',(-0.410064455901665,8.73068661704158,
17.9934643165518));
#47640=CARTESIAN_POINT('Ctrl Pts',(-0.119667517541742,8.7260893818246,17.9959679935218));
#47641=CARTESIAN_POINT('Ctrl Pts',(-0.0218514126762748,8.72557544902211,
17.9962493029249));
#47642=CARTESIAN_POINT('Ctrl Pts',(0.126398432740171,8.72641563924098,17.9957913442492));
#47643=CARTESIAN_POINT('Ctrl Pts',(0.200904777477956,8.72723861905749,17.9953427384674));
#47644=CARTESIAN_POINT('Ctrl Pts',(0.275983255260081,8.72868170504874,17.9945570124753));
#47645=CARTESIAN_POINT('Ctrl Pts',(0.326162714458018,8.72978326875773,17.9939574444567));
#47646=CARTESIAN_POINT('Ctrl Pts',(0.353068789745851,8.73045184547564,17.9935936527374));
#47647=CARTESIAN_POINT('Ctrl Pts',(0.751958403468875,8.74138449395115,17.9876467348906));
#47648=CARTESIAN_POINT('Ctrl Pts',(1.10849134973418,8.76677112538586,17.9738993830128));
#47649=CARTESIAN_POINT('Ctrl Pts',(1.61495191033288,8.82094465101678,17.9447265285685));
#47650=CARTESIAN_POINT('Ctrl Pts',(1.86109747593242,8.8520477561408,17.9280012002593));
#47651=CARTESIAN_POINT('Ctrl Pts',(2.13586905174054,8.89390623756821,17.905531504999));
#47652=CARTESIAN_POINT('Ctrl Pts',(2.25097153050302,8.91288546000701,17.8953504939764));
#47653=CARTESIAN_POINT('Ctrl Pts',(2.32711612345302,8.92575243891898,17.8884497539916));
#47654=CARTESIAN_POINT('Ctrl Pts',(2.36665276247385,8.93260467126174,17.8847756054096));
#47655=CARTESIAN_POINT('Ctrl Pts',(2.68815404379909,8.98955276178681,17.85424606372));
#47656=CARTESIAN_POINT('Ctrl Pts',(2.94945525844658,9.04484068918616,17.8246561887078));
#47657=CARTESIAN_POINT('Ctrl Pts',(3.30469052728873,9.12823135723393,17.7800773475732));
#47658=CARTESIAN_POINT('Ctrl Pts',(3.41698285804794,9.15611908146275,17.7651777008726));
#47659=CARTESIAN_POINT('Ctrl Pts',(3.57624221590447,9.19741366093029,17.7431262720328));
#47660=CARTESIAN_POINT('Ctrl Pts',(3.65357711026217,9.21792832465172,17.7321741939344));
#47661=CARTESIAN_POINT('Ctrl Pts',(3.739785280681,9.24150050145565,17.7195943535128));
#47662=CARTESIAN_POINT('Ctrl Pts',(3.77587109521795,9.25151267978903,17.7142520545844));
#47663=CARTESIAN_POINT('Ctrl Pts',(3.79973707286171,9.2581660471466,17.7107021529559));
#47664=CARTESIAN_POINT('Ctrl Pts',(3.8098321625265,9.26099167213174,17.7091946138522));
#47665=CARTESIAN_POINT('Ctrl Pts',(4.03906084095668,9.32550557489382,17.6747771483891));
#47666=CARTESIAN_POINT('Ctrl Pts',(4.23305855283995,9.38535894097414,17.6428776600593));
#47667=CARTESIAN_POINT('Ctrl Pts',(4.49143473070597,9.46908457807708,17.5983018997288));
#47668=CARTESIAN_POINT('Ctrl Pts',(4.57212339166817,9.49600414147767,17.5839784369806));
#47669=CARTESIAN_POINT('Ctrl Pts',(4.68500128562173,9.53450066553663,17.5635072343031));
#47670=CARTESIAN_POINT('Ctrl Pts',(4.73940145822609,9.55328036811316,17.5535239435117));
#47671=CARTESIAN_POINT('Ctrl Pts',(4.79930047111274,9.57430584208441,17.5423515809152));
#47672=CARTESIAN_POINT('Ctrl Pts',(4.82420693624594,9.58312192570992,17.5376678794198));
#47673=CARTESIAN_POINT('Ctrl Pts',(4.84064134847036,9.58895546402193,17.5345689006767));
#47674=CARTESIAN_POINT('Ctrl Pts',(4.8471229973513,9.59126108436074,17.5333441340759));
#47675=CARTESIAN_POINT('Ctrl Pts',(4.93440424627371,9.62241797040445,17.5167945121165));
#47676=CARTESIAN_POINT('Ctrl Pts',(5.00681738695592,9.64894999419244,17.5027116938825));
#47677=CARTESIAN_POINT('Ctrl Pts',(5.10768181043932,9.68655270637007,17.4827706331314));
#47678=CARTESIAN_POINT('Ctrl Pts',(5.15617520029604,9.70480850706302,17.4730940902559));
#47679=CARTESIAN_POINT('Ctrl Pts',(5.20935788349684,9.72508928042515,17.4623520315752));
#47680=CARTESIAN_POINT('Ctrl Pts',(5.23142340380461,9.73355857970071,17.4578677257988));
#47681=CARTESIAN_POINT('Ctrl Pts',(5.24597218218603,9.739154921829,17.4549049317256));
#47682=CARTESIAN_POINT('Ctrl Pts',(5.25210470602221,9.74151819612761,17.4536539000924));
#47683=CARTESIAN_POINT('Ctrl Pts',(5.39106103678595,9.79520571035242,17.4252374298913));
#47684=CARTESIAN_POINT('Ctrl Pts',(5.5020887329495,9.83993097584024,17.4016311175229));
#47685=CARTESIAN_POINT('Ctrl Pts',(5.593361696325,9.87744142971438,17.3818877156863));
#47686=CARTESIAN_POINT('Origin',(-5.599999999997,9.6786310860259,17.0348569100619));
#47687=CARTESIAN_POINT('Origin',(-5.599999999997,9.6786310860259,17.0348569100619));
#47688=CARTESIAN_POINT('',(-5.99999997117386,9.67863337111575,17.0348538908756));
#47689=CARTESIAN_POINT('Origin',(-5.6,9.67863108604804,17.0348569101035));
#47690=CARTESIAN_POINT('Origin',(-5.59998164336875,9.67863961983816,17.0348438488187));
#47691=CARTESIAN_POINT('Ctrl Pts',(-5.72202473568975,9.61344955698967,17.4236870330605));
#47692=CARTESIAN_POINT('Ctrl Pts',(-5.72274567064853,9.1758914447973,17.227024855994));
#47693=CARTESIAN_POINT('Ctrl Pts',(-5.72404121715671,8.29086220798215,16.7525775913613));
#47694=CARTESIAN_POINT('Ctrl Pts',(-5.72530537911657,7.0637852157259,15.8436323328137));
#47695=CARTESIAN_POINT('Ctrl Pts',(-5.72546529150377,5.9593366094895,14.7303948942631));
#47696=CARTESIAN_POINT('Ctrl Pts',(-5.72471353061148,5.03570888986459,13.4633046841625));
#47697=CARTESIAN_POINT('Ctrl Pts',(-5.72306572655457,4.31359098850255,12.0712170637154));
#47698=CARTESIAN_POINT('Ctrl Pts',(-5.72038901589368,3.83840721059553,10.6678390325755));
#47699=CARTESIAN_POINT('Ctrl Pts',(-5.71829740700494,3.65952909703187,9.72608608981356));
#47700=CARTESIAN_POINT('Ctrl Pts',(-5.71724182049107,3.60559725899456,9.2948909596003));
#47701=CARTESIAN_POINT('Ctrl Pts',(-5.90002849745086,9.63679782292734,17.3716661896694));
#47702=CARTESIAN_POINT('Ctrl Pts',(-5.90064146364177,9.20180721910066,17.1757869809176));
#47703=CARTESIAN_POINT('Ctrl Pts',(-5.9017416993345,8.32198023867081,16.7034321811413));
#47704=CARTESIAN_POINT('Ctrl Pts',(-5.9028112502954,7.10225243166773,15.7991880815107));
#47705=CARTESIAN_POINT('Ctrl Pts',(-5.90294650836853,6.00412626997486,14.6922156321237));
#47706=CARTESIAN_POINT('Ctrl Pts',(-5.90231053688296,5.085487591936,13.4325712074677));
#47707=CARTESIAN_POINT('Ctrl Pts',(-5.90091484041538,4.36673081244574,12.0486614223905));
#47708=CARTESIAN_POINT('Ctrl Pts',(-5.89863714804845,3.89298856491527,10.6534828562829));
#47709=CARTESIAN_POINT('Ctrl Pts',(-5.89685281246244,3.71409999207949,9.71696536617335));
#47710=CARTESIAN_POINT('Ctrl Pts',(-5.89594634491586,3.65996428723496,9.28813332545949));
#47711=CARTESIAN_POINT('Ctrl Pts',(-6.00728099553466,9.69953390946991,17.2318878304503));
#47712=CARTESIAN_POINT('Ctrl Pts',(-6.00760395673598,9.27115450686099,17.0387535402842));
#47713=CARTESIAN_POINT('Ctrl Pts',(-6.00818201774359,8.40460392931769,16.5730884304966));
#47714=CARTESIAN_POINT('Ctrl Pts',(-6.00873883246761,7.20353730477516,15.6822211593903));
#47715=CARTESIAN_POINT('Ctrl Pts',(-6.00880920187504,6.12189909393815,14.5918025726931));
#47716=CARTESIAN_POINT('Ctrl Pts',(-6.00847818758616,5.21697168858999,13.3513274687463));
#47717=CARTESIAN_POINT('Ctrl Pts',(-6.00774958520186,4.50853451476516,11.9883501791246));
#47718=CARTESIAN_POINT('Ctrl Pts',(-6.00654715789313,4.04115926875987,10.6143701706271));
#47719=CARTESIAN_POINT('Ctrl Pts',(-6.00559944219796,3.86430275187011,9.69181559903544));
#47720=CARTESIAN_POINT('Ctrl Pts',(-6.00511045427861,3.81066035891786,9.26940225083461));
#47721=CARTESIAN_POINT('Ctrl Pts',(-5.99966790181819,9.77609467523413,17.0613075954953));
#47722=CARTESIAN_POINT('Ctrl Pts',(-5.99963699057152,9.35567597393494,16.8717624111685));
#47723=CARTESIAN_POINT('Ctrl Pts',(-5.99957878702131,8.50506541600627,16.414659546472));
#47724=CARTESIAN_POINT('Ctrl Pts',(-5.99951367676562,7.32636687298965,15.5403949299101));
#47725=CARTESIAN_POINT('Ctrl Pts',(-5.99950536491651,6.26466320051636,14.4700735480911));
#47726=CARTESIAN_POINT('Ctrl Pts',(-5.99954420752702,5.37658269142921,13.2526794263663));
#47727=CARTESIAN_POINT('Ctrl Pts',(-5.99962585271713,4.68122009686565,11.9148587494722));
#47728=CARTESIAN_POINT('Ctrl Pts',(-5.99973680126801,4.22254572368814,10.5664376666286));
#47729=CARTESIAN_POINT('Ctrl Pts',(-5.99981416583464,4.04893806171432,9.66088387769014));
#47730=CARTESIAN_POINT('Ctrl Pts',(-5.99984092598252,3.99628630515258,9.24632947018055));
#47731=CARTESIAN_POINT('',(-5.99999618081983,3.99788654355748,9.34661202484151));
#47732=CARTESIAN_POINT('Ctrl Pts',(-6.,9.67863396518287,17.0348526023092));
#47733=CARTESIAN_POINT('Ctrl Pts',(-6.,9.24640194836271,16.8355809089051));
#47734=CARTESIAN_POINT('Ctrl Pts',(-6.,8.83275508448163,16.6077872907197));
#47735=CARTESIAN_POINT('Ctrl Pts',(-6.,8.43516131847461,16.3499544364876));
#47736=CARTESIAN_POINT('Ctrl Pts',(-6.,8.03756727126096,16.0921213998978));
#47737=CARTESIAN_POINT('Ctrl Pts',(-6.,7.65602634462916,15.8042490847697));
#47738=CARTESIAN_POINT('Ctrl Pts',(-6.,7.29796322038041,15.4912222280303));
#47739=CARTESIAN_POINT('Ctrl Pts',(-6.,6.93990009613191,15.1781953712911));
#47740=CARTESIAN_POINT('Ctrl Pts',(-6.,6.60531477426643,14.8400139729407));
#47741=CARTESIAN_POINT('Ctrl Pts',(-6.,6.29607548230007,14.4788351240543));
#47742=CARTESIAN_POINT('Ctrl Pts',(-6.,5.98683619033349,14.1176562751676));
#47743=CARTESIAN_POINT('Ctrl Pts',(-6.,5.70294292826608,13.7334799757447));
#47744=CARTESIAN_POINT('Ctrl Pts',(-6.,5.44842667074869,13.3317962248934));
#47745=CARTESIAN_POINT('Ctrl Pts',(-6.,5.19391041323149,12.9301124740424));
#47746=CARTESIAN_POINT('Ctrl Pts',(-6.,4.96877116026427,12.5109212717628));
#47747=CARTESIAN_POINT('Ctrl Pts',(-6.,4.7746677150985,12.076828535284));
#47748=CARTESIAN_POINT('Ctrl Pts',(-6.,4.58056426993259,11.6427357988049));
#47749=CARTESIAN_POINT('Ctrl Pts',(-6.,4.41749663256818,11.1937415281265));
#47750=CARTESIAN_POINT('Ctrl Pts',(-6.,4.28772377553626,10.7378297754049));
#47751=CARTESIAN_POINT('Ctrl Pts',(-6.,4.15795091850444,10.2819180226836));
#47752=CARTESIAN_POINT('Ctrl Pts',(-6.,4.06147284180507,9.81908878791919));
#47753=CARTESIAN_POINT('Ctrl Pts',(-6.,3.99788654321422,9.34661202516592));
#47754=CARTESIAN_POINT('Ctrl Pts',(-5.73278606918832,3.68907427304369,9.81543670344895));
#47755=CARTESIAN_POINT('Ctrl Pts',(-5.74643892975411,3.69157874331479,9.80199766513387));
#47756=CARTESIAN_POINT('Ctrl Pts',(-5.75940527740446,3.69473932546515,9.78873354297374));
#47757=CARTESIAN_POINT('Ctrl Pts',(-5.7716485988922,3.69839100959473,9.77571635192827));
#47758=CARTESIAN_POINT('Ctrl Pts',(-5.78419257321745,3.70213236622016,9.76237950453559));
#47759=CARTESIAN_POINT('Ctrl Pts',(-5.79597832116455,3.70638821389214,9.74930201408252));
#47760=CARTESIAN_POINT('Ctrl Pts',(-5.80701828852253,3.71100259495989,9.73655425995103));
#47761=CARTESIAN_POINT('Ctrl Pts',(-5.8185606921694,3.71582697959233,9.72322634701382));
#47762=CARTESIAN_POINT('Ctrl Pts',(-5.82928881694117,3.72104247748579,9.71025896007629));
#47763=CARTESIAN_POINT('Ctrl Pts',(-5.83925970990793,3.72650871517201,9.6977229197899));
#47764=CARTESIAN_POINT('Ctrl Pts',(-5.84579318371984,3.73009049274115,9.68950862131239));
#47765=CARTESIAN_POINT('Ctrl Pts',(-5.85200237370557,3.73378078310869,9.68147931558694));
#47766=CARTESIAN_POINT('Ctrl Pts',(-5.85790960796569,3.73755009977863,9.67365268746806));
#47767=CARTESIAN_POINT('Ctrl Pts',(-5.86794796082459,3.74395542062822,9.66035264699343));
#47768=CARTESIAN_POINT('Ctrl Pts',(-5.87708910768384,3.75056572619156,9.64762920607599));
#47769=CARTESIAN_POINT('Ctrl Pts',(-5.88541230482037,3.75721385440797,9.63553178398123));
#47770=CARTESIAN_POINT('Ctrl Pts',(-5.89033927120756,3.76114925371699,9.62837064252864));
#47771=CARTESIAN_POINT('Ctrl Pts',(-5.89498027758906,3.76509875741602,9.62142867264591));
#47772=CARTESIAN_POINT('Ctrl Pts',(-5.89935566970285,3.76903508538686,9.61471458108651));
#47773=CARTESIAN_POINT('Ctrl Pts',(-5.90523907304197,3.77432809788155,9.60568642825533));
#47774=CARTESIAN_POINT('Ctrl Pts',(-5.91064087265227,3.779595289029,9.59706928178317));
#47775=CARTESIAN_POINT('Ctrl Pts',(-5.91560821859055,3.78477485647406,9.58887630999103));
#47776=CARTESIAN_POINT('Ctrl Pts',(-5.91809189155969,3.78736464019659,9.58477982409497));
#47777=CARTESIAN_POINT('Ctrl Pts',(-5.92046687519904,3.78993256795288,9.58078937429346));
#47778=CARTESIAN_POINT('Ctrl Pts',(-5.9227391226194,3.79247183393863,9.57690601577689));
#47779=CARTESIAN_POINT('Ctrl Pts',(-5.92387524632958,3.7937414669315,9.5749643365186));
#47780=CARTESIAN_POINT('Ctrl Pts',(-5.92498568057128,3.79500393752615,9.57304942962578));
#47781=CARTESIAN_POINT('Ctrl Pts',(-5.92607115753564,3.79625843901833,9.57116141170833));
#47782=CARTESIAN_POINT('Ctrl Pts',(-5.92683305117489,3.79713897056225,9.56983621652749));
#47783=CARTESIAN_POINT('Ctrl Pts',(-5.92726953125371,3.79764818979171,9.56907222952432));
#47784=CARTESIAN_POINT('Ctrl Pts',(-5.92804136074465,3.79855856119187,9.56771569930345));
#47785=CARTESIAN_POINT('Ctrl Pts',(-5.92836916391853,3.79894520440501,9.56713956828348));
#47786=CARTESIAN_POINT('Ctrl Pts',(-5.92875713505322,3.79940444874364,9.56645654115736));
#47787=CARTESIAN_POINT('Ctrl Pts',(-5.92925343459007,3.79999725005728,9.5655781323251));
#47788=CARTESIAN_POINT('Ctrl Pts',(-5.93848645652589,3.8110255648672,9.54923645272486));
#47789=CARTESIAN_POINT('Ctrl Pts',(-5.94669689114229,3.8224449053479,9.53347789300259));
#47790=CARTESIAN_POINT('Ctrl Pts',(-5.95392299422338,3.83405494850678,9.51833954729964));
#47791=CARTESIAN_POINT('Ctrl Pts',(-5.96134516857754,3.84598001567197,9.50279044151191));
#47792=CARTESIAN_POINT('Ctrl Pts',(-5.96772976030061,3.85810556804016,9.48789569112109));
#47793=CARTESIAN_POINT('Ctrl Pts',(-5.97315960569138,3.87025001855399,9.47368658169972));
#47794=CARTESIAN_POINT('Ctrl Pts',(-5.97885729588574,3.88299353363197,9.45877656169101));
#47795=CARTESIAN_POINT('Ctrl Pts',(-5.98350473838865,3.89575733437832,9.44462148359316));
#47796=CARTESIAN_POINT('Ctrl Pts',(-5.98722767349291,3.90838022749538,9.43124761886934));
#47797=CARTESIAN_POINT('Ctrl Pts',(-5.99106252997875,3.92138259852372,9.4174717000202));
#47798=CARTESIAN_POINT('Ctrl Pts',(-5.9939175880687,3.93423549544542,9.40452456817365));
#47799=CARTESIAN_POINT('Ctrl Pts',(-5.99594423417257,3.94681679063525,9.39242564731228));
#47800=CARTESIAN_POINT('Ctrl Pts',(-5.99807144897294,3.96002241014849,9.37972633909279));
#47801=CARTESIAN_POINT('Ctrl Pts',(-5.99928703414559,3.97292904470642,9.36796138653384));
#47802=CARTESIAN_POINT('Ctrl Pts',(-5.99976393734273,3.98545223150753,9.35714494908657));
#47803=CARTESIAN_POINT('Ctrl Pts',(-5.99992341808622,3.98964009846637,9.35352783455197));
#47804=CARTESIAN_POINT('Ctrl Pts',(-6.00000020849968,3.99378551625259,9.35001673465345));
#47805=CARTESIAN_POINT('Ctrl Pts',(-6.00000045072924,3.99788654296547,9.34661202516627));
#47806=CARTESIAN_POINT('Ctrl Pts',(-5.71201400288887,3.68829715163933,9.85011170501378));
#47807=CARTESIAN_POINT('Ctrl Pts',(-5.71753251403363,3.68939869751833,9.84750341117836));
#47808=CARTESIAN_POINT('Ctrl Pts',(-5.76529487390022,3.69985385925291,9.82453497351882));
#47809=CARTESIAN_POINT('Ctrl Pts',(-5.85056111518657,3.73367616562962,9.77704813744305));
#47810=CARTESIAN_POINT('Ctrl Pts',(-5.94855988658026,3.81178308395445,9.70555474539447));
#47811=CARTESIAN_POINT('Ctrl Pts',(-6.01625395589241,3.91079812614269,9.63668369038972));
#47812=CARTESIAN_POINT('Ctrl Pts',(-6.04733191412374,4.00898590408443,9.5823388230584));
#47813=CARTESIAN_POINT('Ctrl Pts',(-6.05141294660998,4.07077663899963,9.55425433710709));
#47814=CARTESIAN_POINT('Ctrl Pts',(-6.0507177793919,4.09530166542757,9.54404505445509));
#47815=CARTESIAN_POINT('Ctrl Pts',(-5.59595655141215,3.61240315183009,9.56649342059599));
#47816=CARTESIAN_POINT('Ctrl Pts',(-5.60110598069255,3.61339890679393,9.56406447589219));
#47817=CARTESIAN_POINT('Ctrl Pts',(-5.6456815434348,3.62286184211323,9.54267394188476));
#47818=CARTESIAN_POINT('Ctrl Pts',(-5.72536604180584,3.65366544424186,9.49842961777456));
#47819=CARTESIAN_POINT('Ctrl Pts',(-5.81695119687203,3.72506232608075,9.4319382918881));
#47820=CARTESIAN_POINT('Ctrl Pts',(-5.88006121814607,3.81550180528306,9.36820597259601));
#47821=CARTESIAN_POINT('Ctrl Pts',(-5.90886715308718,3.90480301610222,9.31838067552393));
#47822=CARTESIAN_POINT('Ctrl Pts',(-5.91260953843266,3.96061446345423,9.2929624946597));
#47823=CARTESIAN_POINT('Ctrl Pts',(-5.91197130778005,3.98268771189454,9.28378361798423));
#47824=CARTESIAN_POINT('Ctrl Pts',(-5.57885092685922,3.33845035983965,9.41052417590997));
#47825=CARTESIAN_POINT('Ctrl Pts',(-5.5861727528405,3.33986641830796,9.40711957037098));
#47826=CARTESIAN_POINT('Ctrl Pts',(-5.64948567484334,3.35330499147511,9.37718630234053));
#47827=CARTESIAN_POINT('Ctrl Pts',(-5.7617056670393,3.39666414699678,9.31604358749384));
#47828=CARTESIAN_POINT('Ctrl Pts',(-5.89067084915357,3.49660116044179,9.22466059496501));
#47829=CARTESIAN_POINT('Ctrl Pts',(-5.98091140797734,3.62450296347671,9.13596530973809));
#47830=CARTESIAN_POINT('Ctrl Pts',(-6.02359980578094,3.75425184877456,9.06431252548699));
#47831=CARTESIAN_POINT('Ctrl Pts',(-6.02950843301525,3.83859796744313,9.02597213171389));
#47832=CARTESIAN_POINT('Ctrl Pts',(-6.02850758242405,3.8726184681507,9.01180311927841));
#47833=CARTESIAN_POINT('Ctrl Pts',(-5.67190623754282,3.04595868814745,9.4844095814992));
#47834=CARTESIAN_POINT('Ctrl Pts',(-5.68251837688113,3.04804572148206,9.47951365138588));
#47835=CARTESIAN_POINT('Ctrl Pts',(-5.77421430622641,3.06782257858551,9.43651502745686));
#47836=CARTESIAN_POINT('Ctrl Pts',(-5.93576666433574,3.13108394579195,9.34940645997486));
#47837=CARTESIAN_POINT('Ctrl Pts',(-6.12141055110656,3.2761090354012,9.21954946744644));
#47838=CARTESIAN_POINT('Ctrl Pts',(-6.25271771234329,3.46296215222781,9.09214763633029));
#47839=CARTESIAN_POINT('Ctrl Pts',(-6.31634594300365,3.65598776994707,8.98662376375804));
#47840=CARTESIAN_POINT('Ctrl Pts',(-6.32550617250183,3.78468387418799,8.92824050832422));
#47841=CARTESIAN_POINT('Ctrl Pts',(-6.32396076869737,3.83722167560608,8.90633083239327));
#47842=CARTESIAN_POINT('',(-5.99999999616514,3.21424233716894,9.29218337155546));
#47843=CARTESIAN_POINT('Ctrl Pts',(-5.99998809173024,3.99788654423531,9.34661202443565));
#47844=CARTESIAN_POINT('Ctrl Pts',(-5.99998614033841,3.9756966407273,9.33734346540929));
#47845=CARTESIAN_POINT('Ctrl Pts',(-5.99998781129199,3.95340271551789,9.32855288994148));
#47846=CARTESIAN_POINT('Ctrl Pts',(-6.00000062824778,3.93105674294894,9.32034398865034));
#47847=CARTESIAN_POINT('Ctrl Pts',(-6.00000707142181,3.91982326500558,9.3162173161008));
#47848=CARTESIAN_POINT('Ctrl Pts',(-6.00001566897004,3.90857713712436,9.31223733327578));
#47849=CARTESIAN_POINT('Ctrl Pts',(-6.0000244752767,3.89732800865246,9.30841467970623));
#47850=CARTESIAN_POINT('Ctrl Pts',(-6.00004292770395,3.87375697795109,9.30040482499851));
#47851=CARTESIAN_POINT('Ctrl Pts',(-6.00006398859164,3.85017088480974,9.29308821818177));
#47852=CARTESIAN_POINT('Ctrl Pts',(-6.00008526219979,3.82667220549539,9.28652704165603));
#47853=CARTESIAN_POINT('Ctrl Pts',(-6.00009914087016,3.81134192291226,9.28224660151418));
#47854=CARTESIAN_POINT('Ctrl Pts',(-6.00011245325881,3.79604956090522,9.27828690817963));
#47855=CARTESIAN_POINT('Ctrl Pts',(-6.00012171175511,3.78082955043215,9.27465535168952));
#47856=CARTESIAN_POINT('Ctrl Pts',(-6.00013624555717,3.75693748280786,9.26895460704177));
#47857=CARTESIAN_POINT('Ctrl Pts',(-6.00013967180186,3.73322340031339,9.26406506925698));
#47858=CARTESIAN_POINT('Ctrl Pts',(-6.00012396232745,3.70983392607146,9.25997440600767));
#47859=CARTESIAN_POINT('Ctrl Pts',(-6.00011958298683,3.70331362679944,9.25883404909624));
#47860=CARTESIAN_POINT('Ctrl Pts',(-6.00011380591141,3.69681861084596,9.25775547962216));
#47861=CARTESIAN_POINT('Ctrl Pts',(-6.00010670568716,3.69035213901702,9.25673776074387));
#47862=CARTESIAN_POINT('Ctrl Pts',(-6.00010098822708,3.6851450084649,9.25591824196999));
#47863=CARTESIAN_POINT('Ctrl Pts',(-6.0000944168878,3.67995638621582,9.25513817470758));
#47864=CARTESIAN_POINT('Ctrl Pts',(-6.000087197726,3.67478785822803,9.25439696282023));
#47865=CARTESIAN_POINT('Ctrl Pts',(-6.0000686539007,3.66151148589301,9.25249301550313));
#47866=CARTESIAN_POINT('Ctrl Pts',(-6.00005102575909,3.64818629218426,9.25081443241227));
#47867=CARTESIAN_POINT('Ctrl Pts',(-6.00003057014899,3.6350436628381,9.24939478068352));
#47868=CARTESIAN_POINT('Ctrl Pts',(-6.00000992967953,3.62178226225679,9.24796229942235));
#47869=CARTESIAN_POINT('Ctrl Pts',(-5.99998595813632,3.6087072522888,9.24679357696966));
#47870=CARTESIAN_POINT('Ctrl Pts',(-5.99996791547271,3.59607265740729,9.24587342005326));
#47871=CARTESIAN_POINT('Ctrl Pts',(-5.99995722328277,3.58858532121565,9.24532812958318));
#47872=CARTESIAN_POINT('Ctrl Pts',(-5.99994890967927,3.58125292365108,9.24486915457422));
#47873=CARTESIAN_POINT('Ctrl Pts',(-5.99994782973441,3.57412979372052,9.24448538624468));
#47874=CARTESIAN_POINT('Ctrl Pts',(-5.99994380484314,3.54758230563794,9.24305510415602));
#47875=CARTESIAN_POINT('Ctrl Pts',(-5.99996594985709,3.52094333406006,9.24258915158953));
#47876=CARTESIAN_POINT('Ctrl Pts',(-5.99999369856026,3.49438163998381,9.24317248831033));
#47877=CARTESIAN_POINT('Ctrl Pts',(-6.00002003739072,3.46916950834885,9.24372618651007));
#47878=CARTESIAN_POINT('Ctrl Pts',(-6.00005067895185,3.44402809178869,9.24522532892716));
#47879=CARTESIAN_POINT('Ctrl Pts',(-6.00007008721575,3.41912457662145,9.24769520019424));
#47880=CARTESIAN_POINT('Ctrl Pts',(-6.00007112610705,3.41779153389374,9.24782740819415));
#47881=CARTESIAN_POINT('Ctrl Pts',(-6.00007213476198,3.41645917622918,9.24796238580117));
#47882=CARTESIAN_POINT('Ctrl Pts',(-6.00007311154347,3.41512753029382,9.24810013286172));
#47883=CARTESIAN_POINT('Ctrl Pts',(-6.00009137615634,3.39022738858315,9.25067583353174));
#47884=CARTESIAN_POINT('Ctrl Pts',(-6.00009744663443,3.36557569992992,9.25422408903788));
#47885=CARTESIAN_POINT('Ctrl Pts',(-6.00008943235848,3.34134509983179,9.25871858948095));
#47886=CARTESIAN_POINT('Ctrl Pts',(-6.00008131870418,3.3168140362713,9.26326882247539));
#47887=CARTESIAN_POINT('Ctrl Pts',(-6.00005836465279,3.29271560150319,9.26878868405213));
#47888=CARTESIAN_POINT('Ctrl Pts',(-6.00003565609221,3.26922449003499,9.27519998313362));
#47889=CARTESIAN_POINT('Ctrl Pts',(-6.00001753957257,3.2504836640485,9.28031481308094));
#47890=CARTESIAN_POINT('Ctrl Pts',(-5.99999991840366,3.23212942824875,9.28599586008373));
#47891=CARTESIAN_POINT('Ctrl Pts',(-5.99999992132208,3.21424226856843,9.29218317323549));
#47892=CARTESIAN_POINT('Ctrl Pts',(-5.72001867923018,3.0799677452912,9.45352602807886));
#47893=CARTESIAN_POINT('Ctrl Pts',(-5.77263456943365,3.09390922256596,9.42780054399856));
#47894=CARTESIAN_POINT('Ctrl Pts',(-5.82217073197134,3.11234983333796,9.40144596360093));
#47895=CARTESIAN_POINT('Ctrl Pts',(-5.86880003058743,3.13480613498432,9.37455093300828));
#47896=CARTESIAN_POINT('Ctrl Pts',(-5.91542932732122,3.15726243572417,9.34765590350132));
#47897=CARTESIAN_POINT('Ctrl Pts',(-5.95915199503964,3.18373461472357,9.32022095924429));
#47898=CARTESIAN_POINT('Ctrl Pts',(-6.00000008250755,3.21424239912979,9.29218356476923));
#47899=CARTESIAN_POINT('Ctrl Pts',(6.05073416954824,-6.21799316481487,8.31849901783411));
#47900=CARTESIAN_POINT('Ctrl Pts',(6.05138851905234,-6.23846348656192,8.30285784976043));
#47901=CARTESIAN_POINT('Ctrl Pts',(6.04748115695756,-6.29320366773436,8.26366670974756));
#47902=CARTESIAN_POINT('Ctrl Pts',(6.01688298770343,-6.38906583647729,8.20581144498912));
#47903=CARTESIAN_POINT('Ctrl Pts',(5.94901053102531,-6.49891818272934,8.15405555171379));
#47904=CARTESIAN_POINT('Ctrl Pts',(5.85047649675774,-6.60050118995466,8.12193834043125));
#47905=CARTESIAN_POINT('Ctrl Pts',(5.76680004331251,-6.65737095906819,8.11655682688315));
#47906=CARTESIAN_POINT('Ctrl Pts',(5.72097979789639,-6.6816926781363,8.11871977358638));
#47907=CARTESIAN_POINT('Ctrl Pts',(5.71762411915974,-6.68343928363121,8.11890412240399));
#47908=CARTESIAN_POINT('Ctrl Pts',(5.91195465679019,-6.04887183299702,8.09084333278917));
#47909=CARTESIAN_POINT('Ctrl Pts',(5.91255544435238,-6.06728713996125,8.07676162461918));
#47910=CARTESIAN_POINT('Ctrl Pts',(5.90897244737554,-6.11676498715629,8.04139360101593));
#47911=CARTESIAN_POINT('Ctrl Pts',(5.8806167381171,-6.20428020149151,7.9889774803304));
#47912=CARTESIAN_POINT('Ctrl Pts',(5.81734518076637,-6.3053298833833,7.94212151691093));
#47913=CARTESIAN_POINT('Ctrl Pts',(5.72526412879784,-6.39917473945531,7.91333790687482));
#47914=CARTESIAN_POINT('Ctrl Pts',(5.64706911429235,-6.45181161411251,7.90892600936277));
#47915=CARTESIAN_POINT('Ctrl Pts',(5.60430646326424,-6.47432847354459,7.91117108524512));
#47916=CARTESIAN_POINT('Ctrl Pts',(5.60117502174684,-6.47594550881959,7.91135914934469));
#47917=CARTESIAN_POINT('Ctrl Pts',(6.02850429655224,-5.86846171619569,7.8594200448853));
#47918=CARTESIAN_POINT('Ctrl Pts',(6.0294458481419,-5.89685901208869,7.83772995718211));
#47919=CARTESIAN_POINT('Ctrl Pts',(6.02378949073807,-5.9716166886548,7.78420864811893));
#47920=CARTESIAN_POINT('Ctrl Pts',(5.98173069054818,-6.09820219289116,7.70765349338715));
#47921=CARTESIAN_POINT('Ctrl Pts',(5.89124051535816,-6.23988002999824,7.64065795139567));
#47922=CARTESIAN_POINT('Ctrl Pts',(5.76157170010822,-6.36977135011668,7.59951888803959));
#47923=CARTESIAN_POINT('Ctrl Pts',(5.65144406230163,-6.44290468661577,7.59275046404611));
#47924=CARTESIAN_POINT('Ctrl Pts',(5.5907186306291,-6.47449766812669,7.59572432625113));
#47925=CARTESIAN_POINT('Ctrl Pts',(5.58626901549766,-6.47676845393569,7.59597617732597));
#47926=CARTESIAN_POINT('Ctrl Pts',(6.32399708752164,-5.79500234059736,7.77590234717818));
#47927=CARTESIAN_POINT('Ctrl Pts',(6.32545039447524,-5.83887649506691,7.74242252558534));
#47928=CARTESIAN_POINT('Ctrl Pts',(6.31668181867899,-5.95288791984639,7.66066908075003));
#47929=CARTESIAN_POINT('Ctrl Pts',(6.25395529759717,-6.14035453070281,7.54621728843544));
#47930=CARTESIAN_POINT('Ctrl Pts',(6.12226590114595,-6.34546389958309,7.44724201576168));
#47931=CARTESIAN_POINT('Ctrl Pts',(5.93560336462689,-6.53156166818348,7.38615613310121));
#47932=CARTESIAN_POINT('Ctrl Pts',(5.77705748510178,-6.63648756796766,7.37524949342088));
#47933=CARTESIAN_POINT('Ctrl Pts',(5.68912159307504,-6.68208921880697,7.37912115719306));
#47934=CARTESIAN_POINT('Ctrl Pts',(5.68267531632909,-6.68536861183381,7.37945506135755));
#47935=CARTESIAN_POINT('',(5.73278512538254,-6.6558845698369,8.10254539185841));
#47936=CARTESIAN_POINT('',(5.72001596702532,-6.64701164882605,7.39409270018585));
#47937=CARTESIAN_POINT('Origin',(5.89875799467743,-6.95917611500265,7.74135837685731));
#47938=CARTESIAN_POINT('',(5.99999998587216,-6.44014763970973,7.42970560850941));
#47939=CARTESIAN_POINT('Ctrl Pts',(6.00000001391262,-6.44014774286491,7.4297057275149));
#47940=CARTESIAN_POINT('Ctrl Pts',(5.95924742401491,-6.47958993893993,7.4173332049442));
#47941=CARTESIAN_POINT('Ctrl Pts',(5.91558896907838,-6.51654787976713,7.40812577084738));
#47942=CARTESIAN_POINT('Ctrl Pts',(5.86896519300227,-6.55107434372493,7.40211809013247));
#47943=CARTESIAN_POINT('Ctrl Pts',(5.82234141692615,-6.58560080768272,7.39611040941757));
#47944=CARTESIAN_POINT('Ctrl Pts',(5.77275207242162,-6.61769538986344,7.39330201919218));
#47945=CARTESIAN_POINT('Ctrl Pts',(5.72001606109157,-6.64701181310764,7.39409288292955));
#47946=CARTESIAN_POINT('',(5.99998098390851,-6.09545783085286,8.13557311429686));
#47947=CARTESIAN_POINT('Ctrl Pts',(5.99998098390851,-6.09545783085286,8.13557311429686));
#47948=CARTESIAN_POINT('Ctrl Pts',(5.99997795080516,-6.09912681471699,8.10718396161426));
#47949=CARTESIAN_POINT('Ctrl Pts',(5.99997856657729,-6.10348550211984,8.07931777015222));
#47950=CARTESIAN_POINT('Ctrl Pts',(5.99997355844376,-6.10855067239734,8.05200283568773));
#47951=CARTESIAN_POINT('Ctrl Pts',(5.99997239516563,-6.10972719889876,8.04565818338163));
#47952=CARTESIAN_POINT('Ctrl Pts',(5.9999707973073,-6.1109416624435,8.0393432201366));
#47953=CARTESIAN_POINT('Ctrl Pts',(5.99996848874586,-6.11219397191406,8.0330581951774));
#47954=CARTESIAN_POINT('Ctrl Pts',(5.99995522862971,-6.1193870960483,7.9969577217872));
#47955=CARTESIAN_POINT('Ctrl Pts',(5.99992305431804,-6.12783083555669,7.96184754052742));
#47956=CARTESIAN_POINT('Ctrl Pts',(5.9999092524274,-6.13751521093299,7.92768174892519));
#47957=CARTESIAN_POINT('Ctrl Pts',(5.99990745008773,-6.13877985897252,7.92322016005754));
#47958=CARTESIAN_POINT('Ctrl Pts',(5.99990591277677,-6.14006565105881,7.91877462908017));
#47959=CARTESIAN_POINT('Ctrl Pts',(5.99990469357332,-6.14137257067106,7.91434501280618));
#47960=CARTESIAN_POINT('Ctrl Pts',(5.99989649855682,-6.15015718143404,7.88457083661982));
#47961=CARTESIAN_POINT('Ctrl Pts',(5.9998958870529,-6.15990751700441,7.85553451876249));
#47962=CARTESIAN_POINT('Ctrl Pts',(5.99989864392041,-6.17061785514147,7.82724658889151));
#47963=CARTESIAN_POINT('Ctrl Pts',(5.99990072599376,-6.17870664055037,7.8058826514079));
#47964=CARTESIAN_POINT('Ctrl Pts',(5.99990523562835,-6.18734279182029,7.78494486521122));
#47965=CARTESIAN_POINT('Ctrl Pts',(5.99991500873739,-6.19653415230066,7.7644298683282));
#47966=CARTESIAN_POINT('Ctrl Pts',(5.99991850715718,-6.19982432713193,7.75708624095635));
#47967=CARTESIAN_POINT('Ctrl Pts',(5.99992700898706,-6.20329286828286,7.74955169037503));
#47968=CARTESIAN_POINT('Ctrl Pts',(5.99993271621318,-6.20679880098116,7.74216830770547));
#47969=CARTESIAN_POINT('Ctrl Pts',(5.99993849506638,-6.21034873398374,7.73469226179561));
#47970=CARTESIAN_POINT('Ctrl Pts',(5.99994113580615,-6.21393686387291,7.72737150855663));
#47971=CARTESIAN_POINT('Ctrl Pts',(5.99994639777485,-6.21736531306685,7.72054982169873));
#47972=CARTESIAN_POINT('Ctrl Pts',(5.99994718576889,-6.21787873260638,7.71952825564151));
#47973=CARTESIAN_POINT('Ctrl Pts',(5.99994806094423,-6.21838848348708,7.71851785694636));
#47974=CARTESIAN_POINT('Ctrl Pts',(5.99994907258546,-6.21889381249274,7.71751975375738));
#47975=CARTESIAN_POINT('Ctrl Pts',(5.99997579529468,-6.23224218120401,7.69115465452693));
#47976=CARTESIAN_POINT('Ctrl Pts',(5.99996192119624,-6.24651037187084,7.66578871787388));
#47977=CARTESIAN_POINT('Ctrl Pts',(5.9999372794125,-6.26162446045842,7.64138874328849));
#47978=CARTESIAN_POINT('Ctrl Pts',(5.99991690557245,-6.27412079703479,7.62121483117286));
#47979=CARTESIAN_POINT('Ctrl Pts',(5.999890038424,-6.28719634665374,7.60170065612216));
#47980=CARTESIAN_POINT('Ctrl Pts',(5.99987287327607,-6.30083610829983,7.5828324562705));
#47981=CARTESIAN_POINT('Ctrl Pts',(5.99985320162157,-6.31646758899985,7.5612090650795));
#47982=CARTESIAN_POINT('Ctrl Pts',(5.99984785764865,-6.33284019468986,7.54043265309109));
#47983=CARTESIAN_POINT('Ctrl Pts',(5.99986495093018,-6.34996887007247,7.52050046833024));
#47984=CARTESIAN_POINT('Ctrl Pts',(5.99988150843523,-6.36656065957162,7.50119304341716));
#47985=CARTESIAN_POINT('Ctrl Pts',(5.99991970425662,-6.38386297476151,7.48267754176755));
#47986=CARTESIAN_POINT('Ctrl Pts',(5.99995446206205,-6.4019071796299,7.4649826235714));
#47987=CARTESIAN_POINT('Ctrl Pts',(5.99997833382845,-6.41429999437422,7.45282969997515));
#47988=CARTESIAN_POINT('Ctrl Pts',(5.99999989103997,-6.42704314418577,7.44106453666026));
#47989=CARTESIAN_POINT('Ctrl Pts',(5.9999998934196,-6.44014754776427,7.42970550243612));
#47990=CARTESIAN_POINT('Ctrl Pts',(5.99998098390851,-6.09545783085286,8.13557311429686));
#47991=CARTESIAN_POINT('Ctrl Pts',(5.99997772867445,-6.11094053579484,8.12985643031688));
#47992=CARTESIAN_POINT('Ctrl Pts',(5.99924872607125,-6.12747879190542,8.12421726742495));
#47993=CARTESIAN_POINT('Ctrl Pts',(5.997604829686,-6.14501797924142,8.11878177647199));
#47994=CARTESIAN_POINT('Ctrl Pts',(5.99698611775157,-6.15161918879596,8.11673602519944));
#47995=CARTESIAN_POINT('Ctrl Pts',(5.99623762779396,-6.15836181538866,8.11471942401007));
#47996=CARTESIAN_POINT('Ctrl Pts',(5.99534851590325,-6.16524155001333,8.11273984489372));
#47997=CARTESIAN_POINT('Ctrl Pts',(5.99290206688184,-6.18417158594679,8.10729290459006));
#47998=CARTESIAN_POINT('Ctrl Pts',(5.98939069302446,-6.20414337978211,8.1021243085497));
#47999=CARTESIAN_POINT('Ctrl Pts',(5.98464484566116,-6.22504366912051,8.09738742436529));
#48000=CARTESIAN_POINT('Ctrl Pts',(5.98034782442747,-6.24396736813623,8.09309851864123));
#48001=CARTESIAN_POINT('Ctrl Pts',(5.97503916761414,-6.26365224354456,8.08916334415599));
#48002=CARTESIAN_POINT('Ctrl Pts',(5.96858845952096,-6.2839738607091,8.08571964003558));
#48003=CARTESIAN_POINT('Ctrl Pts',(5.96735211223312,-6.28786871626649,8.08505961726167));
#48004=CARTESIAN_POINT('Ctrl Pts',(5.96607378803647,-6.29178683360547,8.08441772769999));
#48005=CARTESIAN_POINT('Ctrl Pts',(5.96475252746431,-6.29572714730741,8.0837950604321));
#48006=CARTESIAN_POINT('Ctrl Pts',(5.96410107363795,-6.29766993777001,8.08348805136608));
#48007=CARTESIAN_POINT('Ctrl Pts',(5.96343918144502,-6.29961812320199,8.08318571602489));
#48008=CARTESIAN_POINT('Ctrl Pts',(5.96276677815532,-6.30157158264049,8.08288816314251));
#48009=CARTESIAN_POINT('Ctrl Pts',(5.9581909831883,-6.31486513727338,8.08086327569404));
#48010=CARTESIAN_POINT('Ctrl Pts',(5.95312831785123,-6.32840360031641,8.07905954701971));
#48011=CARTESIAN_POINT('Ctrl Pts',(5.94755665828282,-6.34214417495224,8.07751341825763));
#48012=CARTESIAN_POINT('Ctrl Pts',(5.94477082849862,-6.34901446227015,8.07674035387659));
#48013=CARTESIAN_POINT('Ctrl Pts',(5.94185770909024,-6.35593526246158,8.07603170829155));
#48014=CARTESIAN_POINT('Ctrl Pts',(5.93881470100109,-6.36290026499228,8.07539249392606));
#48015=CARTESIAN_POINT('Ctrl Pts',(5.93729319695651,-6.36638276625764,8.07507288674331));
#48016=CARTESIAN_POINT('Ctrl Pts',(5.93573921753015,-6.3698763169927,8.07477063876403));
#48017=CARTESIAN_POINT('Ctrl Pts',(5.93415243365218,-6.37338008924375,8.0744863991385));
#48018=CARTESIAN_POINT('Ctrl Pts',(5.93309118143456,-6.37572343676769,8.07429629767785));
#48019=CARTESIAN_POINT('Ctrl Pts',(5.93174669274984,-6.378654997998,8.07407033155907));
#48020=CARTESIAN_POINT('Ctrl Pts',(5.93065585008325,-6.38100281960402,8.07389808521894));
#48021=CARTESIAN_POINT('Ctrl Pts',(5.93011566524478,-6.38216545989472,8.07381278890237));
#48022=CARTESIAN_POINT('Ctrl Pts',(5.92963855434378,-6.38318525846102,8.07374007905873));
#48023=CARTESIAN_POINT('Ctrl Pts',(5.9292933318568,-6.38392121979147,8.07368836917371));
#48024=CARTESIAN_POINT('Ctrl Pts',(5.92334489559235,-6.39660237247523,8.07279736998656));
#48025=CARTESIAN_POINT('Ctrl Pts',(5.91661161124661,-6.41017628257469,8.07209947444279));
#48026=CARTESIAN_POINT('Ctrl Pts',(5.90895442130354,-6.42453791539892,8.07172163154264));
#48027=CARTESIAN_POINT('Ctrl Pts',(5.90810063408666,-6.42613925722406,8.07167950153926));
#48028=CARTESIAN_POINT('Ctrl Pts',(5.90723535216071,-6.42775034845592,8.07164138054929));
#48029=CARTESIAN_POINT('Ctrl Pts',(5.90635837684122,-6.42937100889063,8.07160746788664));
#48030=CARTESIAN_POINT('Ctrl Pts',(5.89875324496737,-6.44342537969755,8.07131337720253));
#48031=CARTESIAN_POINT('Ctrl Pts',(5.89026820006472,-6.45820265893285,8.07133406150863));
#48032=CARTESIAN_POINT('Ctrl Pts',(5.88078908081662,-6.47357436698548,8.0717985590752));
#48033=CARTESIAN_POINT('Ctrl Pts',(5.87367899091882,-6.48510436500285,8.07214696902439));
#48034=CARTESIAN_POINT('Ctrl Pts',(5.8660096694548,-6.49696817421058,8.072745410005));
#48035=CARTESIAN_POINT('Ctrl Pts',(5.85773624959864,-6.50909451012828,8.07365714025404));
#48036=CARTESIAN_POINT('Ctrl Pts',(5.84731781891584,-6.52436478437901,8.07480525053566));
#48037=CARTESIAN_POINT('Ctrl Pts',(5.83594081812807,-6.54005343178411,8.07644904341306));
#48038=CARTESIAN_POINT('Ctrl Pts',(5.82352550448333,-6.55597597045343,8.07873664042811));
#48039=CARTESIAN_POINT('Ctrl Pts',(5.81177708120982,-6.57104322765119,8.08090135883807));
#48040=CARTESIAN_POINT('Ctrl Pts',(5.79909789939182,-6.58631935505125,8.0836433580915));
#48041=CARTESIAN_POINT('Ctrl Pts',(5.78545577118372,-6.60162414051487,8.087086205805));
#48042=CARTESIAN_POINT('Ctrl Pts',(5.7726902189806,-6.61594551580274,8.09030783307193));
#48043=CARTESIAN_POINT('Ctrl Pts',(5.75908137506514,-6.63029216541615,8.09414298561802));
#48044=CARTESIAN_POINT('Ctrl Pts',(5.74462482502411,-6.6444786197375,8.0987080025764));
#48045=CARTESIAN_POINT('Ctrl Pts',(5.74073850671199,-6.64829232889056,8.09993520470623));
#48046=CARTESIAN_POINT('Ctrl Pts',(5.73679106169321,-6.65209422866094,8.10121524939007));
#48047=CARTESIAN_POINT('Ctrl Pts',(5.73278271922475,-6.65588017670764,8.10255062446566));
#48048=CARTESIAN_POINT('Ctrl Pts',(5.99928507441383,-9.87990138305988,16.996213761673));
#48049=CARTESIAN_POINT('Ctrl Pts',(5.99928507441383,-9.88326633338716,16.9632224620409));
#48050=CARTESIAN_POINT('Ctrl Pts',(5.99928507441383,-9.93380725827969,16.441713240187));
#48051=CARTESIAN_POINT('Ctrl Pts',(5.99928507441383,-9.95153396276962,15.4241420274085));
#48052=CARTESIAN_POINT('Ctrl Pts',(5.99928507441383,-9.7585538486203,13.962336164721));
#48053=CARTESIAN_POINT('Ctrl Pts',(5.99928507441383,-9.35132498744714,12.5448501172522));
#48054=CARTESIAN_POINT('Ctrl Pts',(5.99928507441383,-8.73824353394044,11.2027127608678));
#48055=CARTESIAN_POINT('Ctrl Pts',(5.99928507441383,-7.93284774114545,9.96536136565117));
#48056=CARTESIAN_POINT('Ctrl Pts',(5.99928507441383,-7.00873643877852,8.92486523185514));
#48057=CARTESIAN_POINT('Ctrl Pts',(5.99928507441383,-6.3262035229329,8.33936349584419));
#48058=CARTESIAN_POINT('Ctrl Pts',(5.99928507441383,-6.00174807522006,8.09410018447627));
#48059=CARTESIAN_POINT('Ctrl Pts',(6.01063753142534,-10.0685448362718,17.0154707577556));
#48060=CARTESIAN_POINT('Ctrl Pts',(6.01063753142534,-10.0719743009096,16.9818450948751));
#48061=CARTESIAN_POINT('Ctrl Pts',(6.01063753142534,-10.1234844014194,16.4503158788653));
#48062=CARTESIAN_POINT('Ctrl Pts',(6.01063753142534,-10.141555854936,15.4134041054537));
#48063=CARTESIAN_POINT('Ctrl Pts',(6.01063753142534,-9.94485299521173,13.9234127767083));
#48064=CARTESIAN_POINT('Ctrl Pts',(6.01063753142534,-9.52986270675546,12.4789235515721));
#48065=CARTESIAN_POINT('Ctrl Pts',(6.01063753142534,-8.90499026070635,11.1109544163187));
#48066=CARTESIAN_POINT('Ctrl Pts',(6.01063753142534,-8.08420677078012,9.84997711608917));
#48067=CARTESIAN_POINT('Ctrl Pts',(6.01063753142534,-7.14233094405397,8.78947077084895));
#48068=CARTESIAN_POINT('Ctrl Pts',(6.01063753142534,-6.44679011346318,8.19281074633989));
#48069=CARTESIAN_POINT('Ctrl Pts',(6.01063753142534,-6.11609106980937,7.94282973159906));
#48070=CARTESIAN_POINT('Ctrl Pts',(5.90340740959394,-10.2250068268442,17.0314426236621));
#48071=CARTESIAN_POINT('Ctrl Pts',(5.90340740959394,-10.2284898000314,16.9972908161699));
#48072=CARTESIAN_POINT('Ctrl Pts',(5.90340740959394,-10.2808037405078,16.4574509580307));
#48073=CARTESIAN_POINT('Ctrl Pts',(5.90340740959394,-10.2991611308929,15.4044980097731));
#48074=CARTESIAN_POINT('Ctrl Pts',(5.90340740959394,-10.0993706040784,13.8911294895681));
#48075=CARTESIAN_POINT('Ctrl Pts',(5.90340740959394,-9.67794294214227,12.4242436699105));
#48076=CARTESIAN_POINT('Ctrl Pts',(5.90340740959394,-9.04329097746749,11.0348495051978));
#48077=CARTESIAN_POINT('Ctrl Pts',(5.90340740959394,-8.20974484096032,9.7542767402771));
#48078=CARTESIAN_POINT('Ctrl Pts',(5.90340740959394,-7.25313501315403,8.67717380786529));
#48079=CARTESIAN_POINT('Ctrl Pts',(5.90340740959394,-6.54680534150376,8.07125903319736));
#48080=CARTESIAN_POINT('Ctrl Pts',(5.90340740959394,-6.21092782262036,7.8173651275034));
#48081=CARTESIAN_POINT('Ctrl Pts',(5.72171463267843,-10.2827457696937,17.0373366983171));
#48082=CARTESIAN_POINT('Ctrl Pts',(5.72171463267843,-10.2862484890613,17.002990728433));
#48083=CARTESIAN_POINT('Ctrl Pts',(5.72171463267843,-10.3388590694426,16.4600840060095));
#48084=CARTESIAN_POINT('Ctrl Pts',(5.72171463267843,-10.3573219786997,15.4012114061234));
#48085=CARTESIAN_POINT('Ctrl Pts',(5.72171463267843,-10.1563920145498,13.8792160346507));
#48086=CARTESIAN_POINT('Ctrl Pts',(5.72171463267843,-9.73258877795812,12.4040652320039));
#48087=CARTESIAN_POINT('Ctrl Pts',(5.72171463267843,-9.09432789162046,11.0067646195493));
#48088=CARTESIAN_POINT('Ctrl Pts',(5.72171463267843,-8.2560719740424,9.71896056854079));
#48089=CARTESIAN_POINT('Ctrl Pts',(5.72171463267843,-7.29402487905501,8.63573302148622));
#48090=CARTESIAN_POINT('Ctrl Pts',(5.72171463267843,-6.58371381693797,8.02640297970358));
#48091=CARTESIAN_POINT('Ctrl Pts',(5.72171463267843,-6.24592529280697,7.77106510550619));
#48092=CARTESIAN_POINT('',(6.,-9.9133032909571,16.8993688494793));
#48093=CARTESIAN_POINT('Ctrl Pts',(5.99999999999973,-9.9133032909571,16.8993688494793));
#48094=CARTESIAN_POINT('Ctrl Pts',(5.99999999999973,-9.92726798483485,16.7473134109464));
#48095=CARTESIAN_POINT('Ctrl Pts',(6.00000000003746,-9.93769910712317,16.595447980401));
#48096=CARTESIAN_POINT('Ctrl Pts',(5.99999999795221,-9.94464892471596,16.4436799771047));
#48097=CARTESIAN_POINT('Ctrl Pts',(5.99999999586004,-9.95162180286593,16.2914083843728));
#48098=CARTESIAN_POINT('Ctrl Pts',(5.99999999148609,-9.95509022250395,16.1392344036198));
#48099=CARTESIAN_POINT('Ctrl Pts',(5.99999999087348,-9.95505464980814,15.9870607740922));
#48100=CARTESIAN_POINT('Ctrl Pts',(5.99999999026188,-9.95501913510092,15.8351352093599));
#48101=CARTESIAN_POINT('Ctrl Pts',(5.99999999695621,-9.9514910181508,15.6832095322195));
#48102=CARTESIAN_POINT('Ctrl Pts',(5.99999999953312,-9.94441903913389,15.5311901549495));
#48103=CARTESIAN_POINT('Ctrl Pts',(5.99999999982103,-9.94362892143478,15.5142057718932));
#48104=CARTESIAN_POINT('Ctrl Pts',(5.99999999999973,-9.94279451441727,15.4972202267563));
#48105=CARTESIAN_POINT('Ctrl Pts',(5.99999999999973,-9.94191570654023,15.4802333954616));
#48106=CARTESIAN_POINT('Ctrl Pts',(5.99999999999973,-9.94094255237386,15.4614229067532));
#48107=CARTESIAN_POINT('Ctrl Pts',(5.9999999997797,-9.93991594443028,15.4426107520415));
#48108=CARTESIAN_POINT('Ctrl Pts',(5.99999999940201,-9.93883579420981,15.4237975366115));
#48109=CARTESIAN_POINT('Ctrl Pts',(5.99999999572692,-9.92832550450536,15.2407374948734));
#48110=CARTESIAN_POINT('Ctrl Pts',(5.99999998184225,-9.91274149826588,15.057576758604));
#48111=CARTESIAN_POINT('Ctrl Pts',(5.99999998033318,-9.89207963590134,14.8748162763473));
#48112=CARTESIAN_POINT('Ctrl Pts',(5.99999997882271,-9.87139856928759,14.6918859266418));
#48113=CARTESIAN_POINT('Ctrl Pts',(5.9999999873102,-9.84563021940766,14.5093570258918));
#48114=CARTESIAN_POINT('Ctrl Pts',(5.99999999411999,-9.8148225770521,14.3277311598507));
#48115=CARTESIAN_POINT('Ctrl Pts',(5.99999999739309,-9.8000150339968,14.2404335730922));
#48116=CARTESIAN_POINT('Ctrl Pts',(5.99999999999973,-9.78404408500407,14.1533445516174));
#48117=CARTESIAN_POINT('Ctrl Pts',(5.99999999999973,-9.76691931257516,14.0665192561223));
#48118=CARTESIAN_POINT('Ctrl Pts',(5.99999999999973,-9.7602057349753,14.032480359468));
#48119=CARTESIAN_POINT('Ctrl Pts',(5.99999999960408,-9.75331357134629,13.9984822486694));
#48120=CARTESIAN_POINT('Ctrl Pts',(5.99999999898853,-9.74624308953661,13.9645259256645));
#48121=CARTESIAN_POINT('Ctrl Pts',(5.99999999507832,-9.70132904128378,13.7488240865275));
#48122=CARTESIAN_POINT('Ctrl Pts',(5.99999998615653,-9.6492238410253,13.5348078243482));
#48123=CARTESIAN_POINT('Ctrl Pts',(5.99999998771989,-9.59004045253633,13.3227596842198));
#48124=CARTESIAN_POINT('Ctrl Pts',(5.99999998928325,-9.53085706404735,13.1107115440914));
#48125=CARTESIAN_POINT('Ctrl Pts',(5.99999999999973,-9.46459533129902,12.9006309202312));
#48126=CARTESIAN_POINT('Ctrl Pts',(5.99999999999973,-9.39131593584195,12.6928136949694));
#48127=CARTESIAN_POINT('Ctrl Pts',(5.99999999999973,-9.37455367135169,12.6452766311913));
#48128=CARTESIAN_POINT('Ctrl Pts',(5.99999999934667,-9.35742661566423,12.5978569729541));
#48129=CARTESIAN_POINT('Ctrl Pts',(5.99999999845569,-9.33993664766838,12.5505627050574));
#48130=CARTESIAN_POINT('Ctrl Pts',(5.99999999449755,-9.26223771587858,12.3404585987361));
#48131=CARTESIAN_POINT('Ctrl Pts',(5.99999998895131,-9.17737250715791,12.1328304142742));
#48132=CARTESIAN_POINT('Ctrl Pts',(5.99999999115155,-9.08561181914581,11.9283179829288));
#48133=CARTESIAN_POINT('Ctrl Pts',(5.99999999312724,-9.00321607235455,11.7446777457656));
#48134=CARTESIAN_POINT('Ctrl Pts',(5.99999999999973,-8.91526129320293,11.5635498380372));
#48135=CARTESIAN_POINT('Ctrl Pts',(5.99999999999973,-8.82197657218222,11.3853836525694));
#48136=CARTESIAN_POINT('Ctrl Pts',(5.99999999999973,-8.79096372712254,11.3261516556857));
#48137=CARTESIAN_POINT('Ctrl Pts',(5.9999999991363,-8.75935995230306,11.2672485469129));
#48138=CARTESIAN_POINT('Ctrl Pts',(5.99999999780781,-8.72716898892441,11.2086816936824));
#48139=CARTESIAN_POINT('Ctrl Pts',(5.99999999336895,-8.61960963189566,11.0129928289979));
#48140=CARTESIAN_POINT('Ctrl Pts',(5.99999998477723,-8.50549803860959,10.8210557635332));
#48141=CARTESIAN_POINT('Ctrl Pts',(5.99999998688355,-8.38499730264774,10.6331578953627));
#48142=CARTESIAN_POINT('Ctrl Pts',(5.99999998863004,-8.28508151746534,10.477358323829));
#48143=CARTESIAN_POINT('Ctrl Pts',(5.99999999999973,-8.18077212285937,10.324336137916));
#48144=CARTESIAN_POINT('Ctrl Pts',(5.99999999999973,-8.07214107678254,10.1742724167866));
#48145=CARTESIAN_POINT('Ctrl Pts',(5.99999999999973,-8.02304831449606,10.1064553161024));
#48146=CARTESIAN_POINT('Ctrl Pts',(5.99999999683371,-7.97308075075413,10.039234252959));
#48147=CARTESIAN_POINT('Ctrl Pts',(5.99999999319106,-7.92226250667201,9.97264859238534));
#48148=CARTESIAN_POINT('Ctrl Pts',(5.99999998466704,-7.80334493725567,9.81683437533751));
#48149=CARTESIAN_POINT('Ctrl Pts',(5.99999997595993,-7.67976621500289,9.66450210452235));
#48150=CARTESIAN_POINT('Ctrl Pts',(5.99999997954458,-7.5519155657467,9.5160655345673));
#48151=CARTESIAN_POINT('Ctrl Pts',(5.99999998312923,-7.4240649164905,9.36762896461225));
#48152=CARTESIAN_POINT('Ctrl Pts',(5.99999999999973,-7.29194273064179,9.22308846257705));
#48153=CARTESIAN_POINT('Ctrl Pts',(5.99999999999973,-7.15597857436782,9.0828176121166));
#48154=CARTESIAN_POINT('Ctrl Pts',(5.99999999999973,-7.08651113747799,9.01114977907237));
#48155=CARTESIAN_POINT('Ctrl Pts',(5.99999999545184,-7.01602931504084,8.94061618500218));
#48156=CARTESIAN_POINT('Ctrl Pts',(5.99999999307309,-6.94451772313367,8.87118606265322));
#48157=CARTESIAN_POINT('Ctrl Pts',(5.9999999894095,-6.83438040522495,8.7642544833994));
#48158=CARTESIAN_POINT('Ctrl Pts',(5.99999999031162,-6.72180218208047,8.65993850515689));
#48159=CARTESIAN_POINT('Ctrl Pts',(5.99999999276239,-6.60672591906142,8.5581688414802));
#48160=CARTESIAN_POINT('Ctrl Pts',(5.99999999520021,-6.49225775995384,8.45693696491031));
#48161=CARTESIAN_POINT('Ctrl Pts',(5.9999999978678,-6.37531755059047,8.35822425283109));
#48162=CARTESIAN_POINT('Ctrl Pts',(5.99999999875692,-6.25581493514787,8.26200091361462));
#48163=CARTESIAN_POINT('Ctrl Pts',(5.99999999915085,-6.20286922387451,8.21936910077066));
#48164=CARTESIAN_POINT('Ctrl Pts',(5.99999999931877,-6.14942010854285,8.1772264711099));
#48165=CARTESIAN_POINT('Ctrl Pts',(5.99999999931449,-6.09545783333519,8.13557311294732));
#48166=CARTESIAN_POINT('',(5.73644276520453,-10.2877350949113,16.9337809954847));
#48167=CARTESIAN_POINT('Origin',(5.6,-9.91330329093393,16.8993688493888));
#48168=CARTESIAN_POINT('Ctrl Pts',(5.7364427639771,-10.2877350956467,16.9337809951854));
#48169=CARTESIAN_POINT('Ctrl Pts',(5.73708792260912,-10.3280497960652,16.4922344854671));
#48170=CARTESIAN_POINT('Ctrl Pts',(5.73762563125427,-10.3398885462273,16.0482065524611));
#48171=CARTESIAN_POINT('Ctrl Pts',(5.7380559556032,-10.323253700388,15.6057354409328));
#48172=CARTESIAN_POINT('Ctrl Pts',(5.7381218985348,-10.3207045755147,15.5379311386264));
#48173=CARTESIAN_POINT('Ctrl Pts',(5.73818531979119,-10.3174868144141,15.4701632949043));
#48174=CARTESIAN_POINT('Ctrl Pts',(5.73824621957937,-10.313600420569,15.4024463333027));
#48175=CARTESIAN_POINT('Ctrl Pts',(5.73865147700528,-10.2877384264188,14.951824050896));
#48176=CARTESIAN_POINT('Ctrl Pts',(5.73894508028782,-10.2322688266212,14.5034591043037));
#48177=CARTESIAN_POINT('Ctrl Pts',(5.73912707523813,-10.1478930445972,14.0611434726086));
#48178=CARTESIAN_POINT('Ctrl Pts',(5.73915087509495,-10.1368590487234,14.0033009408067));
#48179=CARTESIAN_POINT('Ctrl Pts',(5.73917276625726,-10.1253307016213,13.9455617894377));
#48180=CARTESIAN_POINT('Ctrl Pts',(5.73919274878682,-10.1133095567134,13.8879344352759));
#48181=CARTESIAN_POINT('Ctrl Pts',(5.73934700450547,-10.0205119786601,13.443078397285));
#48182=CARTESIAN_POINT('Ctrl Pts',(5.73938752580425,-9.89834963657934,13.004888446781));
#48183=CARTESIAN_POINT('Ctrl Pts',(5.73931431960101,-9.74808346097681,12.5770746854827));
#48184=CARTESIAN_POINT('Ctrl Pts',(5.7393053689643,-9.7297110022455,12.5247675668472));
#48185=CARTESIAN_POINT('Ctrl Pts',(5.73929471816761,-9.71091839539337,12.472615502568));
#48186=CARTESIAN_POINT('Ctrl Pts',(5.73928236718371,-9.69170792511209,12.4206252243643));
#48187=CARTESIAN_POINT('Ctrl Pts',(5.73918135673792,-9.53459832292005,11.9954314728928));
#48188=CARTESIAN_POINT('Ctrl Pts',(5.73896663198965,-9.34954214044669,11.5810624745185));
#48189=CARTESIAN_POINT('Ctrl Pts',(5.73863815758599,-9.13842733572597,11.1810270495251));
#48190=CARTESIAN_POINT('Ctrl Pts',(5.73859603581172,-9.11135511929459,11.1297286783854));
#48191=CARTESIAN_POINT('Ctrl Pts',(5.73855204348063,-9.08385435544975,11.0786659502261));
#48192=CARTESIAN_POINT('Ctrl Pts',(5.7385061804799,-9.05592899315542,11.027846211693));
#48193=CARTESIAN_POINT('Ctrl Pts',(5.73815298599507,-8.84087363714812,10.6364795090074));
#48194=CARTESIAN_POINT('Ctrl Pts',(5.73768885006914,-8.60063920364099,10.2595268562011));
#48195=CARTESIAN_POINT('Ctrl Pts',(5.73711370889943,-8.33732019141297,9.90009894299511));
#48196=CARTESIAN_POINT('Ctrl Pts',(5.73703020872958,-8.29909099934179,9.84791646436043));
#48197=CARTESIAN_POINT('Ctrl Pts',(5.73694436865899,-8.2603751832675,9.79610330116616));
#48198=CARTESIAN_POINT('Ctrl Pts',(5.73685618849917,-8.22117910196827,9.74466890558282));
#48199=CARTESIAN_POINT('Ctrl Pts',(5.73622838502973,-7.94212045794209,9.37847891382779));
#48200=CARTESIAN_POINT('Ctrl Pts',(5.73548196633125,-7.63872140676405,9.03149064911417));
#48201=CARTESIAN_POINT('Ctrl Pts',(5.73461686622672,-7.31395075498618,8.70648064284032));
#48202=CARTESIAN_POINT('Ctrl Pts',(5.73452247697748,-7.27851571361542,8.67101948600494));
#48203=CARTESIAN_POINT('Ctrl Pts',(5.73442667489549,-7.24282621420437,8.63581993734851));
#48204=CARTESIAN_POINT('Ctrl Pts',(5.73432945990849,-7.20688608431088,8.6008855793511));
#48205=CARTESIAN_POINT('Ctrl Pts',(5.73384874333807,-7.02916640840315,8.42813932607534));
#48206=CARTESIAN_POINT('Ctrl Pts',(5.73333347833963,-6.84531868177435,8.26187772439676));
#48207=CARTESIAN_POINT('Ctrl Pts',(5.73278365812027,-6.65588188879718,8.10254858488964));
#48208=CARTESIAN_POINT('Ctrl Pts',(5.99999999997511,-9.67862872910786,17.0348533156911));
#48209=CARTESIAN_POINT('Ctrl Pts',(5.99999999997511,-9.75700380810197,16.9899528681551));
#48210=CARTESIAN_POINT('Ctrl Pts',(5.99999999997511,-9.83522889702052,16.9447896029531));
#48211=CARTESIAN_POINT('Ctrl Pts',(5.99999999997511,-9.91330177297901,16.8993645966839));
#48212=CARTESIAN_POINT('Ctrl Pts',(6.00000263486451,-9.79664482225296,17.2408547729115));
#48213=CARTESIAN_POINT('Ctrl Pts',(6.00000263486451,-9.87548026830557,17.1956905812713));
#48214=CARTESIAN_POINT('Ctrl Pts',(6.00000263486451,-9.95416475310039,17.1502620839818));
#48215=CARTESIAN_POINT('Ctrl Pts',(6.00000263486451,-10.0326962223327,17.1045702551533));
#48216=CARTESIAN_POINT('Ctrl Pts',(5.83074066841747,-9.87940002138524,17.3853070349674));
#48217=CARTESIAN_POINT('Ctrl Pts',(5.83074066841747,-9.95855828585064,17.3399579007926));
#48218=CARTESIAN_POINT('Ctrl Pts',(5.83074066841747,-10.0375649080453,17.2943434175637));
#48219=CARTESIAN_POINT('Ctrl Pts',(5.83074066841747,-10.1164179518766,17.2484644875256));
#48220=CARTESIAN_POINT('Ctrl Pts',(5.59336110043933,-9.87744127562476,17.3818879717683));
#48221=CARTESIAN_POINT('Ctrl Pts',(5.59336110043933,-9.95659189925084,17.3365432150276));
#48222=CARTESIAN_POINT('Ctrl Pts',(5.59336110043933,-10.0355908967271,17.2909331339327));
#48223=CARTESIAN_POINT('Ctrl Pts',(5.59336110043933,-10.1144363291588,17.2450586324221));
#48224=CARTESIAN_POINT('',(5.9999999999561,-9.67863597085289,17.0348513552246));
#48225=CARTESIAN_POINT('',(5.59336167787126,-9.87744147108621,17.381887702864));
#48226=CARTESIAN_POINT('Origin',(5.6,-9.67863108576213,17.0348569102136));
#48227=CARTESIAN_POINT('',(5.59336169565921,-10.1144356128051,17.2450590601813));
#48228=CARTESIAN_POINT('Origin',(5.59336169595271,-7.59798961603702,13.03919108114));
#48229=CARTESIAN_POINT('Origin',(5.6,-9.9133032910197,16.8993688495356));
#48230=CARTESIAN_POINT('Ctrl Pts',(5.99999999999168,-9.67863900758509,17.0348496155183));
#48231=CARTESIAN_POINT('Ctrl Pts',(5.99999999999173,-9.704809124558,17.0198569673818));
#48232=CARTESIAN_POINT('Ctrl Pts',(5.99999999999975,-9.73095807774519,17.00483964126));
#48233=CARTESIAN_POINT('Ctrl Pts',(5.99999999999975,-9.75705556964899,16.9898117786181));
#48234=CARTESIAN_POINT('Ctrl Pts',(5.99999999999975,-9.7831530615528,16.9747839159761));
#48235=CARTESIAN_POINT('Ctrl Pts',(5.99999999999975,-9.80919909217321,16.959745516814));
#48236=CARTESIAN_POINT('Ctrl Pts',(5.99999999999975,-9.83523570648505,16.9446741824461));
#48237=CARTESIAN_POINT('Ctrl Pts',(5.99999999999975,-9.86127232079687,16.9296028480782));
#48238=CARTESIAN_POINT('Ctrl Pts',(5.99999999999975,-9.88729951880012,16.9144985785046));
#48239=CARTESIAN_POINT('Ctrl Pts',(5.99999999999975,-9.9133032909571,16.8993688494793));
#48240=CARTESIAN_POINT('Origin',(5.6,-9.91330329093393,16.8993688493888));
#48241=CARTESIAN_POINT('Origin',(5.600000004206,-9.91330328921746,16.8993688496408));
#48242=CARTESIAN_POINT('Ctrl Pts',(-5.69266253961901,-10.0630749584107,
17.2766486289707));
#48243=CARTESIAN_POINT('Ctrl Pts',(-5.65789849165985,-10.0769812343233,
17.2678653025353));
#48244=CARTESIAN_POINT('Ctrl Pts',(-5.54372221655544,-10.1222489973318,
17.2393099090453));
#48245=CARTESIAN_POINT('Ctrl Pts',(-5.34116379992913,-10.2002037509081,
17.1903133546863));
#48246=CARTESIAN_POINT('Ctrl Pts',(-5.07576041681189,-10.2978306297997,
17.1291591915671));
#48247=CARTESIAN_POINT('Ctrl Pts',(-4.78280587130533,-10.4000145999421,
17.065301068575));
#48248=CARTESIAN_POINT('Ctrl Pts',(-4.45929391303252,-10.5059967628546,
16.9991853363862));
#48249=CARTESIAN_POINT('Ctrl Pts',(-4.10060720841936,-10.6150288379794,
16.9312638063993));
#48250=CARTESIAN_POINT('Ctrl Pts',(-3.70134405537019,-10.7258628654771,
16.862309194946));
#48251=CARTESIAN_POINT('Ctrl Pts',(-3.25667833810229,-10.8361751048301,
16.7937702956078));
#48252=CARTESIAN_POINT('Ctrl Pts',(-2.76261624754771,-10.9424615311872,
16.7278328779196));
#48253=CARTESIAN_POINT('Ctrl Pts',(-2.2145737102596,-11.0402939926339,16.6672547928867));
#48254=CARTESIAN_POINT('Ctrl Pts',(-1.60552241530544,-11.1242420353307,
16.6154077498866));
#48255=CARTESIAN_POINT('Ctrl Pts',(-0.939003279753059,-11.1858223338615,
16.5775146241924));
#48256=CARTESIAN_POINT('Ctrl Pts',(-0.236719809617086,-11.2158434081714,
16.5591722813375));
#48257=CARTESIAN_POINT('Ctrl Pts',(0.464182390050123,-11.2096967358559,
16.5629102770733));
#48258=CARTESIAN_POINT('Ctrl Pts',(1.12883546536813,-11.170862628158,16.5867059961451));
#48259=CARTESIAN_POINT('Ctrl Pts',(1.73414248783393,-11.1079160719739,16.6254820470085));
#48260=CARTESIAN_POINT('Ctrl Pts',(2.27380839700242,-11.0299200690652,16.6736768114977));
#48261=CARTESIAN_POINT('Ctrl Pts',(2.75209280343738,-10.9437380722387,16.7270466558039));
#48262=CARTESIAN_POINT('Ctrl Pts',(3.179567188373,-10.8531427618628,16.7832417082349));
#48263=CARTESIAN_POINT('Ctrl Pts',(3.56235976801865,-10.7611382589682,16.8403865311068));
#48264=CARTESIAN_POINT('Ctrl Pts',(3.90390329062717,-10.6703740483985,16.8968252371846));
#48265=CARTESIAN_POINT('Ctrl Pts',(4.20699758400573,-10.5830036834202,16.9512104351589));
#48266=CARTESIAN_POINT('Ctrl Pts',(4.47553728859529,-10.5002614434386,17.0027677360216));
#48267=CARTESIAN_POINT('Ctrl Pts',(4.7143855071493,-10.4224791464794,17.0512867978894));
#48268=CARTESIAN_POINT('Ctrl Pts',(4.92835317176294,-10.3494685548629,17.0968840833541));
#48269=CARTESIAN_POINT('Ctrl Pts',(5.12118235045995,-10.2809878012257,17.1397122419037));
#48270=CARTESIAN_POINT('Ctrl Pts',(5.29544761530358,-10.2169248336399,17.1798450111274));
#48271=CARTESIAN_POINT('Ctrl Pts',(5.45302040146602,-10.157235748825,17.2173144652497));
#48272=CARTESIAN_POINT('Ctrl Pts',(5.58355164973166,-10.106475377781,17.2492584257149));
#48273=CARTESIAN_POINT('Ctrl Pts',(5.66171355133499,-10.0754541448553,17.2688299523486));
#48274=CARTESIAN_POINT('Ctrl Pts',(5.69263618025467,-10.0630794583498,17.2766460876169));
#48275=CARTESIAN_POINT('Ctrl Pts',(-5.75649720686471,-10.1846648990153,
17.2128720584055));
#48276=CARTESIAN_POINT('Ctrl Pts',(-5.72140107752118,-10.1986648957518,
17.2039351049194));
#48277=CARTESIAN_POINT('Ctrl Pts',(-5.60613425768153,-10.2442342837783,
17.174874254139));
#48278=CARTESIAN_POINT('Ctrl Pts',(-5.40163680541364,-10.3226887670576,
17.1249729790431));
#48279=CARTESIAN_POINT('Ctrl Pts',(-5.13366297613342,-10.4209067331027,
17.0626076171722));
#48280=CARTESIAN_POINT('Ctrl Pts',(-4.83781655802612,-10.5236857216695,
16.9974070511417));
#48281=CARTESIAN_POINT('Ctrl Pts',(-4.51103516393409,-10.6302700871289,
16.9298289327573));
#48282=CARTESIAN_POINT('Ctrl Pts',(-4.14862658342972,-10.7399128406559,
16.860335762575));
#48283=CARTESIAN_POINT('Ctrl Pts',(-3.74510168729925,-10.851361600653,16.7897161027685));
#48284=CARTESIAN_POINT('Ctrl Pts',(-3.29554845890987,-10.9622791410709,
16.7194498781575));
#48285=CARTESIAN_POINT('Ctrl Pts',(-2.79589484443845,-11.069137934311,16.6517739280095));
#48286=CARTESIAN_POINT('Ctrl Pts',(-2.24147534651171,-11.1674782931378,
16.5895170965467));
#48287=CARTESIAN_POINT('Ctrl Pts',(-1.62516077627618,-11.2518315982921,
16.5361473155307));
#48288=CARTESIAN_POINT('Ctrl Pts',(-0.950537739291694,-11.3136699997299,
16.497060155779));
#48289=CARTESIAN_POINT('Ctrl Pts',(-0.239625133653724,-11.3437751162513,
16.4780724300291));
#48290=CARTESIAN_POINT('Ctrl Pts',(0.469884024736187,-11.3376169473577,
16.4819505930994));
#48291=CARTESIAN_POINT('Ctrl Pts',(1.14268886717138,-11.2986518605244,16.5065488874252));
#48292=CARTESIAN_POINT('Ctrl Pts',(1.75532342712682,-11.2354290547684,16.5465228616901));
#48293=CARTESIAN_POINT('Ctrl Pts',(2.30140127461001,-11.1570507323928,16.5961182236132));
#48294=CARTESIAN_POINT('Ctrl Pts',(2.78524362272039,-11.0704204226496,16.650962897641));
#48295=CARTESIAN_POINT('Ctrl Pts',(3.21756803710182,-10.9793385182868,16.7086453435522));
#48296=CARTESIAN_POINT('Ctrl Pts',(3.60459802992447,-10.8868310186806,16.7672452384226));
#48297=CARTESIAN_POINT('Ctrl Pts',(3.94983127105897,-10.7955653931699,16.8250703222752));
#48298=CARTESIAN_POINT('Ctrl Pts',(4.25612453257301,-10.7077085873143,16.88074650159));
#48299=CARTESIAN_POINT('Ctrl Pts',(4.52743794110943,-10.6245017968007,16.9334872976845));
#48300=CARTESIAN_POINT('Ctrl Pts',(4.76870535582295,-10.5462778473736,16.9830829704242));
#48301=CARTESIAN_POINT('Ctrl Pts',(4.98480296232433,-10.4728460664202,17.0296568340121));
#48302=CARTESIAN_POINT('Ctrl Pts',(5.1795233546998,-10.4039615628841,17.0733681030989));
#48303=CARTESIAN_POINT('Ctrl Pts',(5.35547746058191,-10.3395100165887,17.1142950914743));
#48304=CARTESIAN_POINT('Ctrl Pts',(5.51456438643061,-10.2794463026207,17.1524745505953));
#48305=CARTESIAN_POINT('Ctrl Pts',(5.64634415384641,-10.2283555481259,17.1849988667016));
#48306=CARTESIAN_POINT('Ctrl Pts',(5.72525252118978,-10.1971277043966,17.2049169199058));
#48307=CARTESIAN_POINT('Ctrl Pts',(5.75647014480878,-10.184670688155,17.2128713579864));
#48308=CARTESIAN_POINT('Ctrl Pts',(-5.81361907770973,-10.2517346582615,
17.0898712656509));
#48309=CARTESIAN_POINT('Ctrl Pts',(-5.77819645091898,-10.2657916980671,
17.0808138235748));
#48310=CARTESIAN_POINT('Ctrl Pts',(-5.66186163142478,-10.3115390424439,
17.0513590148227));
#48311=CARTESIAN_POINT('Ctrl Pts',(-5.4554863139952,-10.3902563547935,17.0007659322332));
#48312=CARTESIAN_POINT('Ctrl Pts',(-5.18504873353398,-10.4887261479065,
16.9374955140954));
#48313=CARTESIAN_POINT('Ctrl Pts',(-4.88645673350072,-10.5917076816743,
16.8713088940619));
#48314=CARTESIAN_POINT('Ctrl Pts',(-4.55660229647095,-10.6984534721325,
16.802671434488));
#48315=CARTESIAN_POINT('Ctrl Pts',(-4.19073342277236,-10.808221602351,16.7320536351322));
#48316=CARTESIAN_POINT('Ctrl Pts',(-3.78329293118505,-10.9197598564323,
16.6602564585697));
#48317=CARTESIAN_POINT('Ctrl Pts',(-3.32930551518025,-11.0307265753496,
16.5887833721865));
#48318=CARTESIAN_POINT('Ctrl Pts',(-2.82464539782738,-11.1375863407278,
16.5199084631354));
#48319=CARTESIAN_POINT('Ctrl Pts',(-2.26459202118377,-11.235870852726,16.4565105508145));
#48320=CARTESIAN_POINT('Ctrl Pts',(-1.64194486442485,-11.320106064408,16.4021228636622));
#48321=CARTESIAN_POINT('Ctrl Pts',(-0.960344264318984,-11.3817817301385,
16.3622528822177));
#48322=CARTESIAN_POINT('Ctrl Pts',(-0.242081705222581,-11.4117358685156,
16.3428532574355));
#48323=CARTESIAN_POINT('Ctrl Pts',(0.474713498383719,-11.4056180786119,
16.3468196523771));
#48324=CARTESIAN_POINT('Ctrl Pts',(1.15448587132591,-11.3668108697193,16.3719352137425));
#48325=CARTESIAN_POINT('Ctrl Pts',(1.77344785678181,-11.3037311804594,16.4126987703441));
#48326=CARTESIAN_POINT('Ctrl Pts',(2.32512789356553,-11.2254499630162,16.4632331992705));
#48327=CARTESIAN_POINT('Ctrl Pts',(2.8138835116069,-11.1388660220307,16.5190811568224));
#48328=CARTESIAN_POINT('Ctrl Pts',(3.25054531281605,-11.0477872223285,16.5777881968641));
#48329=CARTESIAN_POINT('Ctrl Pts',(3.64140752922088,-10.95524744967,16.6374017121183));
#48330=CARTESIAN_POINT('Ctrl Pts',(3.99001338647845,-10.8639213867097,16.6962025023282));
#48331=CARTESIAN_POINT('Ctrl Pts',(4.2992597178733,-10.7759819686143,16.7527959847812));
#48332=CARTESIAN_POINT('Ctrl Pts',(4.57315676078164,-10.6926745629042,16.8063854846301));
#48333=CARTESIAN_POINT('Ctrl Pts',(4.81669596217747,-10.6143340261694,16.8567603524753));
#48334=CARTESIAN_POINT('Ctrl Pts',(5.03480844630179,-10.5407698820821,16.904047859267));
#48335=CARTESIAN_POINT('Ctrl Pts',(5.23132995987367,-10.4717364368529,16.948411336553));
#48336=CARTESIAN_POINT('Ctrl Pts',(5.40890279612314,-10.4071184861256,16.9899320138223));
#48337=CARTESIAN_POINT('Ctrl Pts',(5.56945053459471,-10.3468710450711,17.0286496664754));
#48338=CARTESIAN_POINT('Ctrl Pts',(5.70244390694285,-10.2955983500078,17.0616208273054));
#48339=CARTESIAN_POINT('Ctrl Pts',(5.7820837103127,-10.2642485670913,17.0818090366983));
#48340=CARTESIAN_POINT('Ctrl Pts',(5.81359156453149,-10.2517426167626,17.0898715756317));
#48341=CARTESIAN_POINT('Ctrl Pts',(-5.84786853141265,-10.2455091741718,
16.9427568836198));
#48342=CARTESIAN_POINT('Ctrl Pts',(-5.81221749608519,-10.2595705697258,
16.9336460964131));
#48343=CARTESIAN_POINT('Ctrl Pts',(-5.69513979505893,-10.3053222964001,
16.9040200007179));
#48344=CARTESIAN_POINT('Ctrl Pts',(-5.4874797057468,-10.3839920616726,16.8531431733464));
#48345=CARTESIAN_POINT('Ctrl Pts',(-5.21538283686595,-10.482304500486,16.7895290278166));
#48346=CARTESIAN_POINT('Ctrl Pts',(-4.91496901490327,-10.58504037815,16.7229906696414));
#48347=CARTESIAN_POINT('Ctrl Pts',(-4.58310798543357,-10.6914629472664,
16.6539954113149));
#48348=CARTESIAN_POINT('Ctrl Pts',(-4.21501992700169,-10.8008376894694,
16.5830168063254));
#48349=CARTESIAN_POINT('Ctrl Pts',(-3.80511818472374,-10.9119170755123,
16.5108612726519));
#48350=CARTESIAN_POINT('Ctrl Pts',(-3.34840461299257,-11.0223652836609,
16.4390415920042));
#48351=CARTESIAN_POINT('Ctrl Pts',(-2.84073935392859,-11.1286567864201,
16.3698447805026));
#48352=CARTESIAN_POINT('Ctrl Pts',(-2.2773886440694,-11.2263399371374,16.3061645413724));
#48353=CARTESIAN_POINT('Ctrl Pts',(-1.65113026598497,-11.3099693976257,
16.2515501009313));
#48354=CARTESIAN_POINT('Ctrl Pts',(-0.965651068761255,-11.3711094017989,
16.2115286076516));
#48355=CARTESIAN_POINT('Ctrl Pts',(-0.243395249204597,-11.4007213303408,
16.1920663039319));
#48356=CARTESIAN_POINT('Ctrl Pts',(0.477305864509668,-11.394684130552,16.1960442118997));
#48357=CARTESIAN_POINT('Ctrl Pts',(1.16089199366367,-11.3562776831491,16.2212463556512));
#48358=CARTESIAN_POINT('Ctrl Pts',(1.78339237472185,-11.2937181300105,16.2621691278305));
#48359=CARTESIAN_POINT('Ctrl Pts',(2.33828065309362,-11.2159838790585,16.3129169306687));
#48360=CARTESIAN_POINT('Ctrl Pts',(2.82991520548475,-11.1299257391801,16.3690143067492));
#48361=CARTESIAN_POINT('Ctrl Pts',(3.26917472852458,-11.0393367756593,16.4279947460898));
#48362=CARTESIAN_POINT('Ctrl Pts',(3.6623796608692,-10.9472425933416,16.4878950535873));
#48363=CARTESIAN_POINT('Ctrl Pts',(4.01308659024824,-10.8563123186887,16.5469861157905));
#48364=CARTESIAN_POINT('Ctrl Pts',(4.3242042468058,-10.7687158078831,16.6038648539006));
#48365=CARTESIAN_POINT('Ctrl Pts',(4.59976346742793,-10.6856986852594,16.6577291719566));
#48366=CARTESIAN_POINT('Ctrl Pts',(4.84478385417697,-10.6075982814546,16.7083662643601));
#48367=CARTESIAN_POINT('Ctrl Pts',(5.06422562949391,-10.5342268808267,16.7559033549902));
#48368=CARTESIAN_POINT('Ctrl Pts',(5.26194812135429,-10.4653404258265,16.8005042877178));
#48369=CARTESIAN_POINT('Ctrl Pts',(5.44061113093055,-10.4008244566688,16.8422507280134));
#48370=CARTESIAN_POINT('Ctrl Pts',(5.6021525906504,-10.3406354448213,16.8811829719989));
#48371=CARTESIAN_POINT('Ctrl Pts',(5.73598086912627,-10.2893801809809,16.9143414007394));
#48372=CARTESIAN_POINT('Ctrl Pts',(5.81612985524781,-10.2580273269292,16.934647159681));
#48373=CARTESIAN_POINT('Ctrl Pts',(5.84784094545612,-10.2455195636508,16.9427570906608));
#48374=CARTESIAN_POINT('',(-5.593361696257,-10.114435612469,17.2450590606623));
#48375=CARTESIAN_POINT('Ctrl Pts',(-5.593361696257,-10.114435612469,17.2450590606623));
#48376=CARTESIAN_POINT('Ctrl Pts',(-5.53985803395109,-10.1354527263307,
17.2318032775356));
#48377=CARTESIAN_POINT('Ctrl Pts',(-5.47932176399903,-10.1588523176192,
17.2170630927394));
#48378=CARTESIAN_POINT('Ctrl Pts',(-5.377968447602,-10.1974253312631,17.1928124140373));
#48379=CARTESIAN_POINT('Ctrl Pts',(-5.34242585689151,-10.2108546235383,
17.1843762811573));
#48380=CARTESIAN_POINT('Ctrl Pts',(-5.28647474295853,-10.2317797500377,
17.1712407072089));
#48381=CARTESIAN_POINT('Ctrl Pts',(-5.25783987902523,-10.2424369641257,
17.164552952931));
#48382=CARTESIAN_POINT('Ctrl Pts',(-5.22821605464172,-10.2533661581861,
17.1576975073026));
#48383=CARTESIAN_POINT('Ctrl Pts',(-5.20824706939711,-10.2607101238115,
17.1530915356416));
#48384=CARTESIAN_POINT('Ctrl Pts',(-5.19619845864606,-10.2651250909784,
17.150322977261));
#48385=CARTESIAN_POINT('Ctrl Pts',(-5.12194820685333,-10.2922550768492,
17.1333118578821));
#48386=CARTESIAN_POINT('Ctrl Pts',(-5.04924772603904,-10.3183350163019,
17.1169723072663));
#48387=CARTESIAN_POINT('Ctrl Pts',(-4.93014661931982,-10.3600705978436,
17.0908496926532));
#48388=CARTESIAN_POINT('Ctrl Pts',(-4.86808346958576,-10.3815871067203,
17.0773880893416));
#48389=CARTESIAN_POINT('Ctrl Pts',(-4.79127941790741,-10.4076995780588,
17.0610606025377));
#48390=CARTESIAN_POINT('Ctrl Pts',(-4.75177813115442,-10.4209888516975,
17.0527533358605));
#48391=CARTESIAN_POINT('Ctrl Pts',(-4.73461345235018,-10.4267320296099,
17.0491636650573));
#48392=CARTESIAN_POINT('Ctrl Pts',(-4.72311798738954,-10.4305711815526,
17.046764169854));
#48393=CARTESIAN_POINT('Ctrl Pts',(-4.71619978461696,-10.4328766746857,
17.0453232896371));
#48394=CARTESIAN_POINT('Ctrl Pts',(-4.56255901740035,-10.483996393471,17.0133757063631));
#48395=CARTESIAN_POINT('Ctrl Pts',(-4.3865990321201,-10.540073840317,16.978360696291));
#48396=CARTESIAN_POINT('Ctrl Pts',(-4.0821965558671,-10.6301690061502,16.9221750041953));
#48397=CARTESIAN_POINT('Ctrl Pts',(-3.97398531406067,-10.6611651185234,
16.9028549809191));
#48398=CARTESIAN_POINT('Ctrl Pts',(-3.80155282676788,-10.7083647078009,
16.8734499833083));
#48399=CARTESIAN_POINT('Ctrl Pts',(-3.71280767697568,-10.7321382323889,
16.8586428785537));
#48400=CARTESIAN_POINT('Ctrl Pts',(-3.60484608312967,-10.7599898039259,
16.8413024969385));
#48401=CARTESIAN_POINT('Ctrl Pts',(-3.54975888976788,-10.7739192136909,
16.8326318138909));
#48402=CARTESIAN_POINT('Ctrl Pts',(-3.52591300766166,-10.7798869881474,
16.8289174252434));
#48403=CARTESIAN_POINT('Ctrl Pts',(-3.50996306737948,-10.7838647560478,
16.8264417203206));
#48404=CARTESIAN_POINT('Ctrl Pts',(-3.50076307772626,-10.7861501079709,
16.8250194080026));
#48405=CARTESIAN_POINT('Ctrl Pts',(-3.27540677250763,-10.8419576514817,
16.7902881080184));
#48406=CARTESIAN_POINT('Ctrl Pts',(-3.02893969710884,-10.8980033528736,
16.7554422862958));
#48407=CARTESIAN_POINT('Ctrl Pts',(-2.6173294603214,-10.978539531806,16.7054362266149));
#48408=CARTESIAN_POINT('Ctrl Pts',(-2.47314111077737,-11.0047751539418,
16.6891576239548));
#48409=CARTESIAN_POINT('Ctrl Pts',(-2.24638118053902,-11.0422394556187,
16.6659313380236));
#48410=CARTESIAN_POINT('Ctrl Pts',(-2.16904830280584,-11.0544116122549,
16.6583885082993));
#48411=CARTESIAN_POINT('Ctrl Pts',(-2.01089007869873,-11.0779494736167,
16.6438097033959));
#48412=CARTESIAN_POINT('Ctrl Pts',(-1.93207851175822,-11.0890500154442,
16.6369377924131));
#48413=CARTESIAN_POINT('Ctrl Pts',(-1.50915171111936,-11.1447334756106,
16.602486057467));
#48414=CARTESIAN_POINT('Ctrl Pts',(-1.15456312141725,-11.179414968581,16.581094880351));
#48415=CARTESIAN_POINT('Ctrl Pts',(-0.598309513077577,-11.2105762749662,
16.5619397177837));
#48416=CARTESIAN_POINT('Ctrl Pts',(-0.408829856333268,-11.2174892628756,
16.557706909214));
#48417=CARTESIAN_POINT('Ctrl Pts',(-0.118517690270173,-11.2219303194708,
16.5549932439991));
#48418=CARTESIAN_POINT('Ctrl Pts',(0.0281615629980323,-11.2226689944669,
16.5545440520554));
#48419=CARTESIAN_POINT('Ctrl Pts',(0.201952906391755,-11.2207893532392,
16.555691075836));
#48420=CARTESIAN_POINT('Ctrl Pts',(0.277006099542097,-11.2193823030147,
16.556551060769));
#48421=CARTESIAN_POINT('Ctrl Pts',(0.32716849249538,-11.2183090012549,16.5572072730465));
#48422=CARTESIAN_POINT('Ctrl Pts',(0.354069491480004,-11.2176578450654,
16.5576054971895));
#48423=CARTESIAN_POINT('Ctrl Pts',(0.75274992570008,-11.2070187026837,16.5641139248419));
#48424=CARTESIAN_POINT('Ctrl Pts',(1.1090999952353,-11.1824152262659,16.5792286931375));
#48425=CARTESIAN_POINT('Ctrl Pts',(1.61530723788318,-11.1300744467122,16.6115515562428));
#48426=CARTESIAN_POINT('Ctrl Pts',(1.86133139379339,-11.1000478603117,16.6301191065388));
#48427=CARTESIAN_POINT('Ctrl Pts',(2.13597051121459,-11.0596761937399,16.6551243093524));
#48428=CARTESIAN_POINT('Ctrl Pts',(2.25101819057925,-11.0413778628387,16.6664651533834));
#48429=CARTESIAN_POINT('Ctrl Pts',(2.32712668803787,-11.0289738997268,16.6741543546353));
#48430=CARTESIAN_POINT('Ctrl Pts',(2.36663752496652,-11.0223702200823,16.6782487949033));
#48431=CARTESIAN_POINT('Ctrl Pts',(2.68805207114582,-10.967472195256,16.7122929768115));
#48432=CARTESIAN_POINT('Ctrl Pts',(2.94928878969231,-10.9142187883781,16.7453687479245));
#48433=CARTESIAN_POINT('Ctrl Pts',(3.3044462170927,-10.8339400967379,16.7952833992631));
#48434=CARTESIAN_POINT('Ctrl Pts',(3.41671575115627,-10.8071002673444,16.8119803720291));
#48435=CARTESIAN_POINT('Ctrl Pts',(3.57594563964679,-10.7673664139986,16.8367102355905));
#48436=CARTESIAN_POINT('Ctrl Pts',(3.65326698074084,-10.7476293920049,16.8489972383141));
#48437=CARTESIAN_POINT('Ctrl Pts',(3.73946140650262,-10.7249543835214,16.8631179578464));
#48438=CARTESIAN_POINT('Ctrl Pts',(3.77554177350454,-10.7153240107291,16.8691161813833));
#48439=CARTESIAN_POINT('Ctrl Pts',(3.79940421790988,-10.7089245228322,16.8731022769998));
#48440=CARTESIAN_POINT('Ctrl Pts',(3.80949575899816,-10.7062073375777,16.8747948247689));
#48441=CARTESIAN_POINT('Ctrl Pts',(4.03872720869192,-10.6441486480237,16.9134538283418));
#48442=CARTESIAN_POINT('Ctrl Pts',(4.23272945063578,-10.5865995058161,16.9493365218276));
#48443=CARTESIAN_POINT('Ctrl Pts',(4.49111530631149,-10.5061357349937,16.9995553690905));
#48444=CARTESIAN_POINT('Ctrl Pts',(4.57180767366338,-10.4802720452767,17.0157062827));
#48445=CARTESIAN_POINT('Ctrl Pts',(4.68469184788119,-10.4432955350863,17.0388094058357));
#48446=CARTESIAN_POINT('Ctrl Pts',(4.73909534078758,-10.4252599357605,17.0500814197759));
#48447=CARTESIAN_POINT('Ctrl Pts',(4.79899854265733,-10.4050714702017,17.0627039233768));
#48448=CARTESIAN_POINT('Ctrl Pts',(4.82390687063271,-10.3966071017749,17.0679970922034));
#48449=CARTESIAN_POINT('Ctrl Pts',(4.84034253976609,-10.3910064469563,17.0714996462197));
#48450=CARTESIAN_POINT('Ctrl Pts',(4.84682231416707,-10.3887937335801,17.0728835010604));
#48451=CARTESIAN_POINT('Ctrl Pts',(4.93413194828082,-10.3588749603406,17.0915962762918));
#48452=CARTESIAN_POINT('Ctrl Pts',(5.00656807785455,-10.3334060550506,17.1075365103738));
#48453=CARTESIAN_POINT('Ctrl Pts',(5.10746362109077,-10.2973256799759,17.1301368266871));
#48454=CARTESIAN_POINT('Ctrl Pts',(5.15597172992778,-10.2798130361603,17.1411114118487));
#48455=CARTESIAN_POINT('Ctrl Pts',(5.20917011370403,-10.2603647102356,17.1533071871831));
#48456=CARTESIAN_POINT('Ctrl Pts',(5.23124204749381,-10.252244452158,17.1584009613105));
#48457=CARTESIAN_POINT('Ctrl Pts',(5.24579503145523,-10.246879052893,17.1617669938564));
#48458=CARTESIAN_POINT('Ctrl Pts',(5.25192688210893,-10.2446143149913,17.1631879272938));
#48459=CARTESIAN_POINT('Ctrl Pts',(5.39096436493034,-10.1931327539252,17.1954922143067));
#48460=CARTESIAN_POINT('Ctrl Pts',(5.50204974451482,-10.1503044424321,17.2224360957622));
#48461=CARTESIAN_POINT('Ctrl Pts',(5.593361696325,-10.1144356126512,17.2450590603724));
#48462=CARTESIAN_POINT('',(-5.7364434626539,-10.2877335026487,16.9337808606147));
#48463=CARTESIAN_POINT('Origin',(-5.599999999997,-9.91330329093349,16.899368849389));
#48464=CARTESIAN_POINT('Ctrl Pts',(-5.73644387761981,-10.2877346861599,
16.933781035207));
#48465=CARTESIAN_POINT('Ctrl Pts',(-5.73644352459171,-10.2877348228402,
16.9337809477574));
#48466=CARTESIAN_POINT('Ctrl Pts',(-5.73644317156337,-10.2877349595205,
16.9337808603077));
#48467=CARTESIAN_POINT('Ctrl Pts',(-5.73644281853479,-10.287735096201,16.933780772858));
#48468=CARTESIAN_POINT('Ctrl Pts',(-5.67992342214019,-10.3096174512513,
16.9197801907616));
#48469=CARTESIAN_POINT('Ctrl Pts',(-5.61717135766351,-10.3335901883676,
16.9044748730959));
#48470=CARTESIAN_POINT('Ctrl Pts',(-5.54808404764097,-10.3594533564795,
16.8879873983964));
#48471=CARTESIAN_POINT('Ctrl Pts',(-5.52951893949722,-10.3664032943593,
16.8835568922627));
#48472=CARTESIAN_POINT('Ctrl Pts',(-5.51049626897038,-10.3734894845319,
16.8790411222862));
#48473=CARTESIAN_POINT('Ctrl Pts',(-5.49101384545753,-10.3807074712925,
16.8744426778672));
#48474=CARTESIAN_POINT('Ctrl Pts',(-5.42195250385916,-10.4062938080743,
16.858142101061));
#48475=CARTESIAN_POINT('Ctrl Pts',(-5.34711523904944,-10.4335394878555,
16.8408006378256));
#48476=CARTESIAN_POINT('Ctrl Pts',(-5.26639250305688,-10.4622194147446,
16.8225604772693));
#48477=CARTESIAN_POINT('Ctrl Pts',(-5.25084323281781,-10.4677439045695,
16.8190469543169));
#48478=CARTESIAN_POINT('Ctrl Pts',(-5.23507554015899,-10.473321484367,16.8155001622011));
#48479=CARTESIAN_POINT('Ctrl Pts',(-5.21908857950422,-10.4789503599815,
16.8119212284932));
#48480=CARTESIAN_POINT('Ctrl Pts',(-5.19131863628201,-10.4887279255611,
16.8057044879875));
#48481=CARTESIAN_POINT('Ctrl Pts',(-5.16288710415933,-10.4986602990195,
16.7993907444015));
#48482=CARTESIAN_POINT('Ctrl Pts',(-5.13378950707246,-10.5087375916594,
16.7929863248323));
#48483=CARTESIAN_POINT('Ctrl Pts',(-5.06602372686519,-10.5322067322924,
16.7780709870609));
#48484=CARTESIAN_POINT('Ctrl Pts',(-4.9946456086541,-10.5564631357043,16.7626630286108));
#48485=CARTESIAN_POINT('Ctrl Pts',(-4.91959547546881,-10.5813691667781,
16.7468506385375));
#48486=CARTESIAN_POINT('Ctrl Pts',(-4.82890430343498,-10.6114658108868,
16.7277428218351));
#48487=CARTESIAN_POINT('Ctrl Pts',(-4.73285110657451,-10.6425123616857,
16.7080435478597));
#48488=CARTESIAN_POINT('Ctrl Pts',(-4.63132572878703,-10.6742283680998,
16.6879338713862));
#48489=CARTESIAN_POINT('Ctrl Pts',(-4.61737858186911,-10.6785853851408,
16.6851712851407));
#48490=CARTESIAN_POINT('Ctrl Pts',(-4.60332815346294,-10.6829549696038,
16.6824009979981));
#48491=CARTESIAN_POINT('Ctrl Pts',(-4.58917414913846,-10.6873363297421,
16.679623522341));
#48492=CARTESIAN_POINT('Ctrl Pts',(-4.55699556861907,-10.6972971822869,
16.6733090390312));
#48493=CARTESIAN_POINT('Ctrl Pts',(-4.52428164451092,-10.7073189284579,
16.6669573814176));
#48494=CARTESIAN_POINT('Ctrl Pts',(-4.49102899371767,-10.7173919554314,
16.6605747653606));
#48495=CARTESIAN_POINT('Ctrl Pts',(-4.4506194813747,-10.729632967745,16.652818439288));
#48496=CARTESIAN_POINT('Ctrl Pts',(-4.40941439087031,-10.741949738429,16.6450163758549));
#48497=CARTESIAN_POINT('Ctrl Pts',(-4.36740760327574,-10.7543241258112,
16.6371803260442));
#48498=CARTESIAN_POINT('Ctrl Pts',(-4.34640420947845,-10.7605113195023,
16.6332623011389));
#48499=CARTESIAN_POINT('Ctrl Pts',(-4.32520038750531,-10.766712903505,16.6293357787708));
#48500=CARTESIAN_POINT('Ctrl Pts',(-4.30379537259903,-10.7729265138952,
16.6254023037402));
#48501=CARTESIAN_POINT('Ctrl Pts',(-4.29309286514589,-10.7760333190904,
16.6234355662249));
#48502=CARTESIAN_POINT('Ctrl Pts',(-4.28234005920634,-10.7791431299959,
16.6214670904874));
#48503=CARTESIAN_POINT('Ctrl Pts',(-4.27153685848547,-10.782255645371,16.6194970717074));
#48504=CARTESIAN_POINT('Ctrl Pts',(-4.26343445794482,-10.7845900319024,
16.6180195576223));
#48505=CARTESIAN_POINT('Ctrl Pts',(-4.25530371031925,-10.7869259396242,
16.6165411755713));
#48506=CARTESIAN_POINT('Ctrl Pts',(-4.24714457491206,-10.7892632399678,
16.6150620087903));
#48507=CARTESIAN_POINT('Ctrl Pts',(-4.24442486310967,-10.7900423400823,
16.6145689531966));
#48508=CARTESIAN_POINT('Ctrl Pts',(-4.24040522469893,-10.7911923588804,
16.6138411817243));
#48509=CARTESIAN_POINT('Ctrl Pts',(-4.23897597541557,-10.7916009996867,
16.6135825836003));
#48510=CARTESIAN_POINT('Ctrl Pts',(-4.2336371240715,-10.7931274461529,16.6126166100938));
#48511=CARTESIAN_POINT('Ctrl Pts',(-4.22827398300798,-10.7946579551636,
16.6116480535346));
#48512=CARTESIAN_POINT('Ctrl Pts',(-4.22288652589826,-10.7961924549587,
16.610676960236));
#48513=CARTESIAN_POINT('Ctrl Pts',(-4.14210580925051,-10.8192010823345,
16.5961161737666));
#48514=CARTESIAN_POINT('Ctrl Pts',(-4.05585859609673,-10.8431104347092,
16.5809827770254));
#48515=CARTESIAN_POINT('Ctrl Pts',(-3.96405497827556,-10.8676567011821,
16.5654470656392));
#48516=CARTESIAN_POINT('Ctrl Pts',(-3.91582512166372,-10.8805523031251,
16.5572852398822));
#48517=CARTESIAN_POINT('Ctrl Pts',(-3.86606160406621,-10.8936229969566,
16.5490128309054));
#48518=CARTESIAN_POINT('Ctrl Pts',(-3.81475097641875,-10.9068256811941,
16.5406577091471));
#48519=CARTESIAN_POINT('Ctrl Pts',(-3.71992040764233,-10.931226436223,16.5252160553442));
#48520=CARTESIAN_POINT('Ctrl Pts',(-3.61980520893666,-10.9560805656995,
16.5094902210422));
#48521=CARTESIAN_POINT('Ctrl Pts',(-3.51432294869463,-10.9810848930795,
16.4936763458349));
#48522=CARTESIAN_POINT('Ctrl Pts',(-3.46379932858498,-10.9930614011174,
16.4861018568013));
#48523=CARTESIAN_POINT('Ctrl Pts',(-3.41204441572844,-11.0050717436431,
16.4785075780106));
#48524=CARTESIAN_POINT('Ctrl Pts',(-3.3590493348187,-11.0170790331133,16.4709174043337));
#48525=CARTESIAN_POINT('Ctrl Pts',(-3.24837455319146,-11.0421550235115,
16.4550661064437));
#48526=CARTESIAN_POINT('Ctrl Pts',(-3.13229029342362,-11.0672207271769,
16.4392307259755));
#48527=CARTESIAN_POINT('Ctrl Pts',(-3.01072492044189,-11.091908246093,16.4236497593753));
#48528=CARTESIAN_POINT('Ctrl Pts',(-2.96856982425133,-11.1004691109929,
16.4182467640185));
#48529=CARTESIAN_POINT('Ctrl Pts',(-2.92501792022023,-11.1091301709932,
16.4127824523541));
#48530=CARTESIAN_POINT('Ctrl Pts',(-2.88137035979109,-11.1176132503999,
16.40743270236));
#48531=CARTESIAN_POINT('Ctrl Pts',(-2.87181730524371,-11.1194699250802,
16.4062618132426));
#48532=CARTESIAN_POINT('Ctrl Pts',(-2.86225971698664,-11.1213182353447,
16.4050963077141));
#48533=CARTESIAN_POINT('Ctrl Pts',(-2.85271131793043,-11.1231555396757,
16.4039378520687));
#48534=CARTESIAN_POINT('Ctrl Pts',(-2.83187965633902,-11.1271639710198,
16.4014104591695));
#48535=CARTESIAN_POINT('Ctrl Pts',(-2.81109169289071,-11.1311198674688,
16.3989167185575));
#48536=CARTESIAN_POINT('Ctrl Pts',(-2.79049042164608,-11.1349974785239,
16.3964728476892));
#48537=CARTESIAN_POINT('Ctrl Pts',(-2.6197081214259,-11.1671424528552,16.3762134237264));
#48538=CARTESIAN_POINT('Ctrl Pts',(-2.45358689126072,-11.1954600801453,
16.3583851565426));
#48539=CARTESIAN_POINT('Ctrl Pts',(-2.29236877426872,-11.2203892871839,
16.3427065217999));
#48540=CARTESIAN_POINT('Ctrl Pts',(-2.13001959335807,-11.2454933909842,
16.3269178898783));
#48541=CARTESIAN_POINT('Ctrl Pts',(-1.9726425728085,-11.2671622061084,16.313308628385));
#48542=CARTESIAN_POINT('Ctrl Pts',(-1.82044574964147,-11.2858528440568,
16.301585213352));
#48543=CARTESIAN_POINT('Ctrl Pts',(-1.76989122124497,-11.2920612284846,
16.2976910997572));
#48544=CARTESIAN_POINT('Ctrl Pts',(-1.71990782410642,-11.2979409267194,
16.2940051090325));
#48545=CARTESIAN_POINT('Ctrl Pts',(-1.67050197927261,-11.3035083877696,
16.2905166532439));
#48546=CARTESIAN_POINT('Ctrl Pts',(-1.52125898565814,-11.3203263281722,
16.279978880097));
#48547=CARTESIAN_POINT('Ctrl Pts',(-1.37728964501425,-11.3342968914911,
16.2712425364788));
#48548=CARTESIAN_POINT('Ctrl Pts',(-1.23874958120321,-11.3458747262349,
16.2640146511266));
#48549=CARTESIAN_POINT('Ctrl Pts',(-1.14911391351094,-11.3533656059064,
16.2593381964482));
#48550=CARTESIAN_POINT('Ctrl Pts',(-1.06175000190717,-11.3598544133719,
16.2552934670782));
#48551=CARTESIAN_POINT('Ctrl Pts',(-0.97669034347626,-11.3654588671785,
16.2518044106196));
#48552=CARTESIAN_POINT('Ctrl Pts',(-0.844793817754813,-11.374149332192,
16.246394155824));
#48553=CARTESIAN_POINT('Ctrl Pts',(-0.718439524656626,-11.3807153182433,
16.2423188713657));
#48554=CARTESIAN_POINT('Ctrl Pts',(-0.597721599451305,-11.3855832138007,
16.2393040884794));
#48555=CARTESIAN_POINT('Ctrl Pts',(-0.480995492516642,-11.3902901410976,
16.2363889963837));
#48556=CARTESIAN_POINT('Ctrl Pts',(-0.369538556420161,-11.3934093157848,
16.2344654664392));
#48557=CARTESIAN_POINT('Ctrl Pts',(-0.263406647333268,-11.3952954750715,
16.2333039464515));
#48558=CARTESIAN_POINT('Ctrl Pts',(-0.255824396465324,-11.3954302256193,
16.233220965414));
#48559=CARTESIAN_POINT('Ctrl Pts',(-0.248269313533065,-11.3955586699161,
16.2331418815967));
#48560=CARTESIAN_POINT('Ctrl Pts',(-0.240741414122083,-11.3956809312728,
16.2330666150223));
#48561=CARTESIAN_POINT('Ctrl Pts',(-0.202201236844007,-11.3963068660922,
16.2326812768341));
#48562=CARTESIAN_POINT('Ctrl Pts',(-0.16437359065513,-11.3967707924497,
16.2323959571174));
#48563=CARTESIAN_POINT('Ctrl Pts',(-0.127260292915424,-11.3970892300575,
16.2321998046146));
#48564=CARTESIAN_POINT('Ctrl Pts',(-0.105079047690209,-11.3972795484366,
16.2320825715194));
#48565=CARTESIAN_POINT('Ctrl Pts',(-0.0831529736488741,-11.3974178860524,
16.2319971868112));
#48566=CARTESIAN_POINT('Ctrl Pts',(-0.0614823788571396,-11.3975076611715,
16.2319414219955));
#48567=CARTESIAN_POINT('Ctrl Pts',(-0.0416874740895889,-11.3975896658395,
16.2318904838821));
#48568=CARTESIAN_POINT('Ctrl Pts',(-0.0231011596291624,-11.3976306161978,
16.2318646679704));
#48569=CARTESIAN_POINT('Ctrl Pts',(-0.00299587767511127,-11.3976346106805,
16.2318611125498));
#48570=CARTESIAN_POINT('Ctrl Pts',(-0.00109077748708527,-11.3976349891825,
16.2318607756517));
#48571=CARTESIAN_POINT('Ctrl Pts',(0.000827961144775839,-11.3976350036236,
16.2318606597262));
#48572=CARTESIAN_POINT('Ctrl Pts',(0.00276265878407632,-11.3976346367673,
16.2318607758997));
#48573=CARTESIAN_POINT('Ctrl Pts',(0.115384922859647,-11.3976132813997,
16.2318675385748));
#48574=CARTESIAN_POINT('Ctrl Pts',(0.233561096316357,-11.3963109193049,
16.2326602932816));
#48575=CARTESIAN_POINT('Ctrl Pts',(0.35723705049632,-11.3933310334508,16.2344974049638));
#48576=CARTESIAN_POINT('Ctrl Pts',(0.4006677928433,-11.3922846000062,16.2351425354151));
#48577=CARTESIAN_POINT('Ctrl Pts',(0.444776498966903,-11.3910309712916,
16.2359166635083));
#48578=CARTESIAN_POINT('Ctrl Pts',(0.489559944492275,-11.3895519147881,
16.2368316586877));
#48579=CARTESIAN_POINT('Ctrl Pts',(0.616826132084439,-11.3853487124614,
16.2394319040858));
#48580=CARTESIAN_POINT('Ctrl Pts',(0.749544200108315,-11.3793270294523,
16.2431685683526));
#48581=CARTESIAN_POINT('Ctrl Pts',(0.887615196589414,-11.3710593224922,
16.2483172112831));
#48582=CARTESIAN_POINT('Ctrl Pts',(0.982140754091479,-11.3653991213669,
16.25184205253));
#48583=CARTESIAN_POINT('Ctrl Pts',(1.07917451717098,-11.3586855955954,16.2560290586568));
#48584=CARTESIAN_POINT('Ctrl Pts',(1.1786736826074,-11.3507739191701,16.260971147143));
#48585=CARTESIAN_POINT('Ctrl Pts',(1.32346414485075,-11.3392609051491,16.2681628383822));
#48586=CARTESIAN_POINT('Ctrl Pts',(1.47347738408703,-11.3252111773464,16.2769531843729));
#48587=CARTESIAN_POINT('Ctrl Pts',(1.62855152014101,-11.3081749134555,16.2876319525441));
#48588=CARTESIAN_POINT('Ctrl Pts',(1.68651040446399,-11.3018076179588,16.2916231370505));
#48589=CARTESIAN_POINT('Ctrl Pts',(1.74517577213395,-11.2950229558544,16.2958782200467));
#48590=CARTESIAN_POINT('Ctrl Pts',(1.80453741563049,-11.2877968278436,16.3004126889885));
#48591=CARTESIAN_POINT('Ctrl Pts',(1.96227499440047,-11.2685953389839,16.3124618188603));
#48592=CARTESIAN_POINT('Ctrl Pts',(2.12493249599591,-11.2462771144358,16.3264834789877));
#48593=CARTESIAN_POINT('Ctrl Pts',(2.29229484978981,-11.2203986250669,16.3427622938076));
#48594=CARTESIAN_POINT('Ctrl Pts',(2.31267645412228,-11.2172471090953,16.3447447489723));
#48595=CARTESIAN_POINT('Ctrl Pts',(2.33312777143621,-11.2140427844923,16.3467606826937));
#48596=CARTESIAN_POINT('Ctrl Pts',(2.35364835962339,-11.2107848446272,16.3488106114143));
#48597=CARTESIAN_POINT('Ctrl Pts',(2.36243285324297,-11.209390179343,16.3496881489197));
#48598=CARTESIAN_POINT('Ctrl Pts',(2.37123004088339,-11.2079856888241,16.3505719161559));
#48599=CARTESIAN_POINT('Ctrl Pts',(2.38003988911401,-11.2065713117456,16.3514619524672));
#48600=CARTESIAN_POINT('Ctrl Pts',(2.44797664373784,-11.195664405518,16.3583254280799));
#48601=CARTESIAN_POINT('Ctrl Pts',(2.51666639180399,-11.1841695738006,16.3655617099716));
#48602=CARTESIAN_POINT('Ctrl Pts',(2.5860930260163,-11.1720587322928,16.3731888014931));
#48603=CARTESIAN_POINT('Ctrl Pts',(2.62080634312245,-11.1660033115389,16.3770023472539));
#48604=CARTESIAN_POINT('Ctrl Pts',(2.65570388132704,-11.1597938857993,16.3809135953313));
#48605=CARTESIAN_POINT('Ctrl Pts',(2.6907834711816,-11.1534269579017,16.3849247863288));
#48606=CARTESIAN_POINT('Ctrl Pts',(2.70832326610889,-11.1502434939528,16.3869303818276));
#48607=CARTESIAN_POINT('Ctrl Pts',(2.72590857392964,-11.147020654347,16.3889609630524));
#48608=CARTESIAN_POINT('Ctrl Pts',(2.74353911819219,-11.1437580021669,16.3910168095262));
#48609=CARTESIAN_POINT('Ctrl Pts',(2.75886397947236,-11.1409220323114,16.3928037970154));
#48610=CARTESIAN_POINT('Ctrl Pts',(2.77564172384628,-11.1377895682063,16.3947777552928));
#48611=CARTESIAN_POINT('Ctrl Pts',(2.79017260044529,-11.1350548322832,16.3965012236886));
#48612=CARTESIAN_POINT('Ctrl Pts',(2.79235882544797,-11.1346433809843,16.3967605259869));
#48613=CARTESIAN_POINT('Ctrl Pts',(2.79449421169261,-11.13424101261,16.3970141065111));
#48614=CARTESIAN_POINT('Ctrl Pts',(2.79656618101408,-11.1338501710236,16.3972604239752));
#48615=CARTESIAN_POINT('Ctrl Pts',(2.81155319855809,-11.1310231264086,16.3990420932875));
#48616=CARTESIAN_POINT('Ctrl Pts',(2.82653415511714,-11.128174494239,16.4008376888312));
#48617=CARTESIAN_POINT('Ctrl Pts',(2.84150896902975,-11.125304341067,16.4026471655719));
#48618=CARTESIAN_POINT('Ctrl Pts',(2.9877609092892,-11.0972729095777,16.4203194709324));
#48619=CARTESIAN_POINT('Ctrl Pts',(3.13342693458816,-11.0671887043866,16.4393158344591));
#48620=CARTESIAN_POINT('Ctrl Pts',(3.27844000038263,-11.0351204092031,16.4595900055763));
#48621=CARTESIAN_POINT('Ctrl Pts',(3.40983090074459,-11.0060645296232,16.4779596716652));
#48622=CARTESIAN_POINT('Ctrl Pts',(3.54068575419653,-10.9753798121356,16.4973783531426));
#48623=CARTESIAN_POINT('Ctrl Pts',(3.67096096203933,-10.9431207808494,16.5178092758489));
#48624=CARTESIAN_POINT('Ctrl Pts',(3.78813583454779,-10.9141056831896,16.5361856868558));
#48625=CARTESIAN_POINT('Ctrl Pts',(3.90484177689973,-10.8838169747423,16.5553809953117));
#48626=CARTESIAN_POINT('Ctrl Pts',(4.02105135355173,-10.8522959606735,16.5753671327589));
#48627=CARTESIAN_POINT('Ctrl Pts',(4.12469412582962,-10.8241836021467,16.593191986371));
#48628=CARTESIAN_POINT('Ctrl Pts',(4.2279420807947,-10.7950910485532,16.6116458779085));
#48629=CARTESIAN_POINT('Ctrl Pts',(4.33077854876954,-10.7650482812465,16.6307081883437));
#48630=CARTESIAN_POINT('Ctrl Pts',(4.4224084153124,-10.7382794237283,16.6476931839933));
#48631=CARTESIAN_POINT('Ctrl Pts',(4.51371159158894,-10.7107561676242,16.6651612189951));
#48632=CARTESIAN_POINT('Ctrl Pts',(4.60467809233216,-10.6824999484507,16.6830973369985));
#48633=CARTESIAN_POINT('Ctrl Pts',(4.68609873252078,-10.6572088859648,16.6991512711214));
#48634=CARTESIAN_POINT('Ctrl Pts',(4.76724964968438,-10.6313306211052,16.7155802031916));
#48635=CARTESIAN_POINT('Ctrl Pts',(4.84812490671061,-10.6048805365343,16.7323732809376));
#48636=CARTESIAN_POINT('Ctrl Pts',(4.92104763596778,-10.5810313096271,16.7475150821126));
#48637=CARTESIAN_POINT('Ctrl Pts',(4.99374625116398,-10.5567171895405,16.7629529363442));
#48638=CARTESIAN_POINT('Ctrl Pts',(5.06621727472414,-10.531949354954,16.7786790259285));
#48639=CARTESIAN_POINT('Ctrl Pts',(5.13211670113978,-10.5094274418827,16.7929790900432));
#48640=CARTESIAN_POINT('Ctrl Pts',(5.19782793957924,-10.4865303686829,16.8075174857058));
#48641=CARTESIAN_POINT('Ctrl Pts',(5.26334901114175,-10.4632663744166,16.8222888789691));
#48642=CARTESIAN_POINT('Ctrl Pts',(5.32293003021169,-10.4421114626764,16.8357211175256));
#48643=CARTESIAN_POINT('Ctrl Pts',(5.38235379937692,-10.420653143382,16.8493460220469));
#48644=CARTESIAN_POINT('Ctrl Pts',(5.44161920194577,-10.398897403341,16.8631608536372));
#48645=CARTESIAN_POINT('Ctrl Pts',(5.49538550613805,-10.3791603276397,16.8756938392485));
#48646=CARTESIAN_POINT('Ctrl Pts',(5.54902146846579,-10.3591784639908,16.8883831411604));
#48647=CARTESIAN_POINT('Ctrl Pts',(5.60252622810342,-10.3389560486812,16.9012292544107));
#48648=CARTESIAN_POINT('Ctrl Pts',(5.64725725918507,-10.3220497118639,16.9119688576716));
#48649=CARTESIAN_POINT('Ctrl Pts',(5.6918965888703,-10.3049752448851,16.9228180609114));
#48650=CARTESIAN_POINT('Ctrl Pts',(5.73644276371282,-10.2877350949215,16.9337809951188));
#48651=CARTESIAN_POINT('Ctrl Pts',(-5.843530256039,-10.2251619023962,17.1593086092344));
#48652=CARTESIAN_POINT('Ctrl Pts',(-3.89568683736,-11.0033634786087,16.6619375925682));
#48653=CARTESIAN_POINT('Ctrl Pts',(0.0001633689883933,-11.7816837467847,
16.1645405511091));
#48654=CARTESIAN_POINT('Ctrl Pts',(3.896013575336,-11.0032981995481,16.6619793101207));
#48655=CARTESIAN_POINT('Ctrl Pts',(5.844020363005,-10.2249660868567,17.1594337605745));
#48656=CARTESIAN_POINT('Ctrl Pts',(-5.843530256039,-10.3258757279616,16.2770651088131));
#48657=CARTESIAN_POINT('Ctrl Pts',(-3.89568683736,-11.0553894883161,15.8346835239237));
#48658=CARTESIAN_POINT('Ctrl Pts',(0.0001633689883933,-11.7876690390135,
15.3921195066591));
#48659=CARTESIAN_POINT('Ctrl Pts',(3.896013575336,-11.0553280707653,15.8347206425293));
#48660=CARTESIAN_POINT('Ctrl Pts',(5.844020363005,-10.3256921635601,16.2771764234008));
#48661=CARTESIAN_POINT('Ctrl Pts',(-5.843530256039,-10.2973078611637,14.4766625890132));
#48662=CARTESIAN_POINT('Ctrl Pts',(-3.89568683736,-10.9728033087721,14.1582357115413));
#48663=CARTESIAN_POINT('Ctrl Pts',(0.0001633689883933,-11.6469739445733,
13.839942885095));
#48664=CARTESIAN_POINT('Ctrl Pts',(3.896013575336,-10.9727467649199,14.1582624073125));
#48665=CARTESIAN_POINT('Ctrl Pts',(5.844020363005,-10.2971378891111,14.4767427134021));
#48666=CARTESIAN_POINT('Ctrl Pts',(-5.843530256039,-9.55783041482319,11.8732201296673));
#48667=CARTESIAN_POINT('Ctrl Pts',(-3.89568683736,-10.276390078785,11.7328262507184));
#48668=CARTESIAN_POINT('Ctrl Pts',(0.0001633689883934,-10.9955719605932,
11.592156207881));
#48669=CARTESIAN_POINT('Ctrl Pts',(3.896013575336,-10.2763297597585,11.7328380489558));
#48670=CARTESIAN_POINT('Ctrl Pts',(5.844020363005,-9.55764960672994,11.8732554563753));
#48671=CARTESIAN_POINT('Ctrl Pts',(-5.843530256039,-8.22112111690873,9.63761418987316));
#48672=CARTESIAN_POINT('Ctrl Pts',(-3.89568683736,-9.09193883951927,9.6131438962805));
#48673=CARTESIAN_POINT('Ctrl Pts',(0.0001633689883931,-9.96185017516567,
9.58955563129661));
#48674=CARTESIAN_POINT('Ctrl Pts',(3.896013575336,-9.09186587855354,9.61314587466688));
#48675=CARTESIAN_POINT('Ctrl Pts',(5.844020363005,-8.22090199675714,9.63762034723964));
#48676=CARTESIAN_POINT('Ctrl Pts',(-5.843530256039,-7.02222755551629,8.43824701706476));
#48677=CARTESIAN_POINT('Ctrl Pts',(-3.89568683736,-8.04148396885872,8.43232683562214));
#48678=CARTESIAN_POINT('Ctrl Pts',(0.0001633689883938,-9.06239246807137,
8.42475648328517));
#48679=CARTESIAN_POINT('Ctrl Pts',(3.896013575336,-8.04139834349921,8.43232747055704));
#48680=CARTESIAN_POINT('Ctrl Pts',(5.844020363005,-7.02197108439241,8.43824850671153));
#48681=CARTESIAN_POINT('Ctrl Pts',(-5.843530256039,-6.40569322596623,7.94881077194426));
#48682=CARTESIAN_POINT('Ctrl Pts',(-3.89568683736,-7.50133620017675,7.9347606008931));
#48683=CARTESIAN_POINT('Ctrl Pts',(0.0001633689883938,-8.59759863808049,
7.92012362694403));
#48684=CARTESIAN_POINT('Ctrl Pts',(3.896013575336,-7.50124425475692,7.93476182852443));
#48685=CARTESIAN_POINT('Ctrl Pts',(5.844020363005,-6.4054175340111,7.94881430732273));
#48686=CARTESIAN_POINT('',(-5.73278765503808,-6.65588329694249,8.10254693662637));
#48687=CARTESIAN_POINT('Ctrl Pts',(-5.73644356953866,-10.287732124489,16.9337807348462));
#48688=CARTESIAN_POINT('Ctrl Pts',(-5.73766037023391,-10.363335737503,16.106357439364));
#48689=CARTESIAN_POINT('Ctrl Pts',(-5.73849618481051,-10.3386824467405,
15.2703428493243));
#48690=CARTESIAN_POINT('Ctrl Pts',(-5.73940756698809,-10.0903333051297,
13.6301040301155));
#48691=CARTESIAN_POINT('Ctrl Pts',(-5.73948313452165,-9.86673834734387,
12.8258710001043));
#48692=CARTESIAN_POINT('Ctrl Pts',(-5.73887402243792,-9.23545641682537,
11.2957057506713));
#48693=CARTESIAN_POINT('Ctrl Pts',(-5.73818934282062,-8.8274551097991,10.5699144763157));
#48694=CARTESIAN_POINT('Ctrl Pts',(-5.73605973643519,-7.85267850870576,
9.23785247231672));
#48695=CARTESIAN_POINT('Ctrl Pts',(-5.73461480966704,-7.28539109135887,
8.63201129368857));
#48696=CARTESIAN_POINT('Ctrl Pts',(-5.732787802167,-6.65588356458119,8.10254661754625));
#48697=CARTESIAN_POINT('Ctrl Pts',(5.73278688077132,-6.65588777852224,8.1025415711865));
#48698=CARTESIAN_POINT('Ctrl Pts',(5.37827627368246,-6.85241150406531,8.10465963825173));
#48699=CARTESIAN_POINT('Ctrl Pts',(5.01472560063427,-7.03192684229805,8.10373394496733));
#48700=CARTESIAN_POINT('Ctrl Pts',(4.64373673482061,-7.19313127670242,8.10099337416535));
#48701=CARTESIAN_POINT('Ctrl Pts',(4.36982161608589,-7.31215461098387,8.09896990703251));
#48702=CARTESIAN_POINT('Ctrl Pts',(4.09185162034693,-7.42119223737612,8.09595885654005));
#48703=CARTESIAN_POINT('Ctrl Pts',(3.81047150082134,-7.5197407633679,8.09246831279417));
#48704=CARTESIAN_POINT('Ctrl Pts',(3.56966521041932,-7.60407900662645,8.08948109076744));
#48705=CARTESIAN_POINT('Ctrl Pts',(3.32636134248185,-7.68073414882858,8.08614294160563));
#48706=CARTESIAN_POINT('Ctrl Pts',(3.08096402298937,-7.74943065949521,8.08277474483814));
#48707=CARTESIAN_POINT('Ctrl Pts',(3.03961664418193,-7.76100544219926,8.08220723208808));
#48708=CARTESIAN_POINT('Ctrl Pts',(2.99820983352411,-7.77235440392396,8.08163886854269));
#48709=CARTESIAN_POINT('Ctrl Pts',(2.95674552410237,-7.78347638387023,8.08107119111927));
#48710=CARTESIAN_POINT('Ctrl Pts',(2.75869139757556,-7.83660048153941,8.07835968192469));
#48711=CARTESIAN_POINT('Ctrl Pts',(2.55931825461576,-7.88459121383307,8.07570997194223));
#48712=CARTESIAN_POINT('Ctrl Pts',(2.3588932505288,-7.92725022184157,8.07321176886139));
#48713=CARTESIAN_POINT('Ctrl Pts',(2.16496913216616,-7.96852556348848,8.07079459625286));
#48714=CARTESIAN_POINT('Ctrl Pts',(1.97006028134188,-8.00480937407901,8.06851927227267));
#48715=CARTESIAN_POINT('Ctrl Pts',(1.77440869148724,-8.03597039260338,8.06646657500283));
#48716=CARTESIAN_POINT('Ctrl Pts',(1.58213144846987,-8.06659398598143,8.06444928001388));
#48717=CARTESIAN_POINT('Ctrl Pts',(1.38913686510899,-8.09226981697469,8.06264700825244));
#48718=CARTESIAN_POINT('Ctrl Pts',(1.19565462876281,-8.11292263500189,8.06113580896464));
#48719=CARTESIAN_POINT('Ctrl Pts',(0.997079151827903,-8.1341191193265,8.05958482875588));
#48720=CARTESIAN_POINT('Ctrl Pts',(0.797990009959274,-8.15002411796531,
8.05834046071093));
#48721=CARTESIAN_POINT('Ctrl Pts',(0.598635511115839,-8.16061444565142,
8.05748407636205));
#48722=CARTESIAN_POINT('Ctrl Pts',(0.41011089037405,-8.17062945671029,8.05667421485644));
#48723=CARTESIAN_POINT('Ctrl Pts',(0.221348960431186,-8.17589182255372,
8.05621132523823));
#48724=CARTESIAN_POINT('Ctrl Pts',(0.0325597200542654,-8.17643387335583,
8.05616342086763));
#48725=CARTESIAN_POINT('Ctrl Pts',(0.0217146407636161,-8.17646501169781,
8.05616066898041));
#48726=CARTESIAN_POINT('Ctrl Pts',(0.010869471349147,-8.17648058744749,
8.05615928631154));
#48727=CARTESIAN_POINT('Ctrl Pts',(2.42516200383473E-5,-8.17648061201097,
8.05615928567218));
#48728=CARTESIAN_POINT('Ctrl Pts',(1.61677462454062E-5,-8.17648061202928,
8.0561592856717));
#48729=CARTESIAN_POINT('Ctrl Pts',(8.08387248017682E-6,-8.17648061203894,
8.05615928567199));
#48730=CARTESIAN_POINT('Ctrl Pts',(-1.25747418398594E-12,-8.17648061203997,
8.05615928567305));
#48731=CARTESIAN_POINT('Ctrl Pts',(-0.189139035705872,-8.17648063611191,
8.0561593104538));
#48732=CARTESIAN_POINT('Ctrl Pts',(-0.378262933363979,-8.17174639869451,
8.05657974522599));
#48733=CARTESIAN_POINT('Ctrl Pts',(-0.567160529186507,-8.16224240278298,
8.05735224853584));
#48734=CARTESIAN_POINT('Ctrl Pts',(-0.75860062666825,-8.15261048610428,
8.05813514949495));
#48735=CARTESIAN_POINT('Ctrl Pts',(-0.949808289415187,-8.13807964420742,
8.05927965741794));
#48736=CARTESIAN_POINT('Ctrl Pts',(-1.14056371176547,-8.11866645037277,
8.06071380372489));
#48737=CARTESIAN_POINT('Ctrl Pts',(-1.33594378375974,-8.09878260559227,
8.06218271928834));
#48738=CARTESIAN_POINT('Ctrl Pts',(-1.53084942143149,-8.07377685544065,
8.06395548156749));
#48739=CARTESIAN_POINT('Ctrl Pts',(-1.72504444158472,-8.04372179853256,
8.06595395922777));
#48740=CARTESIAN_POINT('Ctrl Pts',(-1.93232436125451,-8.01164162584501,
8.06808709471475));
#48741=CARTESIAN_POINT('Ctrl Pts',(-2.13879467403457,-7.97380847538887,
8.07047738209557));
#48742=CARTESIAN_POINT('Ctrl Pts',(-2.34416816538383,-7.93037483013253,
8.07302899030251));
#48743=CARTESIAN_POINT('Ctrl Pts',(-2.5495416567331,-7.8869411848762,8.07558059850945));
#48744=CARTESIAN_POINT('Ctrl Pts',(-2.75381832665157,-7.83790747751988,
8.07829351057817));
#48745=CARTESIAN_POINT('Ctrl Pts',(-2.9567109605982,-7.78348624499325,8.08107129305309));
#48746=CARTESIAN_POINT('Ctrl Pts',(-3.20112609626292,-7.7179275666307,8.08441755588802));
#48747=CARTESIAN_POINT('Ctrl Pts',(-3.44354367002378,-7.64447761155163,
8.08778762182236));
#48748=CARTESIAN_POINT('Ctrl Pts',(-3.68356773262446,-7.56339748666701,
8.09086695035259));
#48749=CARTESIAN_POINT('Ctrl Pts',(-3.97268664594418,-7.46573312191761,
8.09457612896065));
#48750=CARTESIAN_POINT('Ctrl Pts',(-4.25833276625898,-7.35699881171472,
8.09786311779884));
#48751=CARTESIAN_POINT('Ctrl Pts',(-4.53981409580119,-7.23772737140737,
8.10018171708692));
#48752=CARTESIAN_POINT('Ctrl Pts',(-4.90286922679157,-7.08389085068814,
8.10317225066729));
#48753=CARTESIAN_POINT('Ctrl Pts',(-5.25899585877525,-6.91253101039286,
8.10454919088797));
#48754=CARTESIAN_POINT('Ctrl Pts',(-5.60670917229762,-6.72485657966638,
8.10316803578398));
#48755=CARTESIAN_POINT('Ctrl Pts',(-5.64886055313031,-6.70210583618183,
8.10300060591427));
#48756=CARTESIAN_POINT('Ctrl Pts',(-5.69088829700777,-6.6791153198583,8.10279270682702));
#48757=CARTESIAN_POINT('Ctrl Pts',(-5.73278975881162,-6.65588714129348,
8.10254235866335));
#48758=CARTESIAN_POINT('Ctrl Pts',(5.84532977015488,-6.60907067653791,8.11484374494995));
#48759=CARTESIAN_POINT('Ctrl Pts',(5.67447011930324,-6.70782274026614,8.11771294877927));
#48760=CARTESIAN_POINT('Ctrl Pts',(5.16429345659284,-6.98693741106745,8.12376642310323));
#48761=CARTESIAN_POINT('Ctrl Pts',(4.24590849141901,-7.40895819124323,8.12400293957608));
#48762=CARTESIAN_POINT('Ctrl Pts',(3.01583524949797,-7.83057380116843,8.11342583655146));
#48763=CARTESIAN_POINT('Ctrl Pts',(1.5827416161131,-8.13989354095393,8.09845002215385));
#48764=CARTESIAN_POINT('Ctrl Pts',(-0.000549049248834099,-8.25797507006647,
8.09084489616248));
#48765=CARTESIAN_POINT('Ctrl Pts',(-1.58374029028414,-8.13974006353747,
8.09845910700112));
#48766=CARTESIAN_POINT('Ctrl Pts',(-3.01660487844852,-7.83035051488068,
8.11343402782235));
#48767=CARTESIAN_POINT('Ctrl Pts',(-4.24645128469797,-7.40873441263074,
8.1240053767904));
#48768=CARTESIAN_POINT('Ctrl Pts',(-5.16457961062395,-6.98678753483177,
8.12376410532789));
#48769=CARTESIAN_POINT('Ctrl Pts',(-5.67458005472615,-6.70775903594086,
8.11771107859869));
#48770=CARTESIAN_POINT('Ctrl Pts',(-5.84532137971053,-6.60907553644657,
8.11484388868645));
#48771=CARTESIAN_POINT('Ctrl Pts',(5.72603251848978,-6.40553651593773,7.90654864603447));
#48772=CARTESIAN_POINT('Ctrl Pts',(5.55862522162997,-6.50183163678554,7.90984134163062));
#48773=CARTESIAN_POINT('Ctrl Pts',(5.0587624490829,-6.77403023907758,7.91713060303473));
#48774=CARTESIAN_POINT('Ctrl Pts',(4.15898620617447,-7.18569021983348,7.9194064566943));
#48775=CARTESIAN_POINT('Ctrl Pts',(2.95395178893228,-7.59702783009949,7.91108135352791));
#48776=CARTESIAN_POINT('Ctrl Pts',(1.55019345539187,-7.89883073461615,7.89790735180303));
#48777=CARTESIAN_POINT('Ctrl Pts',(-0.000537746227424225,-8.01404387038147,
7.89103083637919));
#48778=CARTESIAN_POINT('Ctrl Pts',(-1.55117163467799,-7.89868098502473,
7.89791550720898));
#48779=CARTESIAN_POINT('Ctrl Pts',(-2.95470571498482,-7.59680997565968,
7.9110882992896));
#48780=CARTESIAN_POINT('Ctrl Pts',(-4.15951798303049,-7.18547191412746,
7.91940776248282));
#48781=CARTESIAN_POINT('Ctrl Pts',(-5.05904281585884,-6.773884064197,7.91712760404102));
#48782=CARTESIAN_POINT('Ctrl Pts',(-5.55873293575348,-6.5017695177983,7.90983919864932));
#48783=CARTESIAN_POINT('Ctrl Pts',(-5.72602429756767,-6.40554125490832,
7.90654881060056));
#48784=CARTESIAN_POINT('Ctrl Pts',(5.72051931939661,-6.40299635313841,7.59202739925403));
#48785=CARTESIAN_POINT('Ctrl Pts',(5.55358754504462,-6.49829579986879,7.59531976312339));
#48786=CARTESIAN_POINT('Ctrl Pts',(5.05509604406011,-6.76774980134388,7.60262461997097));
#48787=CARTESIAN_POINT('Ctrl Pts',(4.15740464799149,-7.17560639151535,7.60498214643902));
#48788=CARTESIAN_POINT('Ctrl Pts',(2.95412552499078,-7.58366289837459,7.59678147557994));
#48789=CARTESIAN_POINT('Ctrl Pts',(1.5509282484579,-7.88347759639777,7.58370271852113));
#48790=CARTESIAN_POINT('Ctrl Pts',(-0.000538111079215552,-7.99805888798782,
7.57685722966631));
#48791=CARTESIAN_POINT('Ctrl Pts',(-1.55190650864731,-7.88332872496391,
7.58371083015612));
#48792=CARTESIAN_POINT('Ctrl Pts',(-2.95487868487001,-7.58344664067807,
7.59678835073835));
#48793=CARTESIAN_POINT('Ctrl Pts',(-4.15793535657866,-7.17538998909926,
7.60498339567978));
#48794=CARTESIAN_POINT('Ctrl Pts',(-5.05537566230955,-6.76760506823289,
7.60262160571017));
#48795=CARTESIAN_POINT('Ctrl Pts',(-5.55369495290555,-6.49823432383111,
7.59531762036264));
#48796=CARTESIAN_POINT('Ctrl Pts',(-5.72051112194647,-6.40300104308615,
7.592027563499));
#48797=CARTESIAN_POINT('Ctrl Pts',(5.83215265165326,-6.6027019454344,7.37631534334889));
#48798=CARTESIAN_POINT('Ctrl Pts',(5.66241585886446,-6.69911246418964,7.37918461663417));
#48799=CARTESIAN_POINT('Ctrl Pts',(5.1554779165898,-6.97177232001094,7.38527716439616));
#48800=CARTESIAN_POINT('Ctrl Pts',(4.24202288280943,-7.38484664402246,7.38570943211202));
#48801=CARTESIAN_POINT('Ctrl Pts',(3.01611906064791,-7.79874165528961,7.37542885317601));
#48802=CARTESIAN_POINT('Ctrl Pts',(1.5844008409398,-8.10338046623929,7.36068016455236));
#48803=CARTESIAN_POINT('Ctrl Pts',(-0.000549882842812274,-8.21997345439349,
7.35314930988947));
#48804=CARTESIAN_POINT('Ctrl Pts',(-1.58539966393749,-8.10322905712485,
7.3606891448144));
#48805=CARTESIAN_POINT('Ctrl Pts',(-3.01688686011958,-7.79852212707958,
7.375436876266));
#48806=CARTESIAN_POINT('Ctrl Pts',(-4.24256314704044,-7.38462734296759,
7.38571173436092));
#48807=CARTESIAN_POINT('Ctrl Pts',(-5.15576230240762,-6.97162583470661,
7.38527480944027));
#48808=CARTESIAN_POINT('Ctrl Pts',(-5.66252507110996,-6.69905027190079,
7.37918274642969));
#48809=CARTESIAN_POINT('Ctrl Pts',(-5.83214431663215,-6.60270669005865,
7.37631548637498));
#48810=CARTESIAN_POINT('',(-5.72001858724455,-6.64700966239077,7.39409314559782));
#48811=CARTESIAN_POINT('Origin',(-5.89877641407823,-6.95919970879477,7.74135818432323));
#48812=CARTESIAN_POINT('Ctrl Pts',(5.72001587221878,-6.64701148325172,7.39409251600456));
#48813=CARTESIAN_POINT('Ctrl Pts',(5.58565290454697,-6.72168733592391,7.39612364502573));
#48814=CARTESIAN_POINT('Ctrl Pts',(5.44860854991134,-6.79466770029646,7.39767007526861));
#48815=CARTESIAN_POINT('Ctrl Pts',(5.30887161640016,-6.86572132858295,7.39878665706021));
#48816=CARTESIAN_POINT('Ctrl Pts',(5.1302758002585,-6.95653397499499,7.40021374459784));
#48817=CARTESIAN_POINT('Ctrl Pts',(4.94728058316614,-7.04420061915497,7.40093782687921));
#48818=CARTESIAN_POINT('Ctrl Pts',(4.75989538421007,-7.12819823960006,7.40110494294509));
#48819=CARTESIAN_POINT('Ctrl Pts',(4.70375696841375,-7.15336294507689,7.40115500896548));
#48820=CARTESIAN_POINT('Ctrl Pts',(4.64722472964256,-7.17819808859506,7.40115523439491));
#48821=CARTESIAN_POINT('Ctrl Pts',(4.59029942585008,-7.20268894371145,7.40110993482223));
#48822=CARTESIAN_POINT('Ctrl Pts',(4.48483666528044,-7.24806196795919,7.40102601049213));
#48823=CARTESIAN_POINT('Ctrl Pts',(4.37802534628683,-7.29225649954224,7.4007825429084));
#48824=CARTESIAN_POINT('Ctrl Pts',(4.26987188704354,-7.33518654413751,7.40039822446667));
#48825=CARTESIAN_POINT('Ctrl Pts',(4.17517571350464,-7.37277490221194,7.40006172588302));
#48826=CARTESIAN_POINT('Ctrl Pts',(4.07945062248494,-7.40939381534365,7.39961727421961));
#48827=CARTESIAN_POINT('Ctrl Pts',(3.98270573857866,-7.4449835306767,7.39907881998807));
#48828=CARTESIAN_POINT('Ctrl Pts',(3.87908664057,-7.48310207557843,7.39850210585561));
#48829=CARTESIAN_POINT('Ctrl Pts',(3.77429690775606,-7.52004090555753,7.3978169305443));
#48830=CARTESIAN_POINT('Ctrl Pts',(3.66834908493288,-7.555728786703,7.39703672613765));
#48831=CARTESIAN_POINT('Ctrl Pts',(3.61537517352129,-7.57357272727574,7.39664662393433));
#48832=CARTESIAN_POINT('Ctrl Pts',(3.56211173626585,-7.59110392169548,7.39623275554249));
#48833=CARTESIAN_POINT('Ctrl Pts',(3.5085606927734,-7.60831352101272,7.39579651070001));
#48834=CARTESIAN_POINT('Ctrl Pts',(3.48178517102717,-7.61691832067135,7.39557838827878));
#48835=CARTESIAN_POINT('Ctrl Pts',(3.45493774755442,-7.6254427209945,7.39535467120603));
#48836=CARTESIAN_POINT('Ctrl Pts',(3.42801867261478,-7.63388561714074,7.39512552136858));
#48837=CARTESIAN_POINT('Ctrl Pts',(3.41455913514496,-7.63810706521386,7.39501094644986));
#48838=CARTESIAN_POINT('Ctrl Pts',(3.40108168479896,-7.64230813720522,7.39489501330451));
#48839=CARTESIAN_POINT('Ctrl Pts',(3.38758635409509,-7.64648869523428,7.39477774108775));
#48840=CARTESIAN_POINT('Ctrl Pts',(3.38083868874316,-7.64857897424881,7.39471910497938));
#48841=CARTESIAN_POINT('Ctrl Pts',(3.37408655330122,-7.65066412477043,7.39466013410096));
#48842=CARTESIAN_POINT('Ctrl Pts',(3.3673299519168,-7.65274412958196,7.39460083077426));
#48843=CARTESIAN_POINT('Ctrl Pts',(3.36057335053239,-7.65482413439349,7.39454152744755));
#48844=CARTESIAN_POINT('Ctrl Pts',(3.35536610976867,-7.65642365019241,7.39449566394423));
#48845=CARTESIAN_POINT('Ctrl Pts',(3.34704675410775,-7.65896868966984,7.39442192574389));
#48846=CARTESIAN_POINT('Ctrl Pts',(3.25218527717916,-7.68798850965474,7.39358112570173));
#48847=CARTESIAN_POINT('Ctrl Pts',(3.15684396878774,-7.71584499185392,7.39270673831623));
#48848=CARTESIAN_POINT('Ctrl Pts',(3.06103807353292,-7.7425135289854,7.39181551956672));
#48849=CARTESIAN_POINT('Ctrl Pts',(2.81798286979236,-7.81017039611988,7.38955453808784));
#48850=CARTESIAN_POINT('Ctrl Pts',(2.57193719390984,-7.87018487448976,7.3871846311959));
#48851=CARTESIAN_POINT('Ctrl Pts',(2.32323865480377,-7.9221824209829,7.38493236667366));
#48852=CARTESIAN_POINT('Ctrl Pts',(2.09715323564706,-7.96945204764125,7.38288489116218));
#48853=CARTESIAN_POINT('Ctrl Pts',(1.86887526640671,-8.01009597774375,7.38093460284897));
#48854=CARTESIAN_POINT('Ctrl Pts',(1.63866316117177,-8.04379642976548,7.37925911418169));
#48855=CARTESIAN_POINT('Ctrl Pts',(1.3874922641473,-8.08056501218121,7.3774310869757));
#48856=CARTESIAN_POINT('Ctrl Pts',(1.1340181123422,-8.10906858519484,7.3759304349394));
#48857=CARTESIAN_POINT('Ctrl Pts',(0.878690129281667,-8.12901172996105,
7.37484825163557));
#48858=CARTESIAN_POINT('Ctrl Pts',(0.631087833523658,-8.14835143714692,
7.37379881292052));
#48859=CARTESIAN_POINT('Ctrl Pts',(0.381741838955915,-8.15964088646107,
7.37314282965446));
#48860=CARTESIAN_POINT('Ctrl Pts',(0.131083074475465,-8.16256657218579,
7.37297043127167));
#48861=CARTESIAN_POINT('Ctrl Pts',(0.0873209945484005,-8.16307736259359,
7.37294033253635));
#48862=CARTESIAN_POINT('Ctrl Pts',(0.0435189611224462,-8.16333310546151,
7.37292499344789));
#48863=CARTESIAN_POINT('Ctrl Pts',(-0.000320651191468663,-8.16333198982214,
7.37292491924339));
#48864=CARTESIAN_POINT('Ctrl Pts',(-0.000413720047120908,-8.16333198745371,
7.37292491908586));
#48865=CARTESIAN_POINT('Ctrl Pts',(-0.000506788725943568,-8.16333198393689,
7.37292491898686));
#48866=CARTESIAN_POINT('Ctrl Pts',(-0.00059985722791523,-8.16333197927169,
7.37292491894639));
#48867=CARTESIAN_POINT('Ctrl Pts',(-0.245377838851759,-8.16331970940542,
7.37292481250585));
#48868=CARTESIAN_POINT('Ctrl Pts',(-0.488931755613559,-8.15536801383923,
7.37332890290789));
#48869=CARTESIAN_POINT('Ctrl Pts',(-0.730901381957773,-8.13972535157021,
7.37411291131156));
#48870=CARTESIAN_POINT('Ctrl Pts',(-0.980216234492042,-8.12360784089019,
7.37492071906206));
#48871=CARTESIAN_POINT('Ctrl Pts',(-1.22784963174372,-8.09932526051673,
7.37613203112047));
#48872=CARTESIAN_POINT('Ctrl Pts',(-1.47341230443435,-8.06709509687875,
7.37772761591521));
#48873=CARTESIAN_POINT('Ctrl Pts',(-1.5289648740937,-8.05980380789328,7.37808857808624));
#48874=CARTESIAN_POINT('Ctrl Pts',(-1.58441147063682,-8.05210556671063,
7.37846923010716));
#48875=CARTESIAN_POINT('Ctrl Pts',(-1.63974758292758,-8.04400252958216,
7.3788693880513));
#48876=CARTESIAN_POINT('Ctrl Pts',(-1.66249593119237,-8.04067141897518,
7.37903389061386));
#48877=CARTESIAN_POINT('Ctrl Pts',(-1.68522560774449,-8.03727189705941,
7.37920168975841));
#48878=CARTESIAN_POINT('Ctrl Pts',(-1.70793637302213,-8.03380422944271,
7.37937266330925));
#48879=CARTESIAN_POINT('Ctrl Pts',(-1.96557893968563,-7.99446522988985,
7.38131227493982));
#48880=CARTESIAN_POINT('Ctrl Pts',(-2.2207883398496,-7.94639486062531,7.38362138273935));
#48881=CARTESIAN_POINT('Ctrl Pts',(-2.47317150971626,-7.89003942090996,
7.3860437156412));
#48882=CARTESIAN_POINT('Ctrl Pts',(-2.49470738438798,-7.88523060704404,
7.38625041348803));
#48883=CARTESIAN_POINT('Ctrl Pts',(-2.51622268786283,-7.88036143821839,
7.38645794280466));
#48884=CARTESIAN_POINT('Ctrl Pts',(-2.53771717974228,-7.87543217538087,
7.38666614818949));
#48885=CARTESIAN_POINT('Ctrl Pts',(-2.67441352405635,-7.84408404145749,
7.3879902509007));
#48886=CARTESIAN_POINT('Ctrl Pts',(-2.81026874009531,-7.81030869440391,
7.38933832380954));
#48887=CARTESIAN_POINT('Ctrl Pts',(-2.94522550202804,-7.77418776918772,
7.39065223289004));
#48888=CARTESIAN_POINT('Ctrl Pts',(-2.98415816211496,-7.76376751544624,
7.39103127262754));
#48889=CARTESIAN_POINT('Ctrl Pts',(-3.02301611308487,-7.75315207789664,
7.39140741316152));
#48890=CARTESIAN_POINT('Ctrl Pts',(-3.06179791533473,-7.7423435060716,7.39177914203255));
#48891=CARTESIAN_POINT('Ctrl Pts',(-3.09023302610688,-7.7344185794487,7.3920516964527));
#48892=CARTESIAN_POINT('Ctrl Pts',(-3.11862720043851,-7.72638982465056,
7.39232187929955));
#48893=CARTESIAN_POINT('Ctrl Pts',(-3.1469800195739,-7.71825813772175,7.39258901229211));
#48894=CARTESIAN_POINT('Ctrl Pts',(-3.18049121270804,-7.70864701122754,
7.39290474616195));
#48895=CARTESIAN_POINT('Ctrl Pts',(-3.21394456796665,-7.69889206224753,
7.39321626893506));
#48896=CARTESIAN_POINT('Ctrl Pts',(-3.24733926263889,-7.68899472537593,
7.39352254275486));
#48897=CARTESIAN_POINT('Ctrl Pts',(-3.26403660997501,-7.68404605694013,
7.39367567966475));
#48898=CARTESIAN_POINT('Ctrl Pts',(-3.28071929216791,-7.6790617915099,7.39382750431879));
#48899=CARTESIAN_POINT('Ctrl Pts',(-3.29738720786073,-7.67404211112049,
7.3939778835142));
#48900=CARTESIAN_POINT('Ctrl Pts',(-3.30572116570713,-7.67153227092578,
7.39405307311191));
#48901=CARTESIAN_POINT('Ctrl Pts',(-3.31405143192873,-7.66901357699015,
7.39412790134407));
#48902=CARTESIAN_POINT('Ctrl Pts',(-3.32237799395243,-7.66648605224175,
7.39420235133963));
#48903=CARTESIAN_POINT('Ctrl Pts',(-3.33070455597614,-7.66395852749335,
7.39427680133519));
#48904=CARTESIAN_POINT('Ctrl Pts',(-3.34058221695287,-7.66094649443477,
7.39436464287305));
#48905=CARTESIAN_POINT('Ctrl Pts',(-3.34734655488609,-7.65887700853551,
7.39442454967878));
#48906=CARTESIAN_POINT('Ctrl Pts',(-3.55061731417835,-7.59668822165921,
7.39622477048512));
#48907=CARTESIAN_POINT('Ctrl Pts',(-3.74985865767998,-7.52978049086197,
7.39778867780606));
#48908=CARTESIAN_POINT('Ctrl Pts',(-3.94497680967061,-7.45869000841953,
7.39896700945016));
#48909=CARTESIAN_POINT('Ctrl Pts',(-4.05474130595829,-7.41869777337358,
7.39962988462632));
#48910=CARTESIAN_POINT('Ctrl Pts',(-4.16320143712219,-7.37738111165568,
7.4001711594348));
#48911=CARTESIAN_POINT('Ctrl Pts',(-4.27034412110881,-7.33483007898457,
7.40056737433741));
#48912=CARTESIAN_POINT('Ctrl Pts',(-4.46806378722257,-7.25630697633785,
7.40129854398276));
#48913=CARTESIAN_POINT('Ctrl Pts',(-4.66129573604226,-7.17358277320544,
7.40153435793695));
#48914=CARTESIAN_POINT('Ctrl Pts',(-4.85000961939606,-7.08719412760397,
7.40114665247284));
#48915=CARTESIAN_POINT('Ctrl Pts',(-5.00616780657878,-7.0157086912887,7.40082583144281));
#48916=CARTESIAN_POINT('Ctrl Pts',(-5.15923278578926,-6.94171325347014,
7.40007853980481));
#48917=CARTESIAN_POINT('Ctrl Pts',(-5.30919876766189,-6.8654904987653,7.39884386351234));
#48918=CARTESIAN_POINT('Ctrl Pts',(-5.44882245660878,-6.79452438991388,
7.39769433575639));
#48919=CARTESIAN_POINT('Ctrl Pts',(-5.58576002074305,-6.72162731991945,
7.39612251961714));
#48920=CARTESIAN_POINT('Ctrl Pts',(-5.72001849314537,-6.64700949805206,
7.39409296279186));
#48921=CARTESIAN_POINT('Ctrl Pts',(-5.71770960723051,-6.68335028393728,
8.11886589750961));
#48922=CARTESIAN_POINT('Ctrl Pts',(-5.721496759235,-6.6813783301849,8.11865841679221));
#48923=CARTESIAN_POINT('Ctrl Pts',(-5.76762296023213,-6.65682357416613,
8.11653387715794));
#48924=CARTESIAN_POINT('Ctrl Pts',(-5.85140117624736,-6.59964365038765,
8.12210181812362));
#48925=CARTESIAN_POINT('Ctrl Pts',(-5.94950294743152,-6.49819378604652,
8.15431025413625));
#48926=CARTESIAN_POINT('Ctrl Pts',(-6.01705132763319,-6.38857658526742,
8.20603404982171));
#48927=CARTESIAN_POINT('Ctrl Pts',(-6.04762129028345,-6.29253909066633,
8.26403289225712));
#48928=CARTESIAN_POINT('Ctrl Pts',(-6.05142104505506,-6.23757718496964,
8.30343898769059));
#48929=CARTESIAN_POINT('Ctrl Pts',(-6.05067380446042,-6.21682915403947,
8.31933149341578));
#48930=CARTESIAN_POINT('Ctrl Pts',(-5.60128072860216,-6.47591277950037,
7.91132944608927));
#48931=CARTESIAN_POINT('Ctrl Pts',(-5.60481509157088,-6.47408697639146,
7.91111770973153));
#48932=CARTESIAN_POINT('Ctrl Pts',(-5.6478672403021,-6.45135276446487,7.90890568143242));
#48933=CARTESIAN_POINT('Ctrl Pts',(-5.72616393016407,-6.39842545287255,
7.91348808972588));
#48934=CARTESIAN_POINT('Ctrl Pts',(-5.81784682618219,-6.30469904603656,
7.94236012175095));
#48935=CARTESIAN_POINT('Ctrl Pts',(-5.88081975256672,-6.2038613583221,7.98919173691161));
#48936=CARTESIAN_POINT('Ctrl Pts',(-5.90915113313628,-6.11618157328609,
8.04174195586025));
#48937=CARTESIAN_POINT('Ctrl Pts',(-5.91263441684734,-6.0665031749669,8.07730621375402));
#48938=CARTESIAN_POINT('Ctrl Pts',(-5.91194835104428,-6.04783961999084,
8.09161437792024));
#48939=CARTESIAN_POINT('Ctrl Pts',(-5.58641801495452,-6.47671513687815,
7.59599440984281));
#48940=CARTESIAN_POINT('Ctrl Pts',(-5.5914396953494,-6.47415139960797,7.59571095040917));
#48941=CARTESIAN_POINT('Ctrl Pts',(-5.65256568591855,-6.44225947547186,
7.59278698559726));
#48942=CARTESIAN_POINT('Ctrl Pts',(-5.76282180736241,-6.36873604510434,
7.59979555478798));
#48943=CARTESIAN_POINT('Ctrl Pts',(-5.89192971011888,-6.23901079269711,
7.64105456714741));
#48944=CARTESIAN_POINT('Ctrl Pts',(-5.98199882366734,-6.09762069092888,
7.70801622004692));
#48945=CARTESIAN_POINT('Ctrl Pts',(-6.02402385939053,-5.97078784562952,
7.78477094726962));
#48946=CARTESIAN_POINT('Ctrl Pts',(-6.02953497026119,-5.89570321681855,
7.83860015188576));
#48947=CARTESIAN_POINT('Ctrl Pts',(-6.02845916294772,-5.86690265917242,
7.86065144746598));
#48948=CARTESIAN_POINT('Ctrl Pts',(-5.68286000291914,-6.68523138736305,
7.37948114797694));
#48949=CARTESIAN_POINT('Ctrl Pts',(-5.69013455487577,-6.68152915634752,
7.37910549395911));
#48950=CARTESIAN_POINT('Ctrl Pts',(-5.77863954741206,-6.63550177846272,
7.37531163500955));
#48951=CARTESIAN_POINT('Ctrl Pts',(-5.93735490739454,-6.53002893406797,
7.38656833635098));
#48952=CARTESIAN_POINT('Ctrl Pts',(-6.1232092755155,-6.34417047782369,7.44782124655894));
#48953=CARTESIAN_POINT('Ctrl Pts',(-6.25429166682148,-6.13946766772676,
7.54674511464773));
#48954=CARTESIAN_POINT('Ctrl Pts',(-6.31696994181551,-5.95162571009039,
7.66149767844862));
#48955=CARTESIAN_POINT('Ctrl Pts',(-6.32552446128076,-5.8370923344154,7.74373065938116));
#48956=CARTESIAN_POINT('Ctrl Pts',(-6.32386337102072,-5.79257548224713,
7.77777893683687));
#48957=CARTESIAN_POINT('',(-5.99998177541742,-6.09546017895638,8.13557732174909));
#48958=CARTESIAN_POINT('',(-5.9999999892078,-6.44014740669715,7.42970580519182));
#48959=CARTESIAN_POINT('Ctrl Pts',(-5.99998177541743,-6.09546017895638,
8.13557732174909));
#48960=CARTESIAN_POINT('Ctrl Pts',(-5.99997919625023,-6.09857637890248,
8.11146641018613));
#48961=CARTESIAN_POINT('Ctrl Pts',(-5.9999803340948,-6.10217504456045,8.08748984324775));
#48962=CARTESIAN_POINT('Ctrl Pts',(-5.99999165905566,-6.10631456424762,
8.06375435735961));
#48963=CARTESIAN_POINT('Ctrl Pts',(-5.99999654214736,-6.10809944054681,
8.05352010087258));
#48964=CARTESIAN_POINT('Ctrl Pts',(-6.00000279747264,-6.10998446451239,
8.04333087802414));
#48965=CARTESIAN_POINT('Ctrl Pts',(-6.00000912002309,-6.11197215444399,
8.03319606361788));
#48966=CARTESIAN_POINT('Ctrl Pts',(-6.00002436664918,-6.11676540447511,
8.00875628621806));
#48967=CARTESIAN_POINT('Ctrl Pts',(-6.00004196881693,-6.12215899095557,
7.98463229462615));
#48968=CARTESIAN_POINT('Ctrl Pts',(-6.00006170986356,-6.12816391594866,
7.96094115182742));
#48969=CARTESIAN_POINT('Ctrl Pts',(-6.00007545974986,-6.13234642143875,
7.9444399740548));
#48970=CARTESIAN_POINT('Ctrl Pts',(-6.00008945445749,-6.13682448373006,
7.92814910102799));
#48971=CARTESIAN_POINT('Ctrl Pts',(-6.00009959581894,-6.14158753793689,
7.91210887700714));
#48972=CARTESIAN_POINT('Ctrl Pts',(-6.00011451576562,-6.14859493188932,
7.88851053780748));
#48973=CARTESIAN_POINT('Ctrl Pts',(-6.00011997332514,-6.15622144650364,
7.86545568059766));
#48974=CARTESIAN_POINT('Ctrl Pts',(-6.00010726677708,-6.16438990455441,
7.84306513481039));
#48975=CARTESIAN_POINT('Ctrl Pts',(-6.00010434192331,-6.16627015914626,
7.83791117230377));
#48976=CARTESIAN_POINT('Ctrl Pts',(-6.0001005134834,-6.16817892723834,7.83279234488374));
#48977=CARTESIAN_POINT('Ctrl Pts',(-6.00009580094069,-6.17011492270688,
7.82770999624424));
#48978=CARTESIAN_POINT('Ctrl Pts',(-6.00009028882588,-6.17237939646811,
7.82176533091493));
#48979=CARTESIAN_POINT('Ctrl Pts',(-6.00008356776384,-6.17468112514248,
7.81587057433163));
#48980=CARTESIAN_POINT('Ctrl Pts',(-6.00007594955505,-6.17701795841215,
7.81002763965109));
#48981=CARTESIAN_POINT('Ctrl Pts',(-6.00006018731391,-6.18185291772643,
7.79793847958003));
#48982=CARTESIAN_POINT('Ctrl Pts',(-6.00004624872792,-6.18690619132347,
7.78588595792757));
#48983=CARTESIAN_POINT('Ctrl Pts',(-6.00002902709531,-6.19209297392499,
7.77409400077235));
#48984=CARTESIAN_POINT('Ctrl Pts',(-6.00001165250664,-6.19732582357634,
7.76219731189432));
#48985=CARTESIAN_POINT('Ctrl Pts',(-5.99999048406169,-6.2026944521499,7.75056633780675));
#48986=CARTESIAN_POINT('Ctrl Pts',(-5.99997290021277,-6.2080602768582,7.7394209205877));
#48987=CARTESIAN_POINT('Ctrl Pts',(-5.99996100005097,-6.21169168784775,
7.73187807437623));
#48988=CARTESIAN_POINT('Ctrl Pts',(-5.99995104039366,-6.21532069069992,
7.7245573798538));
#48989=CARTESIAN_POINT('Ctrl Pts',(-5.99994980987496,-6.21889227642868,
7.71752287032711));
#48990=CARTESIAN_POINT('Ctrl Pts',(-5.99994574570744,-6.23068853981525,
7.69428923309306));
#48991=CARTESIAN_POINT('Ctrl Pts',(-5.99996685472504,-6.24333106014222,
7.67144245233745));
#48992=CARTESIAN_POINT('Ctrl Pts',(-5.99999370870832,-6.25680978298216,
7.6491604065561));
#48993=CARTESIAN_POINT('Ctrl Pts',(-6.0000205626916,-6.2702885058221,7.62687836077475));
#48994=CARTESIAN_POINT('Ctrl Pts',(-6.00005233393426,-6.28460341539502,
7.6051621505297));
#48995=CARTESIAN_POINT('Ctrl Pts',(-6.00007187511467,-6.29968647301357,
7.5841853475513));
#48996=CARTESIAN_POINT('Ctrl Pts',(-6.00009081506142,-6.31430546235059,
7.56385394878445));
#48997=CARTESIAN_POINT('Ctrl Pts',(-6.0000979707467,-6.32964551319117,7.54421778157841));
#48998=CARTESIAN_POINT('Ctrl Pts',(-6.00009088628216,-6.34559950855879,
7.52541402050796));
#48999=CARTESIAN_POINT('Ctrl Pts',(-6.00008371403553,-6.36175118650071,
7.50637726602054));
#49000=CARTESIAN_POINT('Ctrl Pts',(-6.00006153309211,-6.37853141538619,
7.48819446253251));
#49001=CARTESIAN_POINT('Ctrl Pts',(-6.00003861989632,-6.39578674332505,
7.4709791139653));
#49002=CARTESIAN_POINT('Ctrl Pts',(-6.00001938056299,-6.41027538161532,
7.4565240448229));
#49003=CARTESIAN_POINT('Ctrl Pts',(-5.99999990753438,-6.42509792872277,
7.44275065562263));
#49004=CARTESIAN_POINT('Ctrl Pts',(-5.99999991268315,-6.44014731027582,
7.42970569395491));
#49005=CARTESIAN_POINT('Ctrl Pts',(-5.7200186792232,-6.64700982302636,7.39409332428616));
#49006=CARTESIAN_POINT('Ctrl Pts',(-5.7727585915112,-6.61769118315081,7.39330242589221));
#49007=CARTESIAN_POINT('Ctrl Pts',(-5.82234911438972,-6.58559458350196,
7.39611192268061));
#49008=CARTESIAN_POINT('Ctrl Pts',(-5.86897225180668,-6.55106811709225,
7.40211988414016));
#49009=CARTESIAN_POINT('Ctrl Pts',(-5.91559538922365,-6.51654165068254,
7.40812784559972));
#49010=CARTESIAN_POINT('Ctrl Pts',(-5.95925138962019,-6.47958572443316,
7.41733473682809));
#49011=CARTESIAN_POINT('Ctrl Pts',(-6.00000003423404,-6.4401475070892,7.42970592100962));
#49012=CARTESIAN_POINT('Ctrl Pts',(-5.73278525690433,-6.65587891737084,
8.10255215275025));
#49013=CARTESIAN_POINT('Ctrl Pts',(-5.74761527810194,-6.64187384622179,
8.09761318170997));
#49014=CARTESIAN_POINT('Ctrl Pts',(-5.76160423035811,-6.62765828357803,
8.09343190819409));
#49015=CARTESIAN_POINT('Ctrl Pts',(-5.77475087102938,-6.61342753226589,
8.08988767501939));
#49016=CARTESIAN_POINT('Ctrl Pts',(-5.7887746893241,-6.59824726868458,8.08610696150641));
#49017=CARTESIAN_POINT('Ctrl Pts',(-5.80184019226813,-6.58304949672655,
8.08305131863796));
#49018=CARTESIAN_POINT('Ctrl Pts',(-5.81397380607243,-6.56802291292273,
8.08059407916663));
#49019=CARTESIAN_POINT('Ctrl Pts',(-5.81750441135948,-6.5636505192501,8.07987907844146));
#49020=CARTESIAN_POINT('Ctrl Pts',(-5.8209562778395,-6.55929233721068,8.07921485396509));
#49021=CARTESIAN_POINT('Ctrl Pts',(-5.8243304326853,-6.5549523578848,8.07859853892313));
#49022=CARTESIAN_POINT('Ctrl Pts',(-5.83655607327889,-6.53922722674923,
8.07636543269662));
#49023=CARTESIAN_POINT('Ctrl Pts',(-5.84776060403226,-6.52374510228417,
8.07475914495281));
#49024=CARTESIAN_POINT('Ctrl Pts',(-5.85802333829725,-6.50868496127945,
8.07363507561389));
#49025=CARTESIAN_POINT('Ctrl Pts',(-5.86887239880057,-6.49276441060259,
8.072446786416));
#49026=CARTESIAN_POINT('Ctrl Pts',(-5.87866929268569,-6.47731494656851,
8.07179769481914));
#49027=CARTESIAN_POINT('Ctrl Pts',(-5.88751987338268,-6.46249385037828,
8.07154513059879));
#49028=CARTESIAN_POINT('Ctrl Pts',(-5.89170343543667,-6.45548809812959,
8.07142574655783));
#49029=CARTESIAN_POINT('Ctrl Pts',(-5.89567570660684,-6.44862203152409,
8.07139532808666));
#49030=CARTESIAN_POINT('Ctrl Pts',(-5.89944849885801,-6.44190882017283,
8.07144059735559));
#49031=CARTESIAN_POINT('Ctrl Pts',(-5.90199189965474,-6.43738315696036,
8.07147111530808));
#49032=CARTESIAN_POINT('Ctrl Pts',(-5.90444465114991,-6.43292691848639,
8.07153605347808));
#49033=CARTESIAN_POINT('Ctrl Pts',(-5.90681044160722,-6.4285436545057,8.07163160007322));
#49034=CARTESIAN_POINT('Ctrl Pts',(-5.9099114189334,-6.42279825884871,8.07175683847893));
#49035=CARTESIAN_POINT('Ctrl Pts',(-5.91286301230243,-6.41717828879788,
8.07193462478606));
#49036=CARTESIAN_POINT('Ctrl Pts',(-5.91567435331598,-6.4116914615961,8.07215613452247));
#49037=CARTESIAN_POINT('Ctrl Pts',(-5.91815243471818,-6.40685504922909,
8.07235138623883));
#49038=CARTESIAN_POINT('Ctrl Pts',(-5.92052148273777,-6.40212216222683,
8.07258060357384));
#49039=CARTESIAN_POINT('Ctrl Pts',(-5.9227876888036,-6.39749723758926,8.07283826479711));
#49040=CARTESIAN_POINT('Ctrl Pts',(-5.92392079183651,-6.39518477527048,
8.07296709540874));
#49041=CARTESIAN_POINT('Ctrl Pts',(-5.92502817697261,-6.3928993003763,8.07310304094167));
#49042=CARTESIAN_POINT('Ctrl Pts',(-5.92611059719687,-6.39064132398295,
8.07324545116506));
#49043=CARTESIAN_POINT('Ctrl Pts',(-5.92687336413816,-6.38905015845549,
8.07334580572983));
#49044=CARTESIAN_POINT('Ctrl Pts',(-5.92731260918699,-6.38812757179801,
8.07340554956424));
#49045=CARTESIAN_POINT('Ctrl Pts',(-5.92808745871731,-6.38648961137362,
8.07351632282971));
#49046=CARTESIAN_POINT('Ctrl Pts',(-5.92841217545942,-6.38580319013711,
8.07356274466062));
#49047=CARTESIAN_POINT('Ctrl Pts',(-5.9287955171558,-6.38499101376511,8.0736183461214));
#49048=CARTESIAN_POINT('Ctrl Pts',(-5.92928369519092,-6.38395038033944,
8.07369144263413));
#49049=CARTESIAN_POINT('Ctrl Pts',(-5.93927522066233,-6.36265176665552,
8.07518750680789));
#49050=CARTESIAN_POINT('Ctrl Pts',(-5.94805545914819,-6.3416991033364,8.07736409307303));
#49051=CARTESIAN_POINT('Ctrl Pts',(-5.95569861714587,-6.32126287151163,
8.08008397448817));
#49052=CARTESIAN_POINT('Ctrl Pts',(-5.95898627403075,-6.31247235347184,
8.08125391456572));
#49053=CARTESIAN_POINT('Ctrl Pts',(-5.96206359504637,-6.30377677281201,
8.08252469091863));
#49054=CARTESIAN_POINT('Ctrl Pts',(-5.9649368000487,-6.29518712274744,8.0838866415702));
#49055=CARTESIAN_POINT('Ctrl Pts',(-5.97180219870552,-6.27466252670648,
8.08714096354386));
#49056=CARTESIAN_POINT('Ctrl Pts',(-5.9775031506717,-6.2547458399214,8.09091377323926));
#49057=CARTESIAN_POINT('Ctrl Pts',(-5.98217140046649,-6.2355691581327,8.09506266119555));
#49058=CARTESIAN_POINT('Ctrl Pts',(-5.98714021635121,-6.21515778229022,
8.0994786760378));
#49059=CARTESIAN_POINT('Ctrl Pts',(-5.99093857479877,-6.19558460226744,
8.1043210112003));
#49060=CARTESIAN_POINT('Ctrl Pts',(-5.99371838280598,-6.17695926812329,
8.10944787007493));
#49061=CARTESIAN_POINT('Ctrl Pts',(-5.99432005375399,-6.17292793846947,
8.11055754456733));
#49062=CARTESIAN_POINT('Ctrl Pts',(-5.99487399934209,-6.1689408443237,8.1116806455697));
#49063=CARTESIAN_POINT('Ctrl Pts',(-5.99538175392162,-6.16499882795019,
8.11281588855426));
#49064=CARTESIAN_POINT('Ctrl Pts',(-5.99773613140626,-6.14672032300294,
8.11807983028954));
#49065=CARTESIAN_POINT('Ctrl Pts',(-5.99909926553431,-6.1294140853808,8.12360223596205));
#49066=CARTESIAN_POINT('Ctrl Pts',(-5.9996680087375,-6.11314834194608,8.12924566890368));
#49067=CARTESIAN_POINT('Ctrl Pts',(-5.99987919730825,-6.10710846474153,
8.13134121664893));
#49068=CARTESIAN_POINT('Ctrl Pts',(-5.99998064351921,-6.10121167458743,
8.13345376339408));
#49069=CARTESIAN_POINT('Ctrl Pts',(-5.99998177541743,-6.09546017895638,
8.13557732174909));
#49070=CARTESIAN_POINT('Ctrl Pts',(-5.72202497003794,-10.282630745067,17.0373350432682));
#49071=CARTESIAN_POINT('Ctrl Pts',(-5.72274590418673,-10.3310953139824,
16.5600679618479));
#49072=CARTESIAN_POINT('Ctrl Pts',(-5.72404144894786,-10.3627265719337,
15.5563877915237));
#49073=CARTESIAN_POINT('Ctrl Pts',(-5.72530561181376,-10.1890958128617,
14.0392357399793));
#49074=CARTESIAN_POINT('Ctrl Pts',(-5.72546552594784,-9.77722827557498,
12.526135233631));
#49075=CARTESIAN_POINT('Ctrl Pts',(-5.72471376442816,-9.14170929304714,
11.0927040211933));
#49076=CARTESIAN_POINT('Ctrl Pts',(-5.72306595968661,-8.29718472548057,
9.77128759364862));
#49077=CARTESIAN_POINT('Ctrl Pts',(-5.72038925100475,-7.31941610585418,
8.65807787030266));
#49078=CARTESIAN_POINT('Ctrl Pts',(-5.71829764234389,-6.59327312663666,
8.03228833193905));
#49079=CARTESIAN_POINT('Ctrl Pts',(-5.71724205575826,-6.24681302335888,
7.7699843594215));
#49080=CARTESIAN_POINT('Ctrl Pts',(-5.90012992537085,-10.2258728720551,
17.031541509047));
#49081=CARTESIAN_POINT('Ctrl Pts',(-5.90074282924355,-10.2737314129026,
16.5568909290448));
#49082=CARTESIAN_POINT('Ctrl Pts',(-5.90184295197424,-10.3045732220607,
15.5587654379862));
#49083=CARTESIAN_POINT('Ctrl Pts',(-5.90291239263017,-10.1313394179603,
14.0503335166118));
#49084=CARTESIAN_POINT('Ctrl Pts',(-5.90304763810816,-9.72173758915438,
12.5458458210616));
#49085=CARTESIAN_POINT('Ctrl Pts',(-5.90241173218083,-9.09017458373661,
11.1204627334897));
#49086=CARTESIAN_POINT('Ctrl Pts',(-5.90101617902405,-8.25105475095447,
9.80605003590594));
#49087=CARTESIAN_POINT('Ctrl Pts',(-5.89873871610581,-7.27966994646323,
8.69819149816694));
#49088=CARTESIAN_POINT('Ctrl Pts',(-5.89695455612386,-6.55806882134033,
8.07501211881053));
#49089=CARTESIAN_POINT('Ctrl Pts',(-5.89604817364794,-6.21375837300073,
7.8137137118777));
#49090=CARTESIAN_POINT('Ctrl Pts',(-6.00738644022263,-10.07333564029,17.0159713723814));
#49091=CARTESIAN_POINT('Ctrl Pts',(-6.00770911568216,-10.1202651827221,
16.5484242038607));
#49092=CARTESIAN_POINT('Ctrl Pts',(-6.00828666207577,-10.1502618508912,
15.5651526753668));
#49093=CARTESIAN_POINT('Ctrl Pts',(-6.00884297265506,-9.97928411294258,
14.0795877254805));
#49094=CARTESIAN_POINT('Ctrl Pts',(-6.00891327897517,-9.57577907416303,
12.5976732429584));
#49095=CARTESIAN_POINT('Ctrl Pts',(-6.0085825645024,-8.95396889082556,11.1937656628233));
#49096=CARTESIAN_POINT('Ctrl Pts',(-6.00785461825364,-8.12782700841262,
9.89877135043688));
#49097=CARTESIAN_POINT('Ctrl Pts',(-6.00665324994361,-7.17162847329925,
8.80703886908177));
#49098=CARTESIAN_POINT('Ctrl Pts',(-6.00570635763836,-6.46111186998488,
8.19260787275657));
#49099=CARTESIAN_POINT('Ctrl Pts',(-6.00521778050847,-6.1221175179119,7.93494903754976));
#49100=CARTESIAN_POINT('Ctrl Pts',(-5.99965813360087,-9.88724153611006,
16.9969759522918));
#49101=CARTESIAN_POINT('Ctrl Pts',(-5.99962677163889,-9.93329878843649,
16.5381215791427));
#49102=CARTESIAN_POINT('Ctrl Pts',(-5.99956775772523,-9.96274069261619,
15.5729440399789));
#49103=CARTESIAN_POINT('Ctrl Pts',(-5.99950185524724,-9.79495907659826,
14.1150644943025));
#49104=CARTESIAN_POINT('Ctrl Pts',(-5.99949344308302,-9.39889493478627,
12.6604750418897));
#49105=CARTESIAN_POINT('Ctrl Pts',(-5.99953275683936,-8.78865516910236,
11.2827099739524));
#49106=CARTESIAN_POINT('Ctrl Pts',(-5.99961543411688,-7.97776892723705,
10.0116282351798));
#49107=CARTESIAN_POINT('Ctrl Pts',(-5.99972805551254,-7.03936234204484,
8.94022040002282));
#49108=CARTESIAN_POINT('Ctrl Pts',(-5.9998067257913,-6.34195020476634,8.33710919452135));
#49109=CARTESIAN_POINT('Ctrl Pts',(-5.99983414287826,-6.00926938820036,
8.08424026560283));
#49110=CARTESIAN_POINT('',(-5.99999988467789,-9.91329944128341,16.8993703244349));
#49111=CARTESIAN_POINT('Origin',(-5.5999816434089,-9.91328771269701,16.8993697092576));
#49112=CARTESIAN_POINT('Ctrl Pts',(-6.,-9.91329812074841,16.8993691889373));
#49113=CARTESIAN_POINT('Ctrl Pts',(-6.,-9.9568397826802,16.4254094106132));
#49114=CARTESIAN_POINT('Ctrl Pts',(-6.,-9.96638815209589,15.953283891413));
#49115=CARTESIAN_POINT('Ctrl Pts',(-6.,-9.94189523094625,15.4800411552409));
#49116=CARTESIAN_POINT('Ctrl Pts',(-6.,-9.91740229247353,15.0067980843589));
#49117=CARTESIAN_POINT('Ctrl Pts',(-6.,-9.85886801528275,14.5324377949245));
#49118=CARTESIAN_POINT('Ctrl Pts',(-6.,-9.76681036565181,14.0658326091363));
#49119=CARTESIAN_POINT('Ctrl Pts',(-6.,-9.67475271602093,13.5992274233484));
#49120=CARTESIAN_POINT('Ctrl Pts',(-6.,-9.54917169394994,13.1403773412066));
#49121=CARTESIAN_POINT('Ctrl Pts',(-6.,-9.39100128066893,12.6919788380545));
#49122=CARTESIAN_POINT('Ctrl Pts',(-6.,-9.2328308673878,12.2435803349021));
#49123=CARTESIAN_POINT('Ctrl Pts',(-6.,-9.0420710628966,11.8056334107393));
#49124=CARTESIAN_POINT('Ctrl Pts',(-6.,-8.82146085875875,11.3843739927917));
#49125=CARTESIAN_POINT('Ctrl Pts',(-6.,-8.60085065462106,10.9631145748444));
#49126=CARTESIAN_POINT('Ctrl Pts',(-6.,-8.35039005083675,10.5585426631122));
#49127=CARTESIAN_POINT('Ctrl Pts',(-6.,-8.07150643558797,10.1733977819344));
#49128=CARTESIAN_POINT('Ctrl Pts',(-6.,-7.792622820339,9.78825290075636));
#49129=CARTESIAN_POINT('Ctrl Pts',(-6.,-7.48531619362553,9.42253505013277));
#49130=CARTESIAN_POINT('Ctrl Pts',(-6.,-7.15537146437222,9.08219258646993));
#49131=CARTESIAN_POINT('Ctrl Pts',(-6.,-6.82542673511914,8.74185012280732));
#49132=CARTESIAN_POINT('Ctrl Pts',(-6.,-6.47284390332625,8.42688304610544));
#49133=CARTESIAN_POINT('Ctrl Pts',(-6.,-6.09546018099012,8.13557732069495));
#49134=CARTESIAN_POINT('Origin',(-5.599999999997,-9.91330329093349,16.899368849389));
#49135=CARTESIAN_POINT('Origin',(-5.6,-9.91330329095944,16.8993688494318));
#49136=CARTESIAN_POINT('Ctrl Pts',(-6.05065185023871,-4.09650686474605,
9.54349128053163));
#49137=CARTESIAN_POINT('Ctrl Pts',(-6.05140972708256,-4.0723989783453,9.55349643619757));
#49138=CARTESIAN_POINT('Ctrl Pts',(-6.04764687447984,-4.01080955139642,
9.58136929929187));
#49139=CARTESIAN_POINT('Ctrl Pts',(-6.01714389005373,-3.91255120432432,
9.63551943372867));
#49140=CARTESIAN_POINT('Ctrl Pts',(-5.94963119729813,-3.81288206008285,
9.7046038434688));
#49141=CARTESIAN_POINT('Ctrl Pts',(-5.85153569778131,-3.73419722399452,
9.77638417842136));
#49142=CARTESIAN_POINT('Ctrl Pts',(-5.76771443214422,-3.70073548179553,
9.82315751901543));
#49143=CARTESIAN_POINT('Ctrl Pts',(-5.72154537198058,-3.69027983102092,
9.84550922441198));
#49144=CARTESIAN_POINT('Ctrl Pts',(-5.71772607536419,-3.68946642963374,
9.84733621716733));
#49145=CARTESIAN_POINT('Ctrl Pts',(-5.91196388319657,-3.98378410118069,
9.28331121105742));
#49146=CARTESIAN_POINT('Ctrl Pts',(-5.91265976607569,-3.96208637840918,
9.29230536714295));
#49147=CARTESIAN_POINT('Ctrl Pts',(-5.9092102407762,-3.90646135451234,9.31752641532043));
#49148=CARTESIAN_POINT('Ctrl Pts',(-5.88093976386008,-3.81709709389408,
9.36716626955956));
#49149=CARTESIAN_POINT('Ctrl Pts',(-5.81799703832602,-3.72605533285352,
9.43109497458473));
#49150=CARTESIAN_POINT('Ctrl Pts',(-5.72631526514141,-3.65412316410241,
9.49785603133131));
#49151=CARTESIAN_POINT('Ctrl Pts',(-5.64797404963314,-3.62364364874167,
9.54143888864739));
#49152=CARTESIAN_POINT('Ctrl Pts',(-5.60487947444387,-3.61417509384371,
9.56225713834693));
#49153=CARTESIAN_POINT('Ctrl Pts',(-5.60131491490269,-3.61343908276037,
9.56395871527821));
#49154=CARTESIAN_POINT('Ctrl Pts',(-6.02845826007556,-3.8743345208937,9.01112785386752));
#49155=CARTESIAN_POINT('Ctrl Pts',(-6.02954938100152,-3.84087507001535,
9.02502218021019));
#49156=CARTESIAN_POINT('Ctrl Pts',(-6.02409034814899,-3.75673115811109,
9.06310624745352));
#49157=CARTESIAN_POINT('Ctrl Pts',(-5.98215261412372,-3.62681858681912,
9.13454712209158));
#49158=CARTESIAN_POINT('Ctrl Pts',(-5.89212705130421,-3.49804224901997,
9.22353624826158));
#49159=CARTESIAN_POINT('Ctrl Pts',(-5.76302541892318,-3.39736161362055,
9.31528648438854));
#49160=CARTESIAN_POINT('Ctrl Pts',(-5.65271278399101,-3.35446635079726,
9.37550371289834));
#49161=CARTESIAN_POINT('Ctrl Pts',(-5.59153007899971,-3.34102908670047,
9.40461648632458));
#49162=CARTESIAN_POINT('Ctrl Pts',(-5.58646575731296,-3.33998355022766,
9.40699867986969));
#49163=CARTESIAN_POINT('Ctrl Pts',(-6.32381572581365,-3.83986183316476,
8.90525672846377));
#49164=CARTESIAN_POINT('Ctrl Pts',(-6.32550038395361,-3.78817424015326,
8.92675213935762));
#49165=CARTESIAN_POINT('Ctrl Pts',(-6.31702550013207,-3.65971176909999,
8.98478709160199));
#49166=CARTESIAN_POINT('Ctrl Pts',(-6.25447459339337,-3.46637296327811,
9.09005775360737));
#49167=CARTESIAN_POINT('Ctrl Pts',(-6.12345620551607,-3.27822119685277,
9.21790555729585));
#49168=CARTESIAN_POINT('Ctrl Pts',(-5.937616052749,-3.13212498574318,9.34828223376809));
#49169=CARTESIAN_POINT('Ctrl Pts',(-5.77882600926223,-3.06954994799304,
9.43406098886272));
#49170=CARTESIAN_POINT('Ctrl Pts',(-5.69024266127033,-3.04978819593502,
9.47586226246463));
#49171=CARTESIAN_POINT('Ctrl Pts',(-5.68290661947263,-3.0482489982039,9.47928521174236));
#49172=CARTESIAN_POINT('',(-5.73278765687023,-3.68906981625968,9.8154374870846));
#49173=CARTESIAN_POINT('',(-5.72001858491459,-3.0799676634134,9.45352580072754));
#49174=CARTESIAN_POINT('Origin',(-5.89876013871265,-3.22462655825293,9.8975005542016));
#49175=CARTESIAN_POINT('',(-5.99999998735835,-3.21424020897419,9.29218418198714));
#49176=CARTESIAN_POINT('Ctrl Pts',(-6.00000003704887,-3.21424025835317,
9.29218432473884));
#49177=CARTESIAN_POINT('Ctrl Pts',(-5.95925151906109,-3.18380747703174,
9.32015314616885));
#49178=CARTESIAN_POINT('Ctrl Pts',(-5.91559554599687,-3.15735621311459,
9.34755442745742));
#49179=CARTESIAN_POINT('Ctrl Pts',(-5.86897240659433,-3.13488993689926,
9.37445124425472));
#49180=CARTESIAN_POINT('Ctrl Pts',(-5.82234926719179,-3.11242366068393,
9.40134806105201));
#49181=CARTESIAN_POINT('Ctrl Pts',(-5.77275871290704,-3.09394217276707,
9.42773982822785));
#49182=CARTESIAN_POINT('Ctrl Pts',(-5.72001867761081,-3.07996773842414,
9.4535260309681));
#49183=CARTESIAN_POINT('',(-5.9999819026388,-3.99788652873932,9.3466120296767));
#49184=CARTESIAN_POINT('Ctrl Pts',(-5.9999819026388,-3.99788652873932,9.3466120296767));
#49185=CARTESIAN_POINT('Ctrl Pts',(-5.99997892502811,-3.97149634512734,
9.33560737629572));
#49186=CARTESIAN_POINT('Ctrl Pts',(-5.99997956294922,-3.94521403643915,
9.32545947544754));
#49187=CARTESIAN_POINT('Ctrl Pts',(-5.99997436131157,-3.91905572044391,
9.31619701323493));
#49188=CARTESIAN_POINT('Ctrl Pts',(-5.99997319891254,-3.91321017653617,
9.31412715026793));
#49189=CARTESIAN_POINT('Ctrl Pts',(-5.99997162450337,-3.90737086585166,
9.31210133530766));
#49190=CARTESIAN_POINT('Ctrl Pts',(-5.99996939181339,-3.9015380218435,9.31011961125842));
#49191=CARTESIAN_POINT('Ctrl Pts',(-5.99995605169999,-3.86668732551883,
9.29827899578118));
#49192=CARTESIAN_POINT('Ctrl Pts',(-5.9999237641423,-3.83206867179135,9.28801549899031));
#49193=CARTESIAN_POINT('Ctrl Pts',(-5.99990968741117,-3.79764807109586,
9.27929778340875));
#49194=CARTESIAN_POINT('Ctrl Pts',(-5.99990773622705,-3.79287701104904,
9.27808941563857));
#49195=CARTESIAN_POINT('Ctrl Pts',(-5.99990608047017,-3.78810971834973,
9.27691070715592));
#49196=CARTESIAN_POINT('Ctrl Pts',(-5.99990478331505,-3.78334605668427,
9.27576155474841));
#49197=CARTESIAN_POINT('Ctrl Pts',(-5.9998966985705,-3.75365570796689,9.26859926277548));
#49198=CARTESIAN_POINT('Ctrl Pts',(-5.99989594461753,-3.7241164923183,9.26260358244453));
#49199=CARTESIAN_POINT('Ctrl Pts',(-5.99989840958442,-3.6947401127648,9.25777487994042));
#49200=CARTESIAN_POINT('Ctrl Pts',(-5.99990034204125,-3.67170995132592,
9.25398932842249));
#49201=CARTESIAN_POINT('Ctrl Pts',(-5.99990481363489,-3.64877936325589,
9.25092042635753));
#49202=CARTESIAN_POINT('Ctrl Pts',(-5.99991482494673,-3.6259412251828,9.24857354713652));
#49203=CARTESIAN_POINT('Ctrl Pts',(-5.99991833498322,-3.61793401302479,
9.24775071474223));
#49204=CARTESIAN_POINT('Ctrl Pts',(-5.99992684845666,-3.60967244995355,
9.2469869642076));
#49205=CARTESIAN_POINT('Ctrl Pts',(-5.99993256981174,-3.60152318467775,
9.24633123599943));
#49206=CARTESIAN_POINT('Ctrl Pts',(-5.99993836287564,-3.5932717802666,9.24566728919611));
#49207=CARTESIAN_POINT('Ctrl Pts',(-5.99994102036157,-3.58513584158189,
9.24511412208589));
#49208=CARTESIAN_POINT('Ctrl Pts',(-5.99994630413676,-3.57751190194319,
9.24467223767596));
#49209=CARTESIAN_POINT('Ctrl Pts',(-5.9999470916684,-3.57637557546306,9.24460637606373));
#49210=CARTESIAN_POINT('Ctrl Pts',(-5.99994796568151,-3.57525064535877,
9.24454289917138));
#49211=CARTESIAN_POINT('Ctrl Pts',(-5.99994897476035,-3.57413844577657,
9.24448172000767));
#49212=CARTESIAN_POINT('Ctrl Pts',(-5.99997574698198,-3.54463029204011,
9.24285855434815));
#49213=CARTESIAN_POINT('Ctrl Pts',(-5.99996192315438,-3.51552751704015,
9.24253165400506));
#49214=CARTESIAN_POINT('Ctrl Pts',(-5.99993728662295,-3.48683842875823,
9.24342037855321));
#49215=CARTESIAN_POINT('Ctrl Pts',(-5.99991766072212,-3.46398418878542,
9.24412835239656));
#49216=CARTESIAN_POINT('Ctrl Pts',(-5.99989194171101,-3.4413915343842,9.24560839507766));
#49217=CARTESIAN_POINT('Ctrl Pts',(-5.99987472933798,-3.41905659359933,
9.24784231031407));
#49218=CARTESIAN_POINT('Ctrl Pts',(-5.99985423749428,-3.39246618014718,
9.25050185306036));
#49219=CARTESIAN_POINT('Ctrl Pts',(-5.99984743226518,-3.36623979468742,
9.25422906380482));
#49220=CARTESIAN_POINT('Ctrl Pts',(-5.99986332455246,-3.34036723982923,
9.25903426734148));
#49221=CARTESIAN_POINT('Ctrl Pts',(-5.99987871369806,-3.3153137968055,9.26368734059547));
#49222=CARTESIAN_POINT('Ctrl Pts',(-5.99991598087344,-3.29059138763699,
9.26935207733197));
#49223=CARTESIAN_POINT('Ctrl Pts',(-5.9999511570379,-3.26620847344255,9.27606922917231));
#49224=CARTESIAN_POINT('Ctrl Pts',(-5.99997640640063,-3.24870647871583,
9.28089078393606));
#49225=CARTESIAN_POINT('Ctrl Pts',(-5.99999991134788,-3.23137977939288,
9.28625531048571));
#49226=CARTESIAN_POINT('Ctrl Pts',(-5.99999991596861,-3.21424016050503,
9.29218404186559));
#49227=CARTESIAN_POINT('Ctrl Pts',(-5.9999819026388,-3.99788652873932,9.3466120296767));
#49228=CARTESIAN_POINT('Ctrl Pts',(-5.99997890799539,-3.98519840970855,
9.35715883213799));
#49229=CARTESIAN_POINT('Ctrl Pts',(-5.99925065772263,-3.97204910714977,
9.36865876554123));
#49230=CARTESIAN_POINT('Ctrl Pts',(-5.99760763522023,-3.95857513389356,
9.38112775869376));
#49231=CARTESIAN_POINT('Ctrl Pts',(-5.99700537153811,-3.95363613595889,
9.38569837274031));
#49232=CARTESIAN_POINT('Ctrl Pts',(-5.99628002057492,-3.94865393845055,
9.39039903246601));
#49233=CARTESIAN_POINT('Ctrl Pts',(-5.99542154791787,-3.94363681618573,
9.39522993978368));
#49234=CARTESIAN_POINT('Ctrl Pts',(-5.99297223882613,-3.92932246024583,
9.40901300569433));
#49235=CARTESIAN_POINT('Ctrl Pts',(-5.98943905602187,-3.914720076621,9.42385864009363));
#49236=CARTESIAN_POINT('Ctrl Pts',(-5.9846468393107,-3.9000247023485,9.43974507481651));
#49237=CARTESIAN_POINT('Ctrl Pts',(-5.98035089087139,-3.88685113905285,
9.453986355745));
#49238=CARTESIAN_POINT('Ctrl Pts',(-5.97504355429744,-3.87360276162521,
9.46906389698083));
#49239=CARTESIAN_POINT('Ctrl Pts',(-5.96859394862519,-3.86046121996682,
9.48493891553766));
#49240=CARTESIAN_POINT('Ctrl Pts',(-5.96744221923484,-3.85811448738632,
9.48777377496526));
#49241=CARTESIAN_POINT('Ctrl Pts',(-5.96625404234337,-3.85577127801689,
9.49063400267137));
#49242=CARTESIAN_POINT('Ctrl Pts',(-5.96502863926366,-3.85343278478609,
9.4935192944734));
#49243=CARTESIAN_POINT('Ctrl Pts',(-5.96428753790516,-3.85201850687305,
9.49526426615625));
#49244=CARTESIAN_POINT('Ctrl Pts',(-5.96353282016883,-3.85060595508656,
9.49701840481362));
#49245=CARTESIAN_POINT('Ctrl Pts',(-5.96276437690544,-3.84919536030071,
9.49878163548696));
#49246=CARTESIAN_POINT('Ctrl Pts',(-5.95818717714525,-3.84079321218763,
9.50928424433221));
#49247=CARTESIAN_POINT('Ctrl Pts',(-5.9531229036142,-3.83245988915338,9.52010985266385));
#49248=CARTESIAN_POINT('Ctrl Pts',(-5.94754929030463,-3.82424849588493,
9.53123959893818));
#49249=CARTESIAN_POINT('Ctrl Pts',(-5.94476248364985,-3.8201427992507,9.53680447207534));
#49250=CARTESIAN_POINT('Ctrl Pts',(-5.9418483004759,-3.81606760916532,9.54244537605093));
#49251=CARTESIAN_POINT('Ctrl Pts',(-5.93880412211886,-3.81203044433949,
9.54815934825822));
#49252=CARTESIAN_POINT('Ctrl Pts',(-5.93728203294034,-3.81001186192658,
9.55101633436187));
#49253=CARTESIAN_POINT('Ctrl Pts',(-5.93572744171875,-3.80800278761671,
9.55389158725416));
#49254=CARTESIAN_POINT('Ctrl Pts',(-5.93414001676768,-3.80600420060038,
9.55678471395299));
#49255=CARTESIAN_POINT('Ctrl Pts',(-5.9330828181687,-3.80467317490864,9.55871148818607));
#49256=CARTESIAN_POINT('Ctrl Pts',(-5.93173984860894,-3.80301368285739,
9.56113444361949));
#49257=CARTESIAN_POINT('Ctrl Pts',(-5.93065095545942,-3.80169303734624,
9.56307800903407));
#49258=CARTESIAN_POINT('Ctrl Pts',(-5.93010483305342,-3.8010306820873,9.56405278293258));
#49259=CARTESIAN_POINT('Ctrl Pts',(-5.92962351987447,-3.80045288203708,
9.56490693977137));
#49260=CARTESIAN_POINT('Ctrl Pts',(-5.9292789011774,-3.8000409048946,9.56551731005603));
#49261=CARTESIAN_POINT('Ctrl Pts',(-5.92342174375046,-3.79303891980119,
9.57589119538594));
#49262=CARTESIAN_POINT('Ctrl Pts',(-5.91678402183533,-3.78574286570555,
9.58714431119368));
#49263=CARTESIAN_POINT('Ctrl Pts',(-5.90922580100395,-3.77831400530464,
9.59925023020935));
#49264=CARTESIAN_POINT('Ctrl Pts',(-5.90846944344672,-3.7775705929552,9.60046167977386));
#49265=CARTESIAN_POINT('Ctrl Pts',(-5.90770386059727,-3.77682588945337,
9.6016816510152));
#49266=CARTESIAN_POINT('Ctrl Pts',(-5.90692890757045,-3.77608008326768,
9.60291010453114));
#49267=CARTESIAN_POINT('Ctrl Pts',(-5.89944452236005,-3.76887719406945,
9.61477433243671));
#49268=CARTESIAN_POINT('Ctrl Pts',(-5.89108567512895,-3.76156832512594,
9.62743169755309));
#49269=CARTESIAN_POINT('Ctrl Pts',(-5.88173640074049,-3.75432835168381,
9.64083690558411));
#49270=CARTESIAN_POINT('Ctrl Pts',(-5.87446311616708,-3.74869600151837,
9.65126551092012));
#49271=CARTESIAN_POINT('Ctrl Pts',(-5.86659043159745,-3.74310588829126,
9.66214639069774));
#49272=CARTESIAN_POINT('Ctrl Pts',(-5.85806724378538,-3.73765871579024,
9.67344653471384));
#49273=CARTESIAN_POINT('Ctrl Pts',(-5.8478284059915,-3.73111507074768,9.68702130793009));
#49274=CARTESIAN_POINT('Ctrl Pts',(-5.83665027253931,-3.72477596569576,
9.70120218750934));
#49275=CARTESIAN_POINT('Ctrl Pts',(-5.82445357514376,-3.71885526366353,
9.71590692351583));
#49276=CARTESIAN_POINT('Ctrl Pts',(-5.81280378431398,-3.71320004914077,
9.72995229113683));
#49277=CARTESIAN_POINT('Ctrl Pts',(-5.80022371135754,-3.70792744423552,
9.74447553567856));
#49278=CARTESIAN_POINT('Ctrl Pts',(-5.78667898044615,-3.7032345474092,9.75938338006826));
#49279=CARTESIAN_POINT('Ctrl Pts',(-5.77401425347524,-3.69884654905051,
9.77332265875571));
#49280=CARTESIAN_POINT('Ctrl Pts',(-5.76050602541545,-3.69496516378039,
9.78759826545324));
#49281=CARTESIAN_POINT('Ctrl Pts',(-5.7461478796606,-3.69178345774301,9.80210884284901));
#49282=CARTESIAN_POINT('Ctrl Pts',(-5.74177234227017,-3.69081385665596,
9.80653083264045));
#49283=CARTESIAN_POINT('Ctrl Pts',(-5.73731804252361,-3.68990948299376,
9.81097445275041));
#49284=CARTESIAN_POINT('Ctrl Pts',(-5.73278526695723,-3.68907650035723,
9.81543630638497));
#49285=CARTESIAN_POINT('Ctrl Pts',(-5.71725994859976,-3.6056013506233,9.29487895543824));
#49286=CARTESIAN_POINT('Ctrl Pts',(-5.71831552981187,-3.65953318106983,
9.72607761564714));
#49287=CARTESIAN_POINT('Ctrl Pts',(-5.72040712143486,-3.83841163152394,
10.6678343458936));
#49288=CARTESIAN_POINT('Ctrl Pts',(-5.72308379499235,-4.31359623826603,
12.0712142427945));
#49289=CARTESIAN_POINT('Ctrl Pts',(-5.72473157500471,-5.03571382654535,
13.4633014200608));
#49290=CARTESIAN_POINT('Ctrl Pts',(-5.72548332476085,-5.95934168456203,
14.7303918598931));
#49291=CARTESIAN_POINT('Ctrl Pts',(-5.72532341316257,-7.06379075900272,
15.8436292363302));
#49292=CARTESIAN_POINT('Ctrl Pts',(-5.72405927318753,-8.29086345814456,
16.7525709110518));
#49293=CARTESIAN_POINT('Ctrl Pts',(-5.72276375585025,-9.17588690984407,
17.2270157661404));
#49294=CARTESIAN_POINT('Ctrl Pts',(-5.72204284054482,-9.61344026743877,
17.4236765036483));
#49295=CARTESIAN_POINT('Ctrl Pts',(-5.89606004581221,-3.66000666368765,
9.28811662465129));
#49296=CARTESIAN_POINT('Ctrl Pts',(-5.89696640239014,-3.71414242649981,
9.71695052206151));
#49297=CARTESIAN_POINT('Ctrl Pts',(-5.89875049980449,-3.89303118636646,
10.6534681301436));
#49298=CARTESIAN_POINT('Ctrl Pts',(-5.90102787762071,-4.36677305776408,
12.0486428922503));
#49299=CARTESIAN_POINT('Ctrl Pts',(-5.90242337426096,-5.08552707877001,
13.4325466081192));
#49300=CARTESIAN_POINT('Ctrl Pts',(-5.90305925435447,-6.00416238723668,
14.6921861279471));
#49301=CARTESIAN_POINT('Ctrl Pts',(-5.90292401435139,-7.10228463864252,
15.7991541637147));
#49302=CARTESIAN_POINT('Ctrl Pts',(-5.90185462016992,-8.322003131726,16.7033913584665));
#49303=CARTESIAN_POINT('Ctrl Pts',(-5.9007545479202,-9.20182078389947,17.1757422132168));
#49304=CARTESIAN_POINT('Ctrl Pts',(-5.90014167552026,-9.63680489054994,
17.3716193894984));
#49305=CARTESIAN_POINT('Ctrl Pts',(-6.00522116866736,-3.81082060828096,
9.26937107071129));
#49306=CARTESIAN_POINT('Ctrl Pts',(-6.00570971511597,-3.86446243505639,
9.69178123092468));
#49307=CARTESIAN_POINT('Ctrl Pts',(-6.00665653329783,-4.0413170753428,10.6143250570191));
#49308=CARTESIAN_POINT('Ctrl Pts',(-6.00785781208216,-4.50868641018821,
11.9882849936967));
#49309=CARTESIAN_POINT('Ctrl Pts',(-6.00858569914826,-5.21711252467402,
13.3512402332268));
#49310=CARTESIAN_POINT('Ctrl Pts',(-6.00891638705178,-6.12202585435753,
14.5916957615917));
#49311=CARTESIAN_POINT('Ctrl Pts',(-6.00884608631042,-7.20364747990103,
15.6820971652467));
#49312=CARTESIAN_POINT('Ctrl Pts',(-6.00828982250237,-8.40469064056497,
16.5729470365179));
#49313=CARTESIAN_POINT('Ctrl Pts',(-6.00771232487956,-9.27122184737554,
17.0386027958654));
#49314=CARTESIAN_POINT('Ctrl Pts',(-6.00738967876521,-9.69958976605554,
17.2317327933039));
#49315=CARTESIAN_POINT('Ctrl Pts',(-5.99983391384278,-3.99652936940203,
9.2462882081223));
#49316=CARTESIAN_POINT('Ctrl Pts',(-5.99980647643591,-4.04917980289419,
9.66083589408773));
#49317=CARTESIAN_POINT('Ctrl Pts',(-5.99972775387988,-4.22278351469519,
10.5663714352303));
#49318=CARTESIAN_POINT('Ctrl Pts',(-5.99961507899353,-4.68144737106702,
11.9147614578706));
#49319=CARTESIAN_POINT('Ctrl Pts',(-5.99953236569529,-5.37679277436971,
13.2525493754026));
#49320=CARTESIAN_POINT('Ctrl Pts',(-5.99949303625143,-6.26485171777721,
14.4699140490644));
#49321=CARTESIAN_POINT('Ctrl Pts',(-5.99950145165108,-7.3265302039202,15.5402095165816));
#49322=CARTESIAN_POINT('Ctrl Pts',(-5.99956738117704,-8.50519588233293,
16.4144492818083));
#49323=CARTESIAN_POINT('Ctrl Pts',(-5.99962642146639,-9.35578039726249,
16.871538751569));
#49324=CARTESIAN_POINT('Ctrl Pts',(-5.99965779862438,-9.77618429775514,
17.061077895889));
#49325=CARTESIAN_POINT('',(-5.99999997114735,-9.6786333714602,17.0348538902214));
#49326=CARTESIAN_POINT('Ctrl Pts',(-6.,-3.99788652685643,9.34661203088348));
#49327=CARTESIAN_POINT('Ctrl Pts',(-6.,-4.06147282781482,9.81908884364364));
#49328=CARTESIAN_POINT('Ctrl Pts',(-6.,-4.1579509296493,10.2819181094307));
#49329=CARTESIAN_POINT('Ctrl Pts',(-6.,-4.2877238070187,10.7378298887288));
#49330=CARTESIAN_POINT('Ctrl Pts',(-6.,-4.4174966843882,11.1937416680273));
#49331=CARTESIAN_POINT('Ctrl Pts',(-6.,-4.58056433729266,11.6427359608369));
#49332=CARTESIAN_POINT('Ctrl Pts',(-6.,-4.77466778468932,12.0768286890182));
#49333=CARTESIAN_POINT('Ctrl Pts',(-6.,-4.96877123208584,12.5109214171993));
#49334=CARTESIAN_POINT('Ctrl Pts',(-6.,-5.19391047397451,12.930112580752));
#49335=CARTESIAN_POINT('Ctrl Pts',(-6.,-5.4484267220564,13.3317963060837));
#49336=CARTESIAN_POINT('Ctrl Pts',(-6.,-5.70294297013846,13.7334800314157));
#49337=CARTESIAN_POINT('Ctrl Pts',(-6.,-5.98683622441378,14.1176563185267));
#49338=CARTESIAN_POINT('Ctrl Pts',(-6.,-6.29607551364862,14.4788351606867));
#49339=CARTESIAN_POINT('Ctrl Pts',(-6.,-6.60531480288324,14.8400140028466));
#49340=CARTESIAN_POINT('Ctrl Pts',(-6.,-6.93990012707735,15.1781954000556));
#49341=CARTESIAN_POINT('Ctrl Pts',(-6.,-7.29796324417597,15.4912222498826));
#49342=CARTESIAN_POINT('Ctrl Pts',(-6.,-7.65602636127484,15.8042490997097));
#49343=CARTESIAN_POINT('Ctrl Pts',(-6.,-8.03756727127826,16.0921214021547));
#49344=CARTESIAN_POINT('Ctrl Pts',(-6.,-8.43516131244481,16.3499544329203));
#49345=CARTESIAN_POINT('Ctrl Pts',(-6.,-8.83275507233027,16.6077872812798));
#49346=CARTESIAN_POINT('Ctrl Pts',(-6.,-9.24640194066504,16.835580900463));
#49347=CARTESIAN_POINT('Ctrl Pts',(-6.,-9.67863396568507,17.0348526013128));
#49348=CARTESIAN_POINT('',(-5.73644356943,-9.52121843706026,17.376327826582));
#49349=CARTESIAN_POINT('Origin',(-5.5999816381906,-9.67863859075266,17.0348433699664));
#49350=CARTESIAN_POINT('Ctrl Pts',(-5.732787802673,-3.68906940981089,9.81543755867358));
#49351=CARTESIAN_POINT('Ctrl Pts',(-5.73461480969872,-3.83284536601077,
10.625338537734));
#49352=CARTESIAN_POINT('Ctrl Pts',(-5.73605973938219,-4.07387518713724,
11.4195438346354));
#49353=CARTESIAN_POINT('Ctrl Pts',(-5.73818934988832,-4.74008577639406,
12.9297554589891));
#49354=CARTESIAN_POINT('Ctrl Pts',(-5.73887403071099,-5.1646384849479,13.6459905214075));
#49355=CARTESIAN_POINT('Ctrl Pts',(-5.73948314349551,-6.17415916067771,
14.9577795955828));
#49356=CARTESIAN_POINT('Ctrl Pts',(-5.73940757545737,-6.75884790405006,
15.5535353523723));
#49357=CARTESIAN_POINT('Ctrl Pts',(-5.7384961905607,-8.05516230656083,16.588732228699));
#49358=CARTESIAN_POINT('Ctrl Pts',(-5.7376603737696,-8.76684603821501,17.0280903673069));
#49359=CARTESIAN_POINT('Ctrl Pts',(-5.73644356975375,-9.52121823634833,
17.3763277339283));
#49360=CARTESIAN_POINT('Origin',(-5.599999999997,-9.67863108576248,17.0348569102134));
#49361=CARTESIAN_POINT('',(-5.593361696257,-9.87744142979155,17.381887715825));
#49362=CARTESIAN_POINT('Origin',(-5.599999999997,-9.67863108576248,17.0348569102134));
#49363=CARTESIAN_POINT('Origin',(-5.6,-9.67863108578652,17.0348569102573));
#49364=CARTESIAN_POINT('Ctrl Pts',(-5.59335880963398,-9.87743876208659,
17.3818891889333));
#49365=CARTESIAN_POINT('Ctrl Pts',(-5.59335897597999,-9.88085962292803,
17.3799294167645));
#49366=CARTESIAN_POINT('Ctrl Pts',(-5.5933624992167,-9.95658496857357,17.3365326542547));
#49367=CARTESIAN_POINT('Ctrl Pts',(-5.5933624992167,-10.0355852075694,17.2909218450052));
#49368=CARTESIAN_POINT('Ctrl Pts',(-5.59335897597999,-10.111030579166,17.2470401532232));
#49369=CARTESIAN_POINT('Ctrl Pts',(-5.59335880963397,-10.1144382220706,
17.2450574869161));
#49370=CARTESIAN_POINT('Ctrl Pts',(-5.83074004398886,-9.87939819740596,
17.385309456316));
#49371=CARTESIAN_POINT('Ctrl Pts',(-5.83074021197022,-9.88281933951952,
17.3833494092227));
#49372=CARTESIAN_POINT('Ctrl Pts',(-5.83074376984249,-9.95855095781758,
17.3399466417508));
#49373=CARTESIAN_POINT('Ctrl Pts',(-5.83074376984249,-10.0375588128472,
17.2943314353822));
#49374=CARTESIAN_POINT('Ctrl Pts',(-5.83074021197022,-10.1130125212199,
17.2504473138048));
#49375=CARTESIAN_POINT('Ctrl Pts',(-5.83074004398886,-10.1164205428521,
17.2484645413711));
#49376=CARTESIAN_POINT('Ctrl Pts',(-6.00000347487355,-9.79664251977179,
17.2408563364913));
#49377=CARTESIAN_POINT('Ctrl Pts',(-6.00000357360975,-9.80004967468002,
17.2389042213875));
#49378=CARTESIAN_POINT('Ctrl Pts',(-6.00000566485702,-9.87547170311362,
17.1956771557035));
#49379=CARTESIAN_POINT('Ctrl Pts',(-6.00000566485702,-9.95415740029349,
17.1502479472561));
#49380=CARTESIAN_POINT('Ctrl Pts',(-6.00000357360975,-10.0293041515222,
17.1065440874721));
#49381=CARTESIAN_POINT('Ctrl Pts',(-6.00000347487355,-10.0326983102474,
17.1045694623189));
#49382=CARTESIAN_POINT('Ctrl Pts',(-5.9999999999769,-9.67862555751017,17.0348533300724));
#49383=CARTESIAN_POINT('Ctrl Pts',(-5.99999999996752,-9.68201281532632,
17.0329126138071));
#49384=CARTESIAN_POINT('Ctrl Pts',(-5.99999999976693,-9.75699439866858,
16.9899379593132));
#49385=CARTESIAN_POINT('Ctrl Pts',(-5.99999999976693,-9.83522068189101,
16.9447739936378));
#49386=CARTESIAN_POINT('Ctrl Pts',(-5.99999999996752,-9.90992861607117,
16.9013253648968));
#49387=CARTESIAN_POINT('Ctrl Pts',(-5.9999999999769,-9.91330295456663,16.8993622717116));
#49388=CARTESIAN_POINT('Origin',(-5.47626352655027,8.61291825284854,-14.9180130853614));
#49389=CARTESIAN_POINT('Ctrl Pts',(-6.00000000001697,-9.67863488304264,
17.0348530242413));
#49390=CARTESIAN_POINT('Ctrl Pts',(-6.00000000001004,-9.68201982098913,
17.0329138284059));
#49391=CARTESIAN_POINT('Ctrl Pts',(-6.00000000000346,-9.68540450273407,
17.0309741411426));
#49392=CARTESIAN_POINT('Ctrl Pts',(-5.9999999999973,-9.68878892524755,17.0290339619835));
#49393=CARTESIAN_POINT('Ctrl Pts',(-5.99999999993208,-9.72458345042307,
17.0085141269222));
#49394=CARTESIAN_POINT('Ctrl Pts',(-5.99999999990817,-9.7603489793636,16.9879392663706));
#49395=CARTESIAN_POINT('Ctrl Pts',(-5.99999999990817,-9.79608195797147,
16.9673088199809));
#49396=CARTESIAN_POINT('Ctrl Pts',(-5.99999999990817,-9.831814800472,16.9466784521728));
#49397=CARTESIAN_POINT('Ctrl Pts',(-5.99999999993208,-9.86751509309911,
16.9259924988281));
#49398=CARTESIAN_POINT('Ctrl Pts',(-5.9999999999973,-9.90318155030038,16.9052543226624));
#49399=CARTESIAN_POINT('Ctrl Pts',(-6.00000000000346,-9.90655401250716,
16.9032934125848));
#49400=CARTESIAN_POINT('Ctrl Pts',(-6.00000000001004,-9.90992617222899,
16.9013320356057));
#49401=CARTESIAN_POINT('Ctrl Pts',(-6.00000000001698,-9.91329802836123,
16.8993701945871));
#49402=CARTESIAN_POINT('Ctrl Pts',(-5.67781977236543,-9.69011180339119,
17.4901976785338));
#49403=CARTESIAN_POINT('Ctrl Pts',(-3.78521318157696,-8.87555307108949,
17.9135245439353));
#49404=CARTESIAN_POINT('Ctrl Pts',(-2.07656941121626E-10,-8.05543132883925,
18.3265320501275));
#49405=CARTESIAN_POINT('Ctrl Pts',(3.7852131811623,-8.87555307099925,17.9135245439808));
#49406=CARTESIAN_POINT('Ctrl Pts',(5.67781977174296,-9.69011180312139,17.4901976786702));
#49407=CARTESIAN_POINT('Ctrl Pts',(-5.67781977236543,-9.88673787499947,
17.3789566884608));
#49408=CARTESIAN_POINT('Ctrl Pts',(-3.78521318157695,-9.58451115251288,
17.5169843132773));
#49409=CARTESIAN_POINT('Ctrl Pts',(-2.07656941988987E-10,-9.35257726240188,
17.7858656006621));
#49410=CARTESIAN_POINT('Ctrl Pts',(3.7852131811623,-9.58451115249001,17.5169843133112));
#49411=CARTESIAN_POINT('Ctrl Pts',(5.67781977174296,-9.8867378749017,17.3789566885092));
#49412=CARTESIAN_POINT('Ctrl Pts',(-5.67781977236543,-10.0824830841441,
17.2660356209527));
#49413=CARTESIAN_POINT('Ctrl Pts',(-3.78521318157695,-10.2888890425898,
17.110829551969));
#49414=CARTESIAN_POINT('Ctrl Pts',(-2.07657304546194E-10,-10.5762499707986,
17.0878203717078));
#49415=CARTESIAN_POINT('Ctrl Pts',(3.7852131811623,-10.288889042623,17.1108295519695));
#49416=CARTESIAN_POINT('Ctrl Pts',(5.67781977174296,-10.0824830842147,17.2660356209062));
#49417=CARTESIAN_POINT('Ctrl Pts',(-5.67781977236543,-10.2772191551084,
17.1515085360387));
#49418=CARTESIAN_POINT('Ctrl Pts',(-3.78521318157695,-10.9872896356005,
16.6958668793638));
#49419=CARTESIAN_POINT('Ctrl Pts',(-2.07657334903855E-10,-11.70142277916,
16.2468455207269));
#49420=CARTESIAN_POINT('Ctrl Pts',(3.7852131811623,-10.9872896356761,16.6958668793104));
#49421=CARTESIAN_POINT('Ctrl Pts',(5.67781977174296,-10.2772191553433,17.1515085358907));
#49422=CARTESIAN_POINT('Ctrl Pts',(-5.59336169625718,-9.87744142978604,
17.3818877158154));
#49423=CARTESIAN_POINT('Ctrl Pts',(-5.58014016745599,-9.87200777751962,
17.3847476856453));
#49424=CARTESIAN_POINT('Ctrl Pts',(-5.56083360318078,-9.86407899010458,
17.3889225081183));
#49425=CARTESIAN_POINT('Ctrl Pts',(-5.53540587426982,-9.8537223397616,17.3943811899286));
#49426=CARTESIAN_POINT('Ctrl Pts',(-5.51006695575766,-9.84340186167177,
17.3998208064221));
#49427=CARTESIAN_POINT('Ctrl Pts',(-5.47864940081797,-9.83067044535519,
17.4065354728229));
#49428=CARTESIAN_POINT('Ctrl Pts',(-5.44109677171059,-9.81563689153736,
17.414473213808));
#49429=CARTESIAN_POINT('Ctrl Pts',(-5.41364441246037,-9.80464680828554,
17.420275995726));
#49430=CARTESIAN_POINT('Ctrl Pts',(-5.38291292798052,-9.79242729789503,
17.4267319893631));
#49431=CARTESIAN_POINT('Ctrl Pts',(-5.34887409163183,-9.77903528808476,
17.4338128228857));
#49432=CARTESIAN_POINT('Ctrl Pts',(-5.3032827335042,-9.76109813215338,17.4432968373704));
#49433=CARTESIAN_POINT('Ctrl Pts',(-5.25175863170486,-9.74105586033139,
17.4539027245749));
#49434=CARTESIAN_POINT('Ctrl Pts',(-5.19421946047611,-9.71908218930116,
17.4655424394124));
#49435=CARTESIAN_POINT('Ctrl Pts',(-5.15775787470716,-9.70515785091014,
17.4729183270348));
#49436=CARTESIAN_POINT('Ctrl Pts',(-5.11888059666409,-9.69045878605213,
17.4807088833052));
#49437=CARTESIAN_POINT('Ctrl Pts',(-5.07756380861576,-9.67503820006752,
17.4888863196405));
#49438=CARTESIAN_POINT('Ctrl Pts',(-5.01427499272364,-9.65141703604609,
17.5014124691102));
#49439=CARTESIAN_POINT('Ctrl Pts',(-4.94526265229308,-9.62610071293147,
17.5148476008571));
#49440=CARTESIAN_POINT('Ctrl Pts',(-4.87043052304886,-9.59931643249468,
17.5290729115528));
#49441=CARTESIAN_POINT('Ctrl Pts',(-4.84061083524584,-9.58864322449272,
17.5347415237937));
#49442=CARTESIAN_POINT('Ctrl Pts',(-4.80986688853492,-9.57773739840919,
17.5405353296213));
#49443=CARTESIAN_POINT('Ctrl Pts',(-4.77819214858275,-9.56661529838823,
17.5464456503157));
#49444=CARTESIAN_POINT('Ctrl Pts',(-4.70105849582066,-9.53953099707122,
17.560838337512));
#49445=CARTESIAN_POINT('Ctrl Pts',(-4.61840565271533,-9.51116108590143,
17.5759237012421));
#49446=CARTESIAN_POINT('Ctrl Pts',(-4.53013308906807,-9.48177309561077,
17.5915603571314));
#49447=CARTESIAN_POINT('Ctrl Pts',(-4.50292731933294,-9.47271566186475,
17.5963796038143));
#49448=CARTESIAN_POINT('Ctrl Pts',(-4.47518769076899,-9.46356184078189,
17.6012510356091));
#49449=CARTESIAN_POINT('Ctrl Pts',(-4.44691113574349,-9.45432033449753,
17.606170015553));
#49450=CARTESIAN_POINT('Ctrl Pts',(-4.35780736095133,-9.42519892653396,
17.6216704780645));
#49451=CARTESIAN_POINT('Ctrl Pts',(-4.26337227850525,-9.39520347024718,
17.6376449404718));
#49452=CARTESIAN_POINT('Ctrl Pts',(-4.16350775218228,-9.3646357796818,17.6539333069341));
#49453=CARTESIAN_POINT('Ctrl Pts',(-4.13544084860851,-9.35604473684446,
17.6585111488136));
#49454=CARTESIAN_POINT('Ctrl Pts',(-4.10694505979946,-9.34740876721134,
17.6631136333997));
#49455=CARTESIAN_POINT('Ctrl Pts',(-4.07801817026704,-9.33873522591717,
17.6677368410205));
#49456=CARTESIAN_POINT('Ctrl Pts',(-3.98951353504935,-9.31219768176034,
17.6818819949114));
#49457=CARTESIAN_POINT('Ctrl Pts',(-3.89697326305071,-9.2853063905167,17.6962222527625));
#49458=CARTESIAN_POINT('Ctrl Pts',(-3.80033518871561,-9.25828974819128,
17.710636274634));
#49459=CARTESIAN_POINT('Ctrl Pts',(-3.7559843940544,-9.24589080952809,17.7172514035949));
#49460=CARTESIAN_POINT('Ctrl Pts',(-3.71077051392982,-9.23346584687373,
17.7238818616415));
#49461=CARTESIAN_POINT('Ctrl Pts',(-3.66468761883613,-9.22103894118868,
17.7305148186855));
#49462=CARTESIAN_POINT('Ctrl Pts',(-3.62894139461506,-9.21139946528144,
17.735659963522));
#49463=CARTESIAN_POINT('Ctrl Pts',(-3.59267228232048,-9.2017588456811,17.7408065977769));
#49464=CARTESIAN_POINT('Ctrl Pts',(-3.5558776755651,-9.19212881406848,17.7459484822605));
#49465=CARTESIAN_POINT('Ctrl Pts',(-3.51376315393471,-9.18110643306174,
17.7518338014526));
#49466=CARTESIAN_POINT('Ctrl Pts',(-3.4709601292138,-9.17009772630246,17.7577130026888));
#49467=CARTESIAN_POINT('Ctrl Pts',(-3.42746486524502,-9.15912127550914,
17.7635761932811));
#49468=CARTESIAN_POINT('Ctrl Pts',(-3.40571723326063,-9.15363305011248,
17.7665077885773));
#49469=CARTESIAN_POINT('Ctrl Pts',(-3.38379654146372,-9.14815288863244,
17.7694353810684));
#49470=CARTESIAN_POINT('Ctrl Pts',(-3.36170232017993,-9.14268316429187,
17.7723577061799));
#49471=CARTESIAN_POINT('Ctrl Pts',(-3.35065520953803,-9.13994830212158,
17.7738188687356));
#49472=CARTESIAN_POINT('Ctrl Pts',(-3.33956471652441,-9.13721604922948,
17.7752787144339));
#49473=CARTESIAN_POINT('Ctrl Pts',(-3.3284307836757,-9.13448670717797,17.776737082515));
#49474=CARTESIAN_POINT('Ctrl Pts',(-3.32286381725134,-9.13312203615221,
17.7774662665555));
#49475=CARTESIAN_POINT('Ctrl Pts',(-3.31728599086821,-9.13175809283616,
17.7781950811909));
#49476=CARTESIAN_POINT('Ctrl Pts',(-3.31169729739565,-9.13039491526983,
17.7789235061383));
#49477=CARTESIAN_POINT('Ctrl Pts',(-3.30610860392309,-9.1290317377035,17.7796519310857));
#49478=CARTESIAN_POINT('Ctrl Pts',(-3.30168365407788,-9.12795439452993,
17.7802276294396));
#49479=CARTESIAN_POINT('Ctrl Pts',(-3.29489860859576,-9.12630771796404,
17.7811075915741));
#49480=CARTESIAN_POINT('Ctrl Pts',(-3.26344298383387,-9.11867368805258,
17.7851871159899));
#49481=CARTESIAN_POINT('Ctrl Pts',(-3.23208742976809,-9.11117310786538,
17.7891959499156));
#49482=CARTESIAN_POINT('Ctrl Pts',(-3.20083332668445,-9.10380424140559,
17.7931349824984));
#49483=CARTESIAN_POINT('Ctrl Pts',(-3.02530585865806,-9.06241964404725,
17.8152571471911));
#49484=CARTESIAN_POINT('Ctrl Pts',(-2.8529813703057,-9.02519047366263,17.835177050746));
#49485=CARTESIAN_POINT('Ctrl Pts',(-2.68409749795662,-8.99178992522898,
17.8530636449176));
#49486=CARTESIAN_POINT('Ctrl Pts',(-2.50184996588225,-8.95574641534673,
17.872365592461));
#49487=CARTESIAN_POINT('Ctrl Pts',(-2.32360980605014,-8.92416076071654,
17.8893000331733));
#49488=CARTESIAN_POINT('Ctrl Pts',(-2.14964334505202,-8.89659253190684,
17.9040958435864));
#49489=CARTESIAN_POINT('Ctrl Pts',(-2.1368280328082,-8.89456170678009,17.9051857831601));
#49490=CARTESIAN_POINT('Ctrl Pts',(-2.12403588914884,-8.89255268013611,
17.9062641193081));
#49491=CARTESIAN_POINT('Ctrl Pts',(-2.11126700969829,-8.89056527486909,
17.9073309444277));
#49492=CARTESIAN_POINT('Ctrl Pts',(-1.93627437198519,-8.86332864136276,
17.9219513770491));
#49493=CARTESIAN_POINT('Ctrl Pts',(-1.76565553955631,-8.8401523257222,17.9344099411939));
#49494=CARTESIAN_POINT('Ctrl Pts',(-1.59964365071508,-8.82055945059309,
17.944954301049));
#49495=CARTESIAN_POINT('Ctrl Pts',(-1.55749255292429,-8.81558473943635,
17.9476315571569));
#49496=CARTESIAN_POINT('Ctrl Pts',(-1.51563819099902,-8.81084107829389,
17.9501854021757));
#49497=CARTESIAN_POINT('Ctrl Pts',(-1.47408386155455,-8.80632074147676,
17.9526198695952));
#49498=CARTESIAN_POINT('Ctrl Pts',(-1.30958959117416,-8.78842682966187,
17.9622567942498));
#49499=CARTESIAN_POINT('Ctrl Pts',(-1.14980067354256,-8.77403078416562,
17.9700237199791));
#49500=CARTESIAN_POINT('Ctrl Pts',(-0.99489992585915,-8.76263900451734,
17.9761777098795));
#49501=CARTESIAN_POINT('Ctrl Pts',(-0.923085664592712,-8.75735760818978,
17.9790307899657));
#49502=CARTESIAN_POINT('Ctrl Pts',(-0.852321370951163,-8.752722228548,17.9815370749662));
#49503=CARTESIAN_POINT('Ctrl Pts',(-0.782621885807213,-8.74868521421749,
17.9837215486527));
#49504=CARTESIAN_POINT('Ctrl Pts',(-0.633275179992519,-8.74003500983875,
17.9884022711622));
#49505=CARTESIAN_POINT('Ctrl Pts',(-0.488819950878624,-8.73412973518557,
17.9916063726453));
#49506=CARTESIAN_POINT('Ctrl Pts',(-0.349378098451702,-8.73049565100499,
17.993578507991));
#49507=CARTESIAN_POINT('Ctrl Pts',(-0.26231014410065,-8.72822651681009,
17.9948099158305));
#49508=CARTESIAN_POINT('Ctrl Pts',(-0.177195960558656,-8.72684351736445,
17.9955607558549));
#49509=CARTESIAN_POINT('Ctrl Pts',(-0.0940577120238034,-8.72623777582956,
17.9958879713096));
#49510=CARTESIAN_POINT('Ctrl Pts',(0.0407719420152373,-8.72525541304196,
17.9964186337583));
#49511=CARTESIAN_POINT('Ctrl Pts',(0.170403009420359,-8.72631553881596,
17.9958365055659));
#49512=CARTESIAN_POINT('Ctrl Pts',(0.294765062228333,-8.72898214507651,
17.9943853356517));
#49513=CARTESIAN_POINT('Ctrl Pts',(0.343253157233777,-8.73002184050436,
17.9938195323131));
#49514=CARTESIAN_POINT('Ctrl Pts',(0.390940632154933,-8.73130611756855,
17.9931213835911));
#49515=CARTESIAN_POINT('Ctrl Pts',(0.437824623194182,-8.73281054765871,
17.9923044400091));
#49516=CARTESIAN_POINT('Ctrl Pts',(0.474197692479818,-8.7339776995733,17.9916706470053));
#49517=CARTESIAN_POINT('Ctrl Pts',(0.510087174592007,-8.73527737333325,
17.9909653435499));
#49518=CARTESIAN_POINT('Ctrl Pts',(0.545492010715984,-8.73669849287197,
17.9901946506401));
#49519=CARTESIAN_POINT('Ctrl Pts',(0.575387451174148,-8.73789847002779,
17.9895438863231));
#49520=CARTESIAN_POINT('Ctrl Pts',(0.604937348457799,-8.73918504043949,
17.9888464976008));
#49521=CARTESIAN_POINT('Ctrl Pts',(0.634141294414872,-8.74055156720631,
17.988106142045));
#49522=CARTESIAN_POINT('Ctrl Pts',(0.666036220849481,-8.74204401178083,
17.9872975668605));
#49523=CARTESIAN_POINT('Ctrl Pts',(0.697518424605556,-8.74363181504274,
17.986437747903));
#49524=CARTESIAN_POINT('Ctrl Pts',(0.728587589446316,-8.74530656799649,
17.9855313071974));
#49525=CARTESIAN_POINT('Ctrl Pts',(0.744122171866696,-8.74614394447337,
17.9850780868446));
#49526=CARTESIAN_POINT('Ctrl Pts',(0.75955349455732,-8.74700305820267,17.9846132107042));
#49527=CARTESIAN_POINT('Ctrl Pts',(0.774881512307569,-8.74788288241698,
17.9841372421394));
#49528=CARTESIAN_POINT('Ctrl Pts',(0.782545521182692,-8.74832279452414,
17.983899257857));
#49529=CARTESIAN_POINT('Ctrl Pts',(0.79018370382266,-8.74876788424227,17.9836585004475));
#49530=CARTESIAN_POINT('Ctrl Pts',(0.797796055871818,-8.74921802409098,
17.9834150397507));
#49531=CARTESIAN_POINT('Ctrl Pts',(0.805408407920975,-8.74966816393968,
17.9831715790539));
#49532=CARTESIAN_POINT('Ctrl Pts',(0.814759539845752,-8.75023074091324,
17.9828673475052));
#49533=CARTESIAN_POINT('Ctrl Pts',(0.820555616113578,-8.75058346697539,
17.9826766173275));
#49534=CARTESIAN_POINT('Ctrl Pts',(0.913356226197327,-8.75623094161981,
17.9796228485315));
#49535=CARTESIAN_POINT('Ctrl Pts',(1.01104127809055,-8.76312889262544,17.9758958258308));
#49536=CARTESIAN_POINT('Ctrl Pts',(1.11355367159285,-8.77158547768657,17.9713324330503));
#49537=CARTESIAN_POINT('Ctrl Pts',(1.22617244491014,-8.78087577131352,17.9663191494896));
#49538=CARTESIAN_POINT('Ctrl Pts',(1.34461811515858,-8.79204710949622,17.9602965148535));
#49539=CARTESIAN_POINT('Ctrl Pts',(1.46878588139576,-8.80553711524201,17.9530327656252));
#49540=CARTESIAN_POINT('Ctrl Pts',(1.51530094558083,-8.81059066901154,17.9503116587565));
#49541=CARTESIAN_POINT('Ctrl Pts',(1.56261868623562,-8.81596996869409,17.9474162054766));
#49542=CARTESIAN_POINT('Ctrl Pts',(1.61073229320877,-8.82169925971597,17.944333619927));
#49543=CARTESIAN_POINT('Ctrl Pts',(1.74015317028542,-8.83711048983832,17.9360417675677));
#49544=CARTESIAN_POINT('Ctrl Pts',(1.87533562169987,-8.85505222115745,17.9263967929664));
#49545=CARTESIAN_POINT('Ctrl Pts',(2.01612326058408,-8.87600820007434,17.9151439566848));
#49546=CARTESIAN_POINT('Ctrl Pts',(2.02944741125243,-8.87799147518787,17.9140789875778));
#49547=CARTESIAN_POINT('Ctrl Pts',(2.04282173407464,-8.88000176774852,17.9129996081194));
#49548=CARTESIAN_POINT('Ctrl Pts',(2.05624607591149,-8.8820394998444,17.9119055968046));
#49549=CARTESIAN_POINT('Ctrl Pts',(2.18614502510105,-8.90175735724116,17.9013195344174));
#49550=CARTESIAN_POINT('Ctrl Pts',(2.32073011534617,-8.92404342112689,17.8893639098098));
#49551=CARTESIAN_POINT('Ctrl Pts',(2.45984826428021,-8.94928033766466,17.8758377542891));
#49552=CARTESIAN_POINT('Ctrl Pts',(2.57756099628316,-8.97063417550504,17.8643928009739));
#49553=CARTESIAN_POINT('Ctrl Pts',(2.69851861493594,-8.99410110387364,17.8518232189882));
#49554=CARTESIAN_POINT('Ctrl Pts',(2.82261224042596,-9.01991399804188,17.8380070639727));
#49555=CARTESIAN_POINT('Ctrl Pts',(2.92930800732048,-9.04210793852974,17.8261279263531));
#49556=CARTESIAN_POINT('Ctrl Pts',(3.03832180266503,-9.06603631713803,17.8133271708017));
#49557=CARTESIAN_POINT('Ctrl Pts',(3.14957564004199,-9.09184572100983,17.7995283192272));
#49558=CARTESIAN_POINT('Ctrl Pts',(3.2464634479155,-9.11432239797324,17.787511291215));
#49559=CARTESIAN_POINT('Ctrl Pts',(3.34504998146593,-9.13822573668744,17.7747372610822));
#49560=CARTESIAN_POINT('Ctrl Pts',(3.44527888894342,-9.16365079871295,17.7611569125572));
#49561=CARTESIAN_POINT('Ctrl Pts',(3.44869579451264,-9.16451756498047,17.7606939446403));
#49562=CARTESIAN_POINT('Ctrl Pts',(3.45211460825154,-9.16538609969273,17.7602300396971));
#49563=CARTESIAN_POINT('Ctrl Pts',(3.455535327867,-9.16625640655736,17.7597651958156));
#49564=CARTESIAN_POINT('Ctrl Pts',(3.53359307397269,-9.186116026728,17.7491578763752));
#49565=CARTESIAN_POINT('Ctrl Pts',(3.61264341668592,-9.20689847768366,17.738061605207));
#49566=CARTESIAN_POINT('Ctrl Pts',(3.69265792828245,-9.22864750213413,17.7264538847221));
#49567=CARTESIAN_POINT('Ctrl Pts',(3.69938882440102,-9.23047705056648,17.7254774323362));
#49568=CARTESIAN_POINT('Ctrl Pts',(3.70612654329246,-9.23231343855504,17.7244973609549));
#49569=CARTESIAN_POINT('Ctrl Pts',(3.71287106704227,-9.2341566918957,17.7235136573507));
#49570=CARTESIAN_POINT('Ctrl Pts',(3.74621479932002,-9.24326941033083,17.7186504007541));
#49571=CARTESIAN_POINT('Ctrl Pts',(3.77972485700455,-9.25254992951069,17.7136983661869));
#49572=CARTESIAN_POINT('Ctrl Pts',(3.81339908956568,-9.26200133171344,17.7086559866148));
#49573=CARTESIAN_POINT('Ctrl Pts',(3.83364189329859,-9.26768291270993,17.7056248291909));
#49574=CARTESIAN_POINT('Ctrl Pts',(3.85394402439297,-9.27342624546287,17.7025610239924));
#49575=CARTESIAN_POINT('Ctrl Pts',(3.87430501375982,-9.27923199511567,17.6994642337049));
#49576=CARTESIAN_POINT('Ctrl Pts',(3.88448550844324,-9.28213486994208,17.6979158385612));
#49577=CARTESIAN_POINT('Ctrl Pts',(3.89468071769478,-9.2850533489971,17.696359197152));
#49578=CARTESIAN_POINT('Ctrl Pts',(3.90489058173839,-9.28798751523955,17.6947942674634));
#49579=CARTESIAN_POINT('Ctrl Pts',(3.9099955137602,-9.28945459836077,17.6940118026191));
#49580=CARTESIAN_POINT('Ctrl Pts',(3.91510410948001,-9.29092560327908,17.6932272657054));
#49581=CARTESIAN_POINT('Ctrl Pts',(3.92021636137619,-9.29240054033904,17.6924406514873));
#49582=CARTESIAN_POINT('Ctrl Pts',(3.92532861327237,-9.29387547739899,17.6916540372692));
#49583=CARTESIAN_POINT('Ctrl Pts',(3.93220897303425,-9.29586539662442,17.6905928060135));
#49584=CARTESIAN_POINT('Ctrl Pts',(3.93556407805506,-9.29683715828189,17.6900745716907));
#49585=CARTESIAN_POINT('Ctrl Pts',(3.94194458963118,-9.29868518881035,17.6890890287421));
#49586=CARTESIAN_POINT('Ctrl Pts',(3.94830740862757,-9.30053254622933,17.6881038759401));
#49587=CARTESIAN_POINT('Ctrl Pts',(3.95465255312891,-9.30237916219918,17.6871191496326));
#49588=CARTESIAN_POINT('Ctrl Pts',(4.02986442886426,-9.32426793885767,17.6754467420683));
#49589=CARTESIAN_POINT('Ctrl Pts',(4.10259295180635,-9.34605169598413,17.6638347266839));
#49590=CARTESIAN_POINT('Ctrl Pts',(4.17286884397023,-9.36762209671566,17.6523407877799));
#49591=CARTESIAN_POINT('Ctrl Pts',(4.24079488558807,-9.38847123704941,17.6412311775238));
#49592=CARTESIAN_POINT('Ctrl Pts',(4.30642960316497,-9.40912113845815,17.6302318353715));
#49593=CARTESIAN_POINT('Ctrl Pts',(4.36980087516246,-9.42948272269656,17.6193901793195));
#49594=CARTESIAN_POINT('Ctrl Pts',(4.43124954177303,-9.44922656185413,17.6088774455956));
#49595=CARTESIAN_POINT('Ctrl Pts',(4.49057003742806,-9.46869938263085,17.5985129410387));
#49596=CARTESIAN_POINT('Ctrl Pts',(4.54778744955938,-9.48782728920201,17.5883359882086));
#49597=CARTESIAN_POINT('Ctrl Pts',(4.60354013708818,-9.50646553512084,17.5784195580521));
#49598=CARTESIAN_POINT('Ctrl Pts',(4.65729604831056,-9.52477635419472,17.5686811746484));
#49599=CARTESIAN_POINT('Ctrl Pts',(4.70907777628743,-9.54269760101514,17.5591538849115));
#49600=CARTESIAN_POINT('Ctrl Pts',(4.75989452685353,-9.56028487677992,17.549804140802));
#49601=CARTESIAN_POINT('Ctrl Pts',(4.80880999465553,-9.57749700556393,17.5406576780202));
#49602=CARTESIAN_POINT('Ctrl Pts',(4.85584473182189,-9.59428067508138,17.5317428072007));
#49603=CARTESIAN_POINT('Ctrl Pts',(4.90206086815699,-9.61077223866507,17.5229830923596));
#49604=CARTESIAN_POINT('Ctrl Pts',(4.94646117235429,-9.62685016187419,17.5144469635652));
#49605=CARTESIAN_POINT('Ctrl Pts',(4.98906423000779,-9.64246863080901,17.5061586889104));
#49606=CARTESIAN_POINT('Ctrl Pts',(4.98944484203018,-9.64260816485599,17.5060846421834));
#49607=CARTESIAN_POINT('Ctrl Pts',(4.98982531060002,-9.64274766226093,17.5060106152213));
#49608=CARTESIAN_POINT('Ctrl Pts',(4.99020563573023,-9.64288712299273,17.5059366080404));
#49609=CARTESIAN_POINT('Ctrl Pts',(5.03327003572535,-9.65867832967558,17.4975567388471));
#49610=CARTESIAN_POINT('Ctrl Pts',(5.07449545385076,-9.67399898203165,17.4894307118898));
#49611=CARTESIAN_POINT('Ctrl Pts',(5.11390005292712,-9.68880632332554,17.4815810747738));
#49612=CARTESIAN_POINT('Ctrl Pts',(5.15370342836636,-9.70376351559733,17.4736519989676));
#49613=CARTESIAN_POINT('Ctrl Pts',(5.19164894890748,-9.71819696689999,17.4660049342146));
#49614=CARTESIAN_POINT('Ctrl Pts',(5.22775413193609,-9.73206714983678,17.4586605744959));
#49615=CARTESIAN_POINT('Ctrl Pts',(5.26453872222235,-9.74619833416345,17.4511780126999));
#49616=CARTESIAN_POINT('Ctrl Pts',(5.2994130686145,-9.75974485716931,17.4440096577332));
#49617=CARTESIAN_POINT('Ctrl Pts',(5.33239434212503,-9.77266950709506,17.4371747702162));
#49618=CARTESIAN_POINT('Ctrl Pts',(5.36640803709531,-9.78599874072917,17.4301259284215));
#49619=CARTESIAN_POINT('Ctrl Pts',(5.39840829740277,-9.7986665527749,17.4234317651715));
#49620=CARTESIAN_POINT('Ctrl Pts',(5.42841238787458,-9.81063699877864,17.4171105675975));
#49621=CARTESIAN_POINT('Ctrl Pts',(5.45995951237177,-9.82322305436067,17.4104642869171));
#49622=CARTESIAN_POINT('Ctrl Pts',(5.48929989813585,-9.83503814518865,17.4042303351122));
#49623=CARTESIAN_POINT('Ctrl Pts',(5.51645165227666,-9.84604608684465,17.3984266695236));
#49624=CARTESIAN_POINT('Ctrl Pts',(5.54440170931256,-9.85737767873876,17.3924523673338));
#49625=CARTESIAN_POINT('Ctrl Pts',(5.57003257818161,-9.86785394712241,17.3869340238601));
#49626=CARTESIAN_POINT('Ctrl Pts',(5.59336165995587,-9.87744149987479,17.3818876747373));
#49627=CARTESIAN_POINT('Ctrl Pts',(-5.8463733386606,-9.55547465583272,17.3476041037463));
#49628=CARTESIAN_POINT('Ctrl Pts',(-5.81071187586262,-9.54063151443765,
17.3552733125109));
#49629=CARTESIAN_POINT('Ctrl Pts',(-5.69191576204028,-9.4916725193938,17.380602960615));
#49630=CARTESIAN_POINT('Ctrl Pts',(-5.48048670779979,-9.40738955295889,
17.4243735747273));
#49631=CARTESIAN_POINT('Ctrl Pts',(-5.20213851496678,-9.30184043404152,
17.4793711370373));
#49632=CARTESIAN_POINT('Ctrl Pts',(-4.89413177237216,-9.19155749159157,
17.5369648709957));
#49633=CARTESIAN_POINT('Ctrl Pts',(-4.55275559255447,-9.07723151098239,
17.5967689263156));
#49634=CARTESIAN_POINT('Ctrl Pts',(-4.17237668547323,-8.95957536536919,
17.6583990236104));
#49635=CARTESIAN_POINT('Ctrl Pts',(-3.74657700614932,-8.84000925011093,
17.7211108191622));
#49636=CARTESIAN_POINT('Ctrl Pts',(-3.27005258562448,-8.72141473082344,
17.783401453449));
#49637=CARTESIAN_POINT('Ctrl Pts',(-2.73873739986321,-8.60813796297983,
17.8430033606407));
#49638=CARTESIAN_POINT('Ctrl Pts',(-2.14785706271427,-8.50557223079316,
17.8970963536719));
#49639=CARTESIAN_POINT('Ctrl Pts',(-1.4967968550619,-8.42118487526943,17.9417530293261));
#49640=CARTESIAN_POINT('Ctrl Pts',(-0.805603071092674,-8.36491582767002,
17.9716807938175));
#49641=CARTESIAN_POINT('Ctrl Pts',(-0.113474661740786,-8.34312739996358,
17.9833785830982));
#49642=CARTESIAN_POINT('Ctrl Pts',(0.536087305492918,-8.35364335445179,
17.9777186569795));
#49643=CARTESIAN_POINT('Ctrl Pts',(1.11980900607103,-8.38850996828337,17.9591202910325));
#49644=CARTESIAN_POINT('Ctrl Pts',(1.636919179711,-8.43934018271074,17.9321437718199));
#49645=CARTESIAN_POINT('Ctrl Pts',(2.09765854466679,-8.50038395982727,17.8998516626081));
#49646=CARTESIAN_POINT('Ctrl Pts',(2.51230476687163,-8.56810866040446,17.8641104411872));
#49647=CARTESIAN_POINT('Ctrl Pts',(2.88629849960366,-8.63961055570718,17.8264433928252));
#49648=CARTESIAN_POINT('Ctrl Pts',(3.22331998694596,-8.71249671744812,17.7881005995987));
#49649=CARTESIAN_POINT('Ctrl Pts',(3.52773839095892,-8.7852276671472,17.7498824286448));
#49650=CARTESIAN_POINT('Ctrl Pts',(3.80298126733865,-8.85663091467915,17.7123972644307));
#49651=CARTESIAN_POINT('Ctrl Pts',(4.05169100707615,-8.92576431324658,17.6761335665833));
#49652=CARTESIAN_POINT('Ctrl Pts',(4.27621239277721,-8.99193794361065,17.6414484058552));
#49653=CARTESIAN_POINT('Ctrl Pts',(4.47890149179128,-9.05474661932589,17.6085504399071));
#49654=CARTESIAN_POINT('Ctrl Pts',(4.66211487979546,-9.11402962441174,17.5775210304017));
#49655=CARTESIAN_POINT('Ctrl Pts',(4.82817101282,-9.16982306444236,17.548339195531));
#49656=CARTESIAN_POINT('Ctrl Pts',(4.97931089694066,-9.22231312182208,17.5209060859325));
#49657=CARTESIAN_POINT('Ctrl Pts',(5.11759928752743,-9.2717709266513,17.495079082544));
#49658=CARTESIAN_POINT('Ctrl Pts',(5.24463817723889,-9.31841704262003,17.4707425653601));
#49659=CARTESIAN_POINT('Ctrl Pts',(5.36152006758449,-9.36236512845068,17.4478370666325));
#49660=CARTESIAN_POINT('Ctrl Pts',(5.46894627430349,-9.40363534662726,17.42635189288));
#49661=CARTESIAN_POINT('Ctrl Pts',(5.5675550051916,-9.44226364631247,17.4062679240946));
#49662=CARTESIAN_POINT('Ctrl Pts',(5.65799001946662,-9.47832302411334,17.387546454043));
#49663=CARTESIAN_POINT('Ctrl Pts',(5.74089747013883,-9.5119186332035,17.3701316688078));
#49664=CARTESIAN_POINT('Ctrl Pts',(5.80283354338081,-9.5373887531129,17.356951424237));
#49665=CARTESIAN_POINT('Ctrl Pts',(5.8372084201771,-9.55166080740083,17.3495754016711));
#49666=CARTESIAN_POINT('Ctrl Pts',(5.84634761756587,-9.55546494241973,17.3476100580218));
#49667=CARTESIAN_POINT('Ctrl Pts',(-5.81214108390672,-9.67762768152041,
17.422552109006));
#49668=CARTESIAN_POINT('Ctrl Pts',(-5.77669442398367,-9.66284839961546,
17.4302152968869));
#49669=CARTESIAN_POINT('Ctrl Pts',(-5.6586054670479,-9.61409646251181,17.4555271005114));
#49670=CARTESIAN_POINT('Ctrl Pts',(-5.4483945072021,-9.53015286520016,17.4992766414301));
#49671=CARTESIAN_POINT('Ctrl Pts',(-5.17161296303814,-9.42501288020989,
17.5542583452189));
#49672=CARTESIAN_POINT('Ctrl Pts',(-4.86532906973079,-9.3151511687536,17.6118418521599));
#49673=CARTESIAN_POINT('Ctrl Pts',(-4.5258683630326,-9.20126101315959,17.6716394125171));
#49674=CARTESIAN_POINT('Ctrl Pts',(-4.14764202883284,-9.08405588457841,
17.73326560891));
#49675=CARTESIAN_POINT('Ctrl Pts',(-3.72427988122061,-8.96495263246336,
17.7959753909885));
#49676=CARTESIAN_POINT('Ctrl Pts',(-3.25051918720775,-8.84682286565692,
17.8582653016694));
#49677=CARTESIAN_POINT('Ctrl Pts',(-2.72232654864596,-8.7339958797264,17.9178671153977));
#49678=CARTESIAN_POINT('Ctrl Pts',(-2.1349611118646,-8.63184254874727,17.9719599109248));
#49679=CARTESIAN_POINT('Ctrl Pts',(-1.48780923344429,-8.54779798948218,
18.0166156513017));
#49680=CARTESIAN_POINT('Ctrl Pts',(-0.800784407919693,-8.49175868625974,
18.0465417244253));
#49681=CARTESIAN_POINT('Ctrl Pts',(-0.112803388434847,-8.47005849434548,
18.0582381566499));
#49682=CARTESIAN_POINT('Ctrl Pts',(0.532891166728138,-8.48053201472142,
18.0525789661958));
#49683=CARTESIAN_POINT('Ctrl Pts',(1.11309345819553,-8.51525647368222,18.0339820169203));
#49684=CARTESIAN_POINT('Ctrl Pts',(1.62709043164589,-8.56587948303477,18.0070066017781));
#49685=CARTESIAN_POINT('Ctrl Pts',(2.08506564285918,-8.62667559462568,17.974715114357));
#49686=CARTESIAN_POINT('Ctrl Pts',(2.49723975402976,-8.69412739933001,17.9389741366442));
#49687=CARTESIAN_POINT('Ctrl Pts',(2.86902032483964,-8.76534345922683,17.9013071615013));
#49688=CARTESIAN_POINT('Ctrl Pts',(3.20406354354222,-8.83794065763298,17.8629644838458));
#49689=CARTESIAN_POINT('Ctrl Pts',(3.50670973291176,-8.91038560785036,17.8247466485053));
#49690=CARTESIAN_POINT('Ctrl Pts',(3.78036309777869,-8.98151023781651,17.7872621736466));
#49691=CARTESIAN_POINT('Ctrl Pts',(4.02764738382,-9.05037575367207,17.750999611039));
#49692=CARTESIAN_POINT('Ctrl Pts',(4.25089072086612,-9.11629450106337,17.7163160896842));
#49693=CARTESIAN_POINT('Ctrl Pts',(4.45243283978244,-9.17886240441804,17.6834203038348));
#49694=CARTESIAN_POINT('Ctrl Pts',(4.63461440918886,-9.23791890672294,17.6523936427792));
#49695=CARTESIAN_POINT('Ctrl Pts',(4.79973861820133,-9.29349953159147,17.6232151550724));
#49696=CARTESIAN_POINT('Ctrl Pts',(4.9500320169126,-9.34578932814734,17.5957860347958));
#49697=CARTESIAN_POINT('Ctrl Pts',(5.08754619050864,-9.39505798668279,17.5699637272056));
#49698=CARTESIAN_POINT('Ctrl Pts',(5.21387275743999,-9.44152482985382,17.5456326932636));
#49699=CARTESIAN_POINT('Ctrl Pts',(5.33009684078889,-9.4853026874993,17.5227335504965));
#49700=CARTESIAN_POINT('Ctrl Pts',(5.43691472795915,-9.52641127632892,17.501255677646));
#49701=CARTESIAN_POINT('Ctrl Pts',(5.53496016576123,-9.56488609405541,17.4811800103912));
#49702=CARTESIAN_POINT('Ctrl Pts',(5.62487271584546,-9.60079963775867,17.4624678661905));
#49703=CARTESIAN_POINT('Ctrl Pts',(5.70729474319025,-9.63425659180306,17.4450633926373));
#49704=CARTESIAN_POINT('Ctrl Pts',(5.76886296772336,-9.65961934027998,17.4318922291228));
#49705=CARTESIAN_POINT('Ctrl Pts',(5.80303184039065,-9.67383042396305,17.4245217359534));
#49706=CARTESIAN_POINT('Ctrl Pts',(5.81211616128011,-9.67761826069822,17.4225578918343));
#49707=CARTESIAN_POINT('Ctrl Pts',(-5.75637793437334,-9.81403840381243,
17.4252871466828));
#49708=CARTESIAN_POINT('Ctrl Pts',(-5.72124343449299,-9.79938715618852,
17.4329279577232));
#49709=CARTESIAN_POINT('Ctrl Pts',(-5.6041894339736,-9.75105556027103,17.4581672492143));
#49710=CARTESIAN_POINT('Ctrl Pts',(-5.39579946274376,-9.66782737176423,
17.501797818414));
#49711=CARTESIAN_POINT('Ctrl Pts',(-5.12141106912661,-9.56358205149893,
17.5566355014982));
#49712=CARTESIAN_POINT('Ctrl Pts',(-4.81780022720726,-9.45466429365216,
17.6140695093037));
#49713=CARTESIAN_POINT('Ctrl Pts',(-4.48134885127786,-9.34176852335966,
17.6737106747822));
#49714=CARTESIAN_POINT('Ctrl Pts',(-4.10654179458656,-9.22560739565263,
17.7351728067037));
#49715=CARTESIAN_POINT('Ctrl Pts',(-3.68709221215214,-9.10758918936382,
17.7977114360113));
#49716=CARTESIAN_POINT('Ctrl Pts',(-3.21781356780073,-8.99056166571874,
17.859826087837));
#49717=CARTESIAN_POINT('Ctrl Pts',(-2.69473704827974,-8.87881314592504,
17.9192542591247));
#49718=CARTESIAN_POINT('Ctrl Pts',(-2.11318875262544,-8.77765876537053,
17.97318332707));
#49719=CARTESIAN_POINT('Ctrl Pts',(-1.47256892305503,-8.69445237153633,
18.017698294401));
#49720=CARTESIAN_POINT('Ctrl Pts',(-0.792573669743242,-8.6389796067912,
18.0475260652017));
#49721=CARTESIAN_POINT('Ctrl Pts',(-0.111652214361621,-8.61749917698253,
18.0591824466625));
#49722=CARTESIAN_POINT('Ctrl Pts',(0.527433781118694,-8.62786675128895,
18.0535427952304));
#49723=CARTESIAN_POINT('Ctrl Pts',(1.10168186396621,-8.66223950646855,18.0350078632655));
#49724=CARTESIAN_POINT('Ctrl Pts',(1.6104437947622,-8.71235326743348,18.0081196177625));
#49725=CARTESIAN_POINT('Ctrl Pts',(2.06380279066605,-8.77254445237208,17.9759294726917));
#49726=CARTESIAN_POINT('Ctrl Pts',(2.471875939082,-8.8393339587489,17.9402975746886));
#49727=CARTESIAN_POINT('Ctrl Pts',(2.84000970754068,-8.90986088796221,17.9027425846969));
#49728=CARTESIAN_POINT('Ctrl Pts',(3.17181456380946,-8.98176608815248,17.8645111850715));
#49729=CARTESIAN_POINT('Ctrl Pts',(3.47157828024225,-9.05353078406801,17.8264018584624));
#49730=CARTESIAN_POINT('Ctrl Pts',(3.74266244641465,-9.12399725049448,17.7890217327069));
#49731=CARTESIAN_POINT('Ctrl Pts',(3.98765665383845,-9.19223432334608,17.7528583757986));
#49732=CARTESIAN_POINT('Ctrl Pts',(4.20885881341848,-9.25755929255515,17.7182683265255));
#49733=CARTESIAN_POINT('Ctrl Pts',(4.40857962993792,-9.31957027594431,17.6854600901218));
#49734=CARTESIAN_POINT('Ctrl Pts',(4.58913208163627,-9.3781067089517,17.6545151837928));
#49735=CARTESIAN_POINT('Ctrl Pts',(4.75279328253527,-9.43320245485805,17.6254130205343));
#49736=CARTESIAN_POINT('Ctrl Pts',(4.90176552988434,-9.48503972981198,17.5980553273719));
#49737=CARTESIAN_POINT('Ctrl Pts',(5.03807866068162,-9.53388480985318,17.5723001660497));
#49738=CARTESIAN_POINT('Ctrl Pts',(5.16330731160006,-9.57995417027385,17.548032522943));
#49739=CARTESIAN_POINT('Ctrl Pts',(5.27852455024402,-9.62335879843351,17.5251933812032));
#49740=CARTESIAN_POINT('Ctrl Pts',(5.38441837965784,-9.66411743944915,17.5037723401632));
#49741=CARTESIAN_POINT('Ctrl Pts',(5.4816151955655,-9.70226458024048,17.4837505483551));
#49742=CARTESIAN_POINT('Ctrl Pts',(5.5707476032503,-9.73787152713718,17.4650895405272));
#49743=CARTESIAN_POINT('Ctrl Pts',(5.65245152948686,-9.7710416913486,17.4477336532073));
#49744=CARTESIAN_POINT('Ctrl Pts',(5.71348061603488,-9.79618593614716,17.4346000847585));
#49745=CARTESIAN_POINT('Ctrl Pts',(5.74734932939181,-9.81027420187925,17.4272509118054));
#49746=CARTESIAN_POINT('Ctrl Pts',(5.7563538024379,-9.81402928407118,17.4252927635236));
#49747=CARTESIAN_POINT('Ctrl Pts',(-5.69417905513898,-9.9277103189944,17.3549354620686));
#49748=CARTESIAN_POINT('Ctrl Pts',(-5.65936952811319,-9.91321664820986,
17.362543583712));
#49749=CARTESIAN_POINT('Ctrl Pts',(-5.54339798862242,-9.86540498256572,
17.3876752760031));
#49750=CARTESIAN_POINT('Ctrl Pts',(-5.33693877355696,-9.78307476204316,
17.431121086189));
#49751=CARTESIAN_POINT('Ctrl Pts',(-5.06512202552609,-9.67996770527826,
17.48572544092));
#49752=CARTESIAN_POINT('Ctrl Pts',(-4.76441068914013,-9.5722613821277,17.5429109986631));
#49753=CARTESIAN_POINT('Ctrl Pts',(-4.43124774750502,-9.46064969374635,
17.6022880427151));
#49754=CARTESIAN_POINT('Ctrl Pts',(-4.06020097215969,-9.34584328386552,
17.6634701828468));
#49755=CARTESIAN_POINT('Ctrl Pts',(-3.64507978641427,-9.22923895256998,
17.7257146637894));
#49756=CARTESIAN_POINT('Ctrl Pts',(-3.180788195249,-9.1136531696858,17.7875267698037));
#49757=CARTESIAN_POINT('Ctrl Pts',(-2.66343645887594,-9.00332024433173,
17.8466545610653));
#49758=CARTESIAN_POINT('Ctrl Pts',(-2.0884329388477,-8.90348131169733,17.9003005100313));
#49759=CARTESIAN_POINT('Ctrl Pts',(-1.45520082765633,-8.82138187250908,
17.9445728184062));
#49760=CARTESIAN_POINT('Ctrl Pts',(-0.783193111485207,-8.76665929244331,
17.974232179735));
#49761=CARTESIAN_POINT('Ctrl Pts',(-0.110332699532594,-8.74547074609478,
17.9858206162357));
#49762=CARTESIAN_POINT('Ctrl Pts',(0.521192190350527,-8.75569750097974,
17.9802140384361));
#49763=CARTESIAN_POINT('Ctrl Pts',(1.08866283073277,-8.7896040759372,17.961785002976));
#49764=CARTESIAN_POINT('Ctrl Pts',(1.59148482702499,-8.83904420757627,17.9350464911301));
#49765=CARTESIAN_POINT('Ctrl Pts',(2.03962503535982,-8.89843673409496,17.9030310875698));
#49766=CARTESIAN_POINT('Ctrl Pts',(2.44307842316623,-8.9643535814534,17.8675876986891));
#49767=CARTESIAN_POINT('Ctrl Pts',(2.80711889697381,-9.03397438360193,17.8302264162518));
#49768=CARTESIAN_POINT('Ctrl Pts',(3.13530190870835,-9.1049716283224,17.7921874581311));
#49769=CARTESIAN_POINT('Ctrl Pts',(3.43185318841762,-9.17584572137997,17.7542655605531));
#49770=CARTESIAN_POINT('Ctrl Pts',(3.70008397692616,-9.24545241579932,17.7170653115438));
#49771=CARTESIAN_POINT('Ctrl Pts',(3.94254344408661,-9.31287039114815,17.6810724844686));
#49772=CARTESIAN_POINT('Ctrl Pts',(4.16149389258016,-9.37742322400891,17.6466425384257));
#49773=CARTESIAN_POINT('Ctrl Pts',(4.35921216621147,-9.4387117148047,17.613983614923));
#49774=CARTESIAN_POINT('Ctrl Pts',(4.53797926335854,-9.49657512665328,17.583177424839));
#49775=CARTESIAN_POINT('Ctrl Pts',(4.70004247198356,-9.55104503278127,17.5542039813712));
#49776=CARTESIAN_POINT('Ctrl Pts',(4.84757660412767,-9.60229988245748,17.5269658902415));
#49777=CARTESIAN_POINT('Ctrl Pts',(4.98258705753238,-9.65060148608525,17.5013222155595));
#49778=CARTESIAN_POINT('Ctrl Pts',(5.10662947642265,-9.69616263511548,17.4771587717524));
#49779=CARTESIAN_POINT('Ctrl Pts',(5.22076345927117,-9.73909195903942,17.4544170892153));
#49780=CARTESIAN_POINT('Ctrl Pts',(5.32566771121937,-9.77940696831178,17.4330870766611));
#49781=CARTESIAN_POINT('Ctrl Pts',(5.4219603766622,-9.81714085302345,17.413150195144));
#49782=CARTESIAN_POINT('Ctrl Pts',(5.51026622868089,-9.8523633594578,17.3945683316977));
#49783=CARTESIAN_POINT('Ctrl Pts',(5.59121384820522,-9.88517616538835,17.3772861883258));
#49784=CARTESIAN_POINT('Ctrl Pts',(5.65167852005776,-9.91004987479868,17.3642085773892));
#49785=CARTESIAN_POINT('Ctrl Pts',(5.68523421205636,-9.9239866959767,17.3568907578296));
#49786=CARTESIAN_POINT('Ctrl Pts',(5.69415549150679,-9.92770142712335,17.3549409634383));
#49787=CARTESIAN_POINT('',(5.7364427498306,-9.52121898129658,17.3763264188218));
#49788=CARTESIAN_POINT('Origin',(5.599999999773,-9.67863108544441,17.0348569101661));
#49789=CARTESIAN_POINT('Ctrl Pts',(-5.73644387793042,-9.52121721533639,
17.3763301032685));
#49790=CARTESIAN_POINT('Ctrl Pts',(-5.66411038162322,-9.49169730087515,
17.3916242108731));
#49791=CARTESIAN_POINT('Ctrl Pts',(-5.58548128683522,-9.46019526466375,
17.407976703292));
#49792=CARTESIAN_POINT('Ctrl Pts',(-5.50055659194694,-9.42702544965956,
17.4252224559801));
#49793=CARTESIAN_POINT('Ctrl Pts',(-5.41741954382298,-9.39455385220615,
17.4421051892423));
#49794=CARTESIAN_POINT('Ctrl Pts',(-5.3282491481451,-9.3604841148662,17.4598438858076));
#49795=CARTESIAN_POINT('Ctrl Pts',(-5.23304540339397,-9.32515773279535,
17.4782590776983));
#49796=CARTESIAN_POINT('Ctrl Pts',(-5.13477099393748,-9.28869194728111,
17.4972682260551));
#49797=CARTESIAN_POINT('Ctrl Pts',(-5.03006776433377,-9.25088687600408,
17.5169983552411));
#49798=CARTESIAN_POINT('Ctrl Pts',(-4.9189357129117,-9.21216968518984,17.537224895896));
#49799=CARTESIAN_POINT('Ctrl Pts',(-4.80780366148964,-9.17345249437559,
17.557451436551));
#49800=CARTESIAN_POINT('Ctrl Pts',(-4.69024278824921,-9.13382318061147,
17.5781743903966));
#49801=CARTESIAN_POINT('Ctrl Pts',(-4.56625309151927,-9.09376132461316,
17.5991415631926));
#49802=CARTESIAN_POINT('Ctrl Pts',(-4.44622752890923,-9.05498030544612,
17.6194383844411));
#49803=CARTESIAN_POINT('Ctrl Pts',(-4.32017765149417,-9.01579421513404,
17.6399639238612));
#49804=CARTESIAN_POINT('Ctrl Pts',(-4.18810345927408,-8.97668492680345,
17.6604647283727));
#49805=CARTESIAN_POINT('Ctrl Pts',(-4.05161756545643,-8.93626926281454,
17.6816503255034));
#49806=CARTESIAN_POINT('Ctrl Pts',(-3.90869817218809,-8.89593533402846,
17.7028096566685));
#49807=CARTESIAN_POINT('Ctrl Pts',(-3.75934527946908,-8.856266693735,17.7236357378929));
#49808=CARTESIAN_POINT('Ctrl Pts',(-3.60999238675007,-8.81659805344155,
17.7444618191173));
#49809=CARTESIAN_POINT('Ctrl Pts',(-3.45420599458039,-8.77759469628942,
17.7649546527636));
#49810=CARTESIAN_POINT('Ctrl Pts',(-3.29198610296003,-8.73989286152806,
17.7847794985823));
#49811=CARTESIAN_POINT('Ctrl Pts',(-3.21175007622309,-8.72124505334789,
17.7945851200957));
#49812=CARTESIAN_POINT('Ctrl Pts',(-3.12994014689571,-8.70291646379771,
17.8042268961841));
#49813=CARTESIAN_POINT('Ctrl Pts',(-3.04655631966383,-8.68498886666937,
17.8136618172413));
#49814=CARTESIAN_POINT('Ctrl Pts',(-3.00486440604789,-8.67602506810521,
17.8183792777699));
#49815=CARTESIAN_POINT('Ctrl Pts',(-2.96277900922897,-8.66716153817332,
17.8230449853729));
#49816=CARTESIAN_POINT('Ctrl Pts',(-2.92030014046422,-8.65840882966546,
17.8276534235764));
#49817=CARTESIAN_POINT('Ctrl Pts',(-2.89906070608185,-8.65403247541154,
17.8299576426782));
#49818=CARTESIAN_POINT('Ctrl Pts',(-2.87772290314608,-8.64968382778711,
17.8322475419892));
#49819=CARTESIAN_POINT('Ctrl Pts',(-2.85628673150918,-8.64536421936501,
17.834522419904));
#49820=CARTESIAN_POINT('Ctrl Pts',(-2.84556864569073,-8.64320441515397,
17.8356598588614));
#49821=CARTESIAN_POINT('Ctrl Pts',(-2.83482596766454,-8.64105187082454,
17.836793542316));
#49822=CARTESIAN_POINT('Ctrl Pts',(-2.82405869742173,-8.63890675413443,
17.8379233819689));
#49823=CARTESIAN_POINT('Ctrl Pts',(-2.81867506230032,-8.63783419578937,
17.8384883017953));
#49824=CARTESIAN_POINT('Ctrl Pts',(-2.81328527912276,-8.63676349435921,
17.8390522606617));
#49825=CARTESIAN_POINT('Ctrl Pts',(-2.80788934788906,-8.63569467088992,
17.8396152474944));
#49826=CARTESIAN_POINT('Ctrl Pts',(-2.80249341665537,-8.63462584742063,
17.8401782343271));
#49827=CARTESIAN_POINT('Ctrl Pts',(-2.79531838615154,-8.63320975323161,
17.8409241692332));
#49828=CARTESIAN_POINT('Ctrl Pts',(-2.79168311001559,-8.63249385544467,
17.8413012807856));
#49829=CARTESIAN_POINT('Ctrl Pts',(-2.04607521596783,-8.48566070678899,
17.9186481837106));
#49830=CARTESIAN_POINT('Ctrl Pts',(-1.30047967324348,-8.39780990969505,
17.9651212818614));
#49831=CARTESIAN_POINT('Ctrl Pts',(-0.55486679613319,-8.36896299940472,
17.9806923161373));
#49832=CARTESIAN_POINT('Ctrl Pts',(-0.369912415081077,-8.36180732572766,
17.9845548178393));
#49833=CARTESIAN_POINT('Ctrl Pts',(-0.184956967406051,-8.35828253263868,
17.986515779255));
#49834=CARTESIAN_POINT('Ctrl Pts',(-7.72943142945967E-13,-8.35838942589688,
17.9865746356273));
#49835=CARTESIAN_POINT('Ctrl Pts',(6.96532233517991E-5,-8.35838946615197,
17.9865746577921));
#49836=CARTESIAN_POINT('Ctrl Pts',(0.000139306447692276,-8.35838950692212,
17.9865746796872));
#49837=CARTESIAN_POINT('Ctrl Pts',(0.000208959672248314,-8.35838954820731,
17.9865747013125));
#49838=CARTESIAN_POINT('Ctrl Pts',(0.465533924648662,-8.35866535788534,
17.9867191711212));
#49839=CARTESIAN_POINT('Ctrl Pts',(0.930858888603267,-8.38166467718553,
17.9746778420633));
#49840=CARTESIAN_POINT('Ctrl Pts',(1.39618385153606,-8.42737858503983,17.9504582799483));
#49841=CARTESIAN_POINT('Ctrl Pts',(1.62884633300245,-8.45023553896698,17.9383484988907));
#49842=CARTESIAN_POINT('Ctrl Pts',(1.86150881432015,-8.47877078912326,17.9231942078017));
#49843=CARTESIAN_POINT('Ctrl Pts',(2.09417129412707,-8.51298109397737,17.9049966542053));
#49844=CARTESIAN_POINT('Ctrl Pts',(2.21050253403054,-8.53008624640443,17.8958978774071));
#49845=CARTESIAN_POINT('Ctrl Pts',(2.32683377547297,-8.54861015630717,17.8860382965441));
#49846=CARTESIAN_POINT('Ctrl Pts',(2.44316501613488,-8.5685522661496,17.8754180780318));
#49847=CARTESIAN_POINT('Ctrl Pts',(2.50133063646584,-8.57852332107081,17.8701079687756));
#49848=CARTESIAN_POINT('Ctrl Pts',(2.55949625670459,-8.58884892557739,17.864607700846));
#49849=CARTESIAN_POINT('Ctrl Pts',(2.61766187686913,-8.59952900439952,17.8589172978087));
#49850=CARTESIAN_POINT('Ctrl Pts',(2.64674468695139,-8.60486904381058,17.8560720962901));
#49851=CARTESIAN_POINT('Ctrl Pts',(2.67582749702413,-8.61029770177647,17.8531793610399));
#49852=CARTESIAN_POINT('Ctrl Pts',(2.70491030708909,-8.61581496835059,17.8502390950788));
#49853=CARTESIAN_POINT('Ctrl Pts',(2.73217544152499,-8.62098740576383,17.8474825957402));
#49854=CARTESIAN_POINT('Ctrl Pts',(2.75944057595433,-8.62623772183578,17.8446843213643));
#49855=CARTESIAN_POINT('Ctrl Pts',(2.78670571038341,-8.63156590812219,17.8418442744992));
#49856=CARTESIAN_POINT('Ctrl Pts',(2.78852338601201,-8.63192112054128,17.8416549380415));
#49857=CARTESIAN_POINT('Ctrl Pts',(2.79172337447383,-8.63254733872129,17.8413211462471));
#49858=CARTESIAN_POINT('Ctrl Pts',(2.79215873726898,-8.63263258364449,17.8412757081596));
#49859=CARTESIAN_POINT('Ctrl Pts',(2.80635256732739,-8.63541176451781,17.8397943218317));
#49860=CARTESIAN_POINT('Ctrl Pts',(2.82657169823296,-8.63939985249501,17.8376810545087));
#49861=CARTESIAN_POINT('Ctrl Pts',(2.85281612998569,-8.6446742432296,17.8348952271828));
#49862=CARTESIAN_POINT('Ctrl Pts',(2.87906085573414,-8.64994869304904,17.8321093686494));
#49863=CARTESIAN_POINT('Ctrl Pts',(2.91133101732391,-8.65650947442629,17.8286509348427));
#49864=CARTESIAN_POINT('Ctrl Pts',(2.94962661475501,-8.66448013438173,17.8244550000515));
#49865=CARTESIAN_POINT('Ctrl Pts',(2.98792266551261,-8.67245088869036,17.8202590155906));
#49866=CARTESIAN_POINT('Ctrl Pts',(3.03224429476531,-8.68183155489256,17.8153255123835));
#49867=CARTESIAN_POINT('Ctrl Pts',(3.08259150251312,-8.69279183462203,17.8095653204095));
#49868=CARTESIAN_POINT('Ctrl Pts',(3.13293969676294,-8.70375232910697,17.8038050155705));
#49869=CARTESIAN_POINT('Ctrl Pts',(3.18931370564027,-8.71629249885724,17.797217989197));
#49870=CARTESIAN_POINT('Ctrl Pts',(3.2517135291451,-8.73062820904404,17.7896908282125));
#49871=CARTESIAN_POINT('Ctrl Pts',(3.31411405755573,-8.74496408117561,17.7821635821966));
#49872=CARTESIAN_POINT('Ctrl Pts',(3.38254053673707,-8.76109553416888,17.7736961798243));
#49873=CARTESIAN_POINT('Ctrl Pts',(3.45699296668911,-8.77928459686504,17.7641509726701));
#49874=CARTESIAN_POINT('Ctrl Pts',(3.53144681502674,-8.79747400607916,17.7546055836711));
#49875=CARTESIAN_POINT('Ctrl Pts',(3.61192684373679,-8.81772110315139,17.7439823482514));
#49876=CARTESIAN_POINT('Ctrl Pts',(3.69843305281927,-8.84033409273623,17.732119385857));
#49877=CARTESIAN_POINT('Ctrl Pts',(3.77372916539131,-8.86001672855428,17.7217937114186));
#49878=CARTESIAN_POINT('Ctrl Pts',(3.85359082346075,-8.88149251454903,17.7105284259308));
#49879=CARTESIAN_POINT('Ctrl Pts',(3.93801802702761,-8.90499316277047,17.6982018453617));
#49880=CARTESIAN_POINT('Ctrl Pts',(3.98561695038899,-8.91824251258163,17.6912522848051));
#49881=CARTESIAN_POINT('Ctrl Pts',(4.03466705650711,-8.93213595430368,17.6839651349225));
#49882=CARTESIAN_POINT('Ctrl Pts',(4.08516835096818,-8.94671873895556,17.676316648598));
#49883=CARTESIAN_POINT('Ctrl Pts',(4.11041899819872,-8.95401013128149,17.6724924054358));
#49884=CARTESIAN_POINT('Ctrl Pts',(4.13603243296646,-8.9614738754163,17.6685777961487));
#49885=CARTESIAN_POINT('Ctrl Pts',(4.16200866737389,-8.96911590964012,17.6645697329619));
#49886=CARTESIAN_POINT('Ctrl Pts',(4.17499678457761,-8.97293692675204,17.6625657013686));
#49887=CARTESIAN_POINT('Ctrl Pts',(4.18807560110365,-8.97680251739733,17.660538304294));
#49888=CARTESIAN_POINT('Ctrl Pts',(4.20124511680291,-8.98071343504126,17.6584871457692));
#49889=CARTESIAN_POINT('Ctrl Pts',(4.20782987465255,-8.98266889386323,17.6574615665068));
#49890=CARTESIAN_POINT('Ctrl Pts',(4.21443730725747,-8.98463568449712,17.6564300467572));
#49891=CARTESIAN_POINT('Ctrl Pts',(4.22106741461914,-8.9866139021614,17.6553925365324));
#49892=CARTESIAN_POINT('Ctrl Pts',(4.22769752198081,-8.98859211982568,17.6543550263075));
#49893=CARTESIAN_POINT('Ctrl Pts',(4.23593900697649,-8.99105802557391,17.6530617434669));
#49894=CARTESIAN_POINT('Ctrl Pts',(4.24102576089831,-8.99258293191174,17.6522619840224));
#49895=CARTESIAN_POINT('Ctrl Pts',(4.37039703482885,-9.03136583326327,17.6319217238558));
#49896=CARTESIAN_POINT('Ctrl Pts',(4.49374245266343,-9.07012830039618,17.61160848498));
#49897=CARTESIAN_POINT('Ctrl Pts',(4.61106201570063,-9.10839870848643,17.5915703319006));
#49898=CARTESIAN_POINT('Ctrl Pts',(4.72934461225931,-9.14698326440435,17.5713676929279));
#49899=CARTESIAN_POINT('Ctrl Pts',(4.84150201989796,-9.18506758915995,17.5514447066701));
#49900=CARTESIAN_POINT('Ctrl Pts',(4.9475342399474,-9.22221578420815,17.5320306005081));
#49901=CARTESIAN_POINT('Ctrl Pts',(5.05275997752547,-9.25908142959233,17.5127641582951));
#49902=CARTESIAN_POINT('Ctrl Pts',(5.15195334967944,-9.29502519376288,17.4939988518562));
#49903=CARTESIAN_POINT('Ctrl Pts',(5.24511435771002,-9.32966737365834,17.4759343044898));
#49904=CARTESIAN_POINT('Ctrl Pts',(5.33934638774133,-9.36470781606304,17.4576620787386));
#49905=CARTESIAN_POINT('Ctrl Pts',(5.42740655466849,-9.3984164865661,17.4401068637726));
#49906=CARTESIAN_POINT('Ctrl Pts',(5.50929485983757,-9.43044842471371,17.4234499554535));
#49907=CARTESIAN_POINT('Ctrl Pts',(5.59118316500664,-9.46248036286132,17.4067930471343));
#49908=CARTESIAN_POINT('Ctrl Pts',(5.66689960841764,-9.4928355706219,17.3910344443383));
#49909=CARTESIAN_POINT('Ctrl Pts',(5.73644419141664,-9.52121731728258,17.3763300250081));
#49910=CARTESIAN_POINT('Origin',(5.6,-9.67863108576213,17.0348569102136));
#49911=CARTESIAN_POINT('Origin',(5.59997427801229,-9.67865015413163,17.0348418886071));
#49912=CARTESIAN_POINT('Ctrl Pts',(5.7176130128486,-3.68945532772947,9.84748761497653));
#49913=CARTESIAN_POINT('Ctrl Pts',(5.72101169066759,-3.69017805224285,9.84586230390886));
#49914=CARTESIAN_POINT('Ctrl Pts',(5.76688773959286,-3.70048425892532,9.8236880828416));
#49915=CARTESIAN_POINT('Ctrl Pts',(5.85062090523121,-3.73363357303796,9.7770831424454));
#49916=CARTESIAN_POINT('Ctrl Pts',(5.94915275497326,-3.81230845463928,9.70513932835593));
#49917=CARTESIAN_POINT('Ctrl Pts',(6.01699168753275,-3.91212539537255,9.63586548676976));
#49918=CARTESIAN_POINT('Ctrl Pts',(6.04750393498136,-4.01010954209592,9.58182952763555));
#49919=CARTESIAN_POINT('Ctrl Pts',(6.05138588436001,-4.07133194826796,9.55406663714884));
#49920=CARTESIAN_POINT('Ctrl Pts',(6.05073510899355,-4.09501988092087,9.54419767224957));
#49921=CARTESIAN_POINT('Ctrl Pts',(5.60116392361712,-3.61346410389966,9.56401900963965));
#49922=CARTESIAN_POINT('Ctrl Pts',(5.6043354827448,-3.6141179583603,9.56250546762696));
#49923=CARTESIAN_POINT('Ctrl Pts',(5.64715015969186,-3.62344889768341,9.54185530555744));
#49924=CARTESIAN_POINT('Ctrl Pts',(5.72539812923533,-3.65363741952875,9.49843452207815));
#49925=CARTESIAN_POINT('Ctrl Pts',(5.81747684225603,-3.72555031859565,9.43152778111091));
#49926=CARTESIAN_POINT('Ctrl Pts',(5.88071656821272,-3.81671595959616,9.36742946903526));
#49927=CARTESIAN_POINT('Ctrl Pts',(5.90899203942426,-3.90581940681478,9.31789944012116));
#49928=CARTESIAN_POINT('Ctrl Pts',(5.91255165229384,-3.96110742538711,9.29277836968071));
#49929=CARTESIAN_POINT('Ctrl Pts',(5.91195414402012,-3.98242656800513,9.28390550969072));
#49930=CARTESIAN_POINT('Ctrl Pts',(5.58625429018143,-3.33992185286638,9.4070408693956));
#49931=CARTESIAN_POINT('Ctrl Pts',(5.59076091566283,-3.34085079789971,9.4049216144276));
#49932=CARTESIAN_POINT('Ctrl Pts',(5.65155980037929,-3.35409562789098,9.37603625759484));
#49933=CARTESIAN_POINT('Ctrl Pts',(5.76176077930928,-3.39659253349918,9.31602842442839));
#49934=CARTESIAN_POINT('Ctrl Pts',(5.89142705504701,-3.49725390257798,9.22407233768376));
#49935=CARTESIAN_POINT('Ctrl Pts',(5.98187551871793,-3.62620437369158,9.13484987539963));
#49936=CARTESIAN_POINT('Ctrl Pts',(6.02382013630363,-3.75573644179709,9.0635694766303));
#49937=CARTESIAN_POINT('Ctrl Pts',(6.02944021185559,-3.83935013265183,9.02565148550328));
#49938=CARTESIAN_POINT('Ctrl Pts',(6.02850383718158,-3.87220383486143,9.0119569801733));
#49939=CARTESIAN_POINT('Ctrl Pts',(5.68265567725631,-3.04810711614505,9.47943574065643));
#49940=CARTESIAN_POINT('Ctrl Pts',(5.68918455596363,-3.04947481887442,9.47639027304701));
#49941=CARTESIAN_POINT('Ctrl Pts',(5.77722643655303,-3.06895754584997,9.43490778788664));
#49942=CARTESIAN_POINT('Ctrl Pts',(5.93587673121703,-3.13096513514427,9.3494127976663));
#49943=CARTESIAN_POINT('Ctrl Pts',(6.12253650192003,-3.27704376992711,9.21873820754285));
#49944=CARTESIAN_POINT('Ctrl Pts',(6.25416912891128,-3.46545114247581,9.09055820339493));
#49945=CARTESIAN_POINT('Ctrl Pts',(6.31673010125175,-3.65822436169862,8.98552625787696));
#49946=CARTESIAN_POINT('Ctrl Pts',(6.32544301813554,-3.78585922915993,8.92775966642298));
#49947=CARTESIAN_POINT('Ctrl Pts',(6.32399773550576,-3.83659112696463,8.90658585651305));
#49948=CARTESIAN_POINT('',(5.99998069488466,-3.99788653537587,9.34660672384924));
#49949=CARTESIAN_POINT('',(5.99999998706781,-3.21424121943635,9.2921838327228));
#49950=CARTESIAN_POINT('Ctrl Pts',(5.99998069488466,-3.99788653537587,9.34660672384924));
#49951=CARTESIAN_POINT('Ctrl Pts',(5.99997825547866,-3.97544692625939,9.33725008234246));
#49952=CARTESIAN_POINT('Ctrl Pts',(5.99997953090646,-3.95288229363252,9.32837835501087));
#49953=CARTESIAN_POINT('Ctrl Pts',(5.99999093101457,-3.93025585224078,9.32009551206795));
#49954=CARTESIAN_POINT('Ctrl Pts',(5.99999583058559,-3.92053139566385,9.31653568818149));
#49955=CARTESIAN_POINT('Ctrl Pts',(6.00000208202755,-3.91079590771391,9.313084395188));
#49956=CARTESIAN_POINT('Ctrl Pts',(6.0000083910374,-3.90105617909432,9.3097484395143));
#49957=CARTESIAN_POINT('Ctrl Pts',(6.00002365440229,-3.87749288859613,9.30167777392408));
#49958=CARTESIAN_POINT('Ctrl Pts',(6.00004122708332,-3.85390258847053,9.29428474465244));
#49959=CARTESIAN_POINT('Ctrl Pts',(6.00006097205355,-3.83038110088263,9.28763749735748));
#49960=CARTESIAN_POINT('Ctrl Pts',(6.00007474334107,-3.81397585110789,9.28300132152971));
#49961=CARTESIAN_POINT('Ctrl Pts',(6.00008877497374,-3.79760486147016,9.2787272046869));
#49962=CARTESIAN_POINT('Ctrl Pts',(6.00009896189812,-3.78130850697401,9.27482624452034));
#49963=CARTESIAN_POINT('Ctrl Pts',(6.00011392971824,-3.75736399796689,9.26909449783633));
#49964=CARTESIAN_POINT('Ctrl Pts',(6.00011947181448,-3.73358031968664,9.26417081834576));
#49965=CARTESIAN_POINT('Ctrl Pts',(6.0001068790683,-3.71010072455357,9.26004886835312));
#49966=CARTESIAN_POINT('Ctrl Pts',(6.00010389446192,-3.70453582642796,9.25907192511121));
#49967=CARTESIAN_POINT('Ctrl Pts',(6.00009995311129,-3.698988058318,9.258139800092));
#49968=CARTESIAN_POINT('Ctrl Pts',(6.00009507698778,-3.69345939306189,9.25725200972086));
#49969=CARTESIAN_POINT('Ctrl Pts',(6.00008968453197,-3.68734529793109,9.25627021130589));
#49970=CARTESIAN_POINT('Ctrl Pts',(6.00008315014167,-3.68125456446157,9.2553426362406));
#49971=CARTESIAN_POINT('Ctrl Pts',(6.00007576287927,-3.67518971333856,9.25446844767461));
#49972=CARTESIAN_POINT('Ctrl Pts',(6.00006006901019,-3.66230524080158,9.25261127783775));
#49973=CARTESIAN_POINT('Ctrl Pts',(6.00004619203746,-3.64934307924697,9.25096136123653));
#49974=CARTESIAN_POINT('Ctrl Pts',(6.00002901871136,-3.63653958486174,9.24955726473395));
#49975=CARTESIAN_POINT('Ctrl Pts',(6.00001169308667,-3.62362254495518,9.24814071625034));
#49976=CARTESIAN_POINT('Ctrl Pts',(5.9999905602067,-3.61086748883357,9.2469745209682));
#49977=CARTESIAN_POINT('Ctrl Pts',(5.99997298498214,-3.5985341229454,9.24604863264794));
#49978=CARTESIAN_POINT('Ctrl Pts',(5.99996108050175,-3.59018018631326,9.24542148735557));
#49979=CARTESIAN_POINT('Ctrl Pts',(5.99995110675469,-3.58202007426576,9.24490350011415));
#49980=CARTESIAN_POINT('Ctrl Pts',(5.99994986561638,-3.57413696972424,9.24447901888708));
#49981=CARTESIAN_POINT('Ctrl Pts',(5.99994572912138,-3.54786397313808,9.24306429785034));
#49982=CARTESIAN_POINT('Ctrl Pts',(5.99996726956826,-3.52150110691479,9.24259411083022));
#49983=CARTESIAN_POINT('Ctrl Pts',(5.99999448700643,-3.49521226937049,9.24315082110635));
#49984=CARTESIAN_POINT('Ctrl Pts',(6.0000217044446,-3.46892343182619,9.24370753138247));
#49985=CARTESIAN_POINT('Ctrl Pts',(6.00005373135004,-3.44270963425123,9.24529169775039));
#49986=CARTESIAN_POINT('Ctrl Pts',(6.00007304312752,-3.41676089682398,9.24793117163163));
#49987=CARTESIAN_POINT('Ctrl Pts',(6.00009158147329,-3.39185139963973,9.25046493526453));
#49988=CARTESIAN_POINT('Ctrl Pts',(6.00009812241609,-3.36718699899513,9.25397091649523));
#49989=CARTESIAN_POINT('Ctrl Pts',(6.00009050007888,-3.34294012363997,9.25842391697067));
#49990=CARTESIAN_POINT('Ctrl Pts',(6.00008278309713,-3.31839218126482,9.26293220917188));
#49991=CARTESIAN_POINT('Ctrl Pts',(6.00006013980506,-3.29427323053127,9.26841096327143));
#49992=CARTESIAN_POINT('Ctrl Pts',(6.00003725529026,-3.27075809151588,9.27478305130894));
#49993=CARTESIAN_POINT('Ctrl Pts',(6.00001849832783,-3.25148424705605,9.28000584134386));
#49994=CARTESIAN_POINT('Ctrl Pts',(5.99999989152894,-3.23261615806335,9.2858276417319));
#49995=CARTESIAN_POINT('Ctrl Pts',(5.99999989737976,-3.21424117270406,9.29218369762246));
#49996=CARTESIAN_POINT('',(5.72001574683959,-3.07996623050488,9.45352741085221));
#49997=CARTESIAN_POINT('Ctrl Pts',(5.72001583932757,-3.07996630534764,9.45352764057597));
#49998=CARTESIAN_POINT('Ctrl Pts',(5.77275232442229,-3.09393993078643,9.42774314696833));
#49999=CARTESIAN_POINT('Ctrl Pts',(5.82234187961538,-3.11241974313512,9.40135240094038));
#50000=CARTESIAN_POINT('Ctrl Pts',(5.86896567632587,-3.13488603146277,9.37445534842813));
#50001=CARTESIAN_POINT('Ctrl Pts',(5.91558947303636,-3.15735231979043,9.34755829591588));
#50002=CARTESIAN_POINT('Ctrl Pts',(5.95924775859859,-3.18380528255528,9.3201555191835));
#50003=CARTESIAN_POINT('Ctrl Pts',(6.00000001914382,-3.21424127110487,9.29218398209336));
#50004=CARTESIAN_POINT('',(5.732784907806,-3.68906816095735,9.81544004097578));
#50005=CARTESIAN_POINT('Origin',(5.89877293621907,-3.22461215454891,9.89752349969974));
#50006=CARTESIAN_POINT('Ctrl Pts',(5.7327825100706,-3.68907486546999,9.81543885690915));
#50007=CARTESIAN_POINT('Ctrl Pts',(5.74764948384582,-3.69180670821221,9.80080167796743));
#50008=CARTESIAN_POINT('Ctrl Pts',(5.76167658134928,-3.69530452754189,9.78635735023664));
#50009=CARTESIAN_POINT('Ctrl Pts',(5.77486160049988,-3.69936666582116,9.77221490407054));
#50010=CARTESIAN_POINT('Ctrl Pts',(5.78891900853863,-3.70369757612544,9.75713672070559));
#50011=CARTESIAN_POINT('Ctrl Pts',(5.80201936622981,-3.70867022853965,9.74240158470817));
#50012=CARTESIAN_POINT('Ctrl Pts',(5.81418801307471,-3.71408129430063,9.72810973814384));
#50013=CARTESIAN_POINT('Ctrl Pts',(5.81740490064576,-3.71551175657096,9.72433156427077));
#50014=CARTESIAN_POINT('Ctrl Pts',(5.8205568113287,-3.7169730546453,9.72058421196347));
#50015=CARTESIAN_POINT('Ctrl Pts',(5.82364449135978,-3.71846183295476,9.71686920835376));
#50016=CARTESIAN_POINT('Ctrl Pts',(5.83601524515966,-3.72442660577562,9.70198508999997));
#50017=CARTESIAN_POINT('Ctrl Pts',(5.84735402368391,-3.73082847913117,9.68762273979523));
#50018=CARTESIAN_POINT('Ctrl Pts',(5.85773994244867,-3.73744892184006,9.6738670485));
#50019=CARTESIAN_POINT('Ctrl Pts',(5.86865590927978,-3.7444072405651,9.6594093319206));
#50020=CARTESIAN_POINT('Ctrl Pts',(5.87851959247198,-3.75160756637909,9.6456214755469));
#50021=CARTESIAN_POINT('Ctrl Pts',(5.88743536558818,-3.75884759269843,9.63256909564335));
#50022=CARTESIAN_POINT('Ctrl Pts',(5.89158024689428,-3.76221343089952,9.62650113442928));
#50023=CARTESIAN_POINT('Ctrl Pts',(5.8955204092406,-3.76558850460084,9.62059170537446));
#50024=CARTESIAN_POINT('Ctrl Pts',(5.89926696894881,-3.76895557030682,9.61484542094946));
#50025=CARTESIAN_POINT('Ctrl Pts',(5.90175393687619,-3.77119062995416,9.61103103490477));
#50026=CARTESIAN_POINT('Ctrl Pts',(5.90415560487913,-3.77342219894787,9.60728851115445));
#50027=CARTESIAN_POINT('Ctrl Pts',(5.90647529181436,-3.77564564485586,9.60361893755839));
#50028=CARTESIAN_POINT('Ctrl Pts',(5.90966133214877,-3.77869950020014,9.59857885680029));
#50029=CARTESIAN_POINT('Ctrl Pts',(5.91269274269099,-3.78173796382313,9.59367641974815));
#50030=CARTESIAN_POINT('Ctrl Pts',(5.91557902779535,-3.78474891647479,9.58891407316326));
#50031=CARTESIAN_POINT('Ctrl Pts',(5.91807289117107,-3.78735049749416,9.5847992191897));
#50032=CARTESIAN_POINT('Ctrl Pts',(5.92045834780138,-3.78993149928615,9.58078901354365));
#50033=CARTESIAN_POINT('Ctrl Pts',(5.92274147618617,-3.79248497313327,9.57688456026381));
#50034=CARTESIAN_POINT('Ctrl Pts',(5.92388304037856,-3.79376171005683,9.57493233362389));
#50035=CARTESIAN_POINT('Ctrl Pts',(5.92499901532196,-3.79503156983948,9.57300654433216));
#50036=CARTESIAN_POINT('Ctrl Pts',(5.92609014106788,-3.79629373914138,9.57110731271001));
#50037=CARTESIAN_POINT('Ctrl Pts',(5.92686106600724,-3.79718551334446,9.56976542793769));
#50038=CARTESIAN_POINT('Ctrl Pts',(5.92731171353663,-3.79771183702838,9.56897640141495));
#50039=CARTESIAN_POINT('Ctrl Pts',(5.92809603246344,-3.7986380362319,9.56759650003687));
#50040=CARTESIAN_POINT('Ctrl Pts',(5.92842179641288,-3.79902272962663,9.56702336313122));
#50041=CARTESIAN_POINT('Ctrl Pts',(5.92880480754124,-3.79947665663788,9.56634829711098));
#50042=CARTESIAN_POINT('Ctrl Pts',(5.92928969071536,-3.80005638685381,9.56548940150969));
#50043=CARTESIAN_POINT('Ctrl Pts',(5.93928521267292,-3.81200711315668,9.54778387923122));
#50044=CARTESIAN_POINT('Ctrl Pts',(5.94806892639471,-3.82437504732193,9.53071818637277));
#50045=CARTESIAN_POINT('Ctrl Pts',(5.95571469163255,-3.83695616247855,9.51437147298147));
#50046=CARTESIAN_POINT('Ctrl Pts',(5.95896087035118,-3.84229775315098,9.50743111430189));
#50047=CARTESIAN_POINT('Ctrl Pts',(5.96200197167069,-3.84767833832296,9.50061999222101));
#50048=CARTESIAN_POINT('Ctrl Pts',(5.96484395211758,-3.85308457920931,9.49394263078481));
#50049=CARTESIAN_POINT('Ctrl Pts',(5.97172175150301,-3.86616807536293,9.47778293044895));
#50050=CARTESIAN_POINT('Ctrl Pts',(5.97743430190242,-3.87939847007179,9.46240829174299));
#50051=CARTESIAN_POINT('Ctrl Pts',(5.98211309003572,-3.89258616441926,9.44786214539775));
#50052=CARTESIAN_POINT('Ctrl Pts',(5.98709331622123,-3.90662349606251,9.43237884141757));
#50053=CARTESIAN_POINT('Ctrl Pts',(5.99090179182026,-3.92061275286255,9.41783420575638));
#50054=CARTESIAN_POINT('Ctrl Pts',(5.99369013037234,-3.9343760335644,9.40425257196093));
#50055=CARTESIAN_POINT('Ctrl Pts',(5.99430533024733,-3.93741266932761,9.40125601352407));
#50056=CARTESIAN_POINT('Ctrl Pts',(5.99487086199565,-3.94043847980818,9.39830623162827));
#50057=CARTESIAN_POINT('Ctrl Pts',(5.99538834779487,-3.94345183865437,9.39540332080571));
#50058=CARTESIAN_POINT('Ctrl Pts',(5.99774241059584,-3.95715972392664,9.38219786784031));
#50059=CARTESIAN_POINT('Ctrl Pts',(5.99910410221826,-3.97060616074746,9.36996372163261));
#50060=CARTESIAN_POINT('Ctrl Pts',(5.99967027283376,-3.98363782450936,9.35869135705663));
#50061=CARTESIAN_POINT('Ctrl Pts',(5.99987914390199,-3.98844545220349,9.35453276816853));
#50062=CARTESIAN_POINT('Ctrl Pts',(5.99997953584385,-3.99319708251765,9.35050490868574));
#50063=CARTESIAN_POINT('Ctrl Pts',(5.99998069488466,-3.99788653537587,9.34660672384923));
#50064=CARTESIAN_POINT('Ctrl Pts',(5.99970218902464,-4.00041486383445,9.24574070855039));
#50065=CARTESIAN_POINT('Ctrl Pts',(5.99970218902464,-4.05365231287788,9.67397466963937));
#50066=CARTESIAN_POINT('Ctrl Pts',(5.99970218902464,-4.23216229704141,10.6067282950652));
#50067=CARTESIAN_POINT('Ctrl Pts',(5.99970218902464,-4.7103395450234,11.9928022384675));
#50068=CARTESIAN_POINT('Ctrl Pts',(5.99970218902464,-5.43783918301558,13.3613505076908));
#50069=CARTESIAN_POINT('Ctrl Pts',(5.99970218902464,-6.36842741850186,14.5997819466434));
#50070=CARTESIAN_POINT('Ctrl Pts',(5.99970218902464,-7.48063208193852,15.6796604855679));
#50071=CARTESIAN_POINT('Ctrl Pts',(5.99970218902464,-8.63550391275622,16.4940252554982));
#50072=CARTESIAN_POINT('Ctrl Pts',(5.99970218902464,-9.43064084707896,16.9071646182876));
#50073=CARTESIAN_POINT('Ctrl Pts',(5.99970218902464,-9.77579624509523,17.06208514011));
#50074=CARTESIAN_POINT('Ctrl Pts',(6.00690499952675,-3.81528531867719,9.26875000770376));
#50075=CARTESIAN_POINT('Ctrl Pts',(6.00690499952675,-3.86952777852313,9.7050827268058));
#50076=CARTESIAN_POINT('Ctrl Pts',(6.00690499952675,-4.05137912813777,10.6553011459376));
#50077=CARTESIAN_POINT('Ctrl Pts',(6.00690499952675,-4.53860924447568,12.067600402351));
#50078=CARTESIAN_POINT('Ctrl Pts',(6.00690499952675,-5.27974784182031,13.4618117081885));
#50079=CARTESIAN_POINT('Ctrl Pts',(6.00690499952675,-6.22793540867418,14.7236676441621));
#50080=CARTESIAN_POINT('Ctrl Pts',(6.00690499952675,-7.36100880388284,15.8238001511061));
#50081=CARTESIAN_POINT('Ctrl Pts',(6.00690499952675,-8.5377034970597,16.6535599584588));
#50082=CARTESIAN_POINT('Ctrl Pts',(6.00690499952675,-9.3477361651398,17.0744403871867));
#50083=CARTESIAN_POINT('Ctrl Pts',(6.00690499952675,-9.69940847689799,17.2322837299283));
#50084=CARTESIAN_POINT('Ctrl Pts',(5.89977162083546,-3.66341997502774,9.2876249804719));
#50085=CARTESIAN_POINT('Ctrl Pts',(5.89977162083546,-3.71848686465799,9.73060126728731));
#50086=CARTESIAN_POINT('Ctrl Pts',(5.89977162083546,-3.90307920092505,10.6951463942138));
#50087=CARTESIAN_POINT('Ctrl Pts',(5.89977162083546,-4.39773556012829,12.1289587817135));
#50088=CARTESIAN_POINT('Ctrl Pts',(5.89977162083546,-5.1500624594129,13.5442219724419));
#50089=CARTESIAN_POINT('Ctrl Pts',(5.89977162083546,-6.11268709790595,14.8252934760138));
#50090=CARTESIAN_POINT('Ctrl Pts',(5.89977162083546,-7.26287951709116,15.9420407043495));
#50091=CARTESIAN_POINT('Ctrl Pts',(5.89977162083546,-8.45747592600413,16.7844293584207));
#50092=CARTESIAN_POINT('Ctrl Pts',(5.89977162083546,-9.27972785235618,17.2116599331396));
#50093=CARTESIAN_POINT('Ctrl Pts',(5.89977162083546,-9.63674611439996,17.3719009223656));
#50094=CARTESIAN_POINT('Ctrl Pts',(5.72171418897201,-3.60697683468152,9.29464016057385));
#50095=CARTESIAN_POINT('Ctrl Pts',(5.72171418897201,-3.66235013659085,9.74008563368347));
#50096=CARTESIAN_POINT('Ctrl Pts',(5.72171418897201,-3.84796120360022,10.709955506594));
#50097=CARTESIAN_POINT('Ctrl Pts',(5.72171418897201,-4.34537764260743,12.1517635871689));
#50098=CARTESIAN_POINT('Ctrl Pts',(5.72171418897201,-5.10186285004451,13.5748510415821));
#50099=CARTESIAN_POINT('Ctrl Pts',(5.72171418897201,-6.0698532529814,14.8630643126808));
#50100=CARTESIAN_POINT('Ctrl Pts',(5.72171418897201,-7.22640822631808,15.9859866631895));
#50101=CARTESIAN_POINT('Ctrl Pts',(5.72171418897201,-8.42765808906915,16.8330690265054));
#50102=CARTESIAN_POINT('Ctrl Pts',(5.72171418897201,-9.25445149468778,17.2626597327244));
#50103=CARTESIAN_POINT('Ctrl Pts',(5.72171418897201,-9.61345666312839,17.4237918449321));
#50104=CARTESIAN_POINT('Ctrl Pts',(5.73278343891033,-3.68907227129128,9.81543931495127));
#50105=CARTESIAN_POINT('Ctrl Pts',(5.73338951195738,-3.73677169448297,10.0841578313552));
#50106=CARTESIAN_POINT('Ctrl Pts',(5.73395354731066,-3.79517193860139,10.3512383428457));
#50107=CARTESIAN_POINT('Ctrl Pts',(5.73447555432297,-3.86412900186718,10.6157493871671));
#50108=CARTESIAN_POINT('Ctrl Pts',(5.73532470053474,-3.97630111386147,11.0460281879475));
#50109=CARTESIAN_POINT('Ctrl Pts',(5.7360626339114,-4.11640867475991,11.4695101586091));
#50110=CARTESIAN_POINT('Ctrl Pts',(5.73668941370095,-4.28354705454678,11.8826222728609));
#50111=CARTESIAN_POINT('Ctrl Pts',(5.73681689631878,-4.31754182998523,11.9666463825406));
#50112=CARTESIAN_POINT('Ctrl Pts',(5.73693978068686,-4.3526547996942,12.0502413363141));
#50113=CARTESIAN_POINT('Ctrl Pts',(5.73705806732598,-4.38887829682059,12.1333768104643));
#50114=CARTESIAN_POINT('Ctrl Pts',(5.73707478352026,-4.39399737891054,12.1451254639772));
#50115=CARTESIAN_POINT('Ctrl Pts',(5.73709140789253,-4.39913863949845,12.1568649410002));
#50116=CARTESIAN_POINT('Ctrl Pts',(5.73710794044422,-4.40430204004992,12.1685951618524));
#50117=CARTESIAN_POINT('Ctrl Pts',(5.73767502814514,-4.58141329317504,12.5709567632529));
#50118=CARTESIAN_POINT('Ctrl Pts',(5.73813408876969,-4.78457571005312,12.9624318070339));
#50119=CARTESIAN_POINT('Ctrl Pts',(5.73848518363096,-5.01222351458537,13.3397802002642));
#50120=CARTESIAN_POINT('Ctrl Pts',(5.73855071722427,-5.05471510385475,13.4102141452326));
#50121=CARTESIAN_POINT('Ctrl Pts',(5.73861248923238,-5.09805970732631,13.4801557828557));
#50122=CARTESIAN_POINT('Ctrl Pts',(5.73867049997421,-5.14224706204589,13.5495838576326));
#50123=CARTESIAN_POINT('Ctrl Pts',(5.73897977963041,-5.3778284292935,13.9197341163462));
#50124=CARTESIAN_POINT('Ctrl Pts',(5.73918215131397,-5.6373663945189,14.2752903707391));
#50125=CARTESIAN_POINT('Ctrl Pts',(5.73927764639914,-5.91884406793555,14.6132515745047));
#50126=CARTESIAN_POINT('Ctrl Pts',(5.73929840900891,-5.98004314514966,14.6867313413138));
#50127=CARTESIAN_POINT('Ctrl Pts',(5.73931411925514,-6.04227924864683,14.7593791926461));
#50128=CARTESIAN_POINT('Ctrl Pts',(5.73932477725726,-6.10553147686454,14.8311640048254));
#50129=CARTESIAN_POINT('Ctrl Pts',(5.739373586197,-6.39519872996674,15.1599067217915));
#50130=CARTESIAN_POINT('Ctrl Pts',(5.73931644036589,-6.70617912931026,15.4705526572465));
#50131=CARTESIAN_POINT('Ctrl Pts',(5.73915333068962,-7.03611036566116,15.7604173878931));
#50132=CARTESIAN_POINT('Ctrl Pts',(5.7391174737338,-7.10864027337172,15.8241393391545));
#50133=CARTESIAN_POINT('Ctrl Pts',(5.73907649576432,-7.18208588698078,15.8868568479539));
#50134=CARTESIAN_POINT('Ctrl Pts',(5.7390303964735,-7.2564218957479,15.9485411327689));
#50135=CARTESIAN_POINT('Ctrl Pts',(5.73900084502645,-7.3040741825488,15.988083170065));
#50136=CARTESIAN_POINT('Ctrl Pts',(5.73896918906768,-7.3520923590695,16.02720062128));
#50137=CARTESIAN_POINT('Ctrl Pts',(5.73893542850084,-7.40046852267685,16.065887648773));
#50138=CARTESIAN_POINT('Ctrl Pts',(5.73869640199973,-7.74297417965619,16.3397937376393));
#50139=CARTESIAN_POINT('Ctrl Pts',(5.73835187101066,-8.10342818285287,16.5921266953169));
#50140=CARTESIAN_POINT('Ctrl Pts',(5.73790180004051,-8.47900260085346,16.8207961663496));
#50141=CARTESIAN_POINT('Ctrl Pts',(5.73786596894725,-8.50890286745421,16.8390010222174));
#50142=CARTESIAN_POINT('Ctrl Pts',(5.73782946892097,-8.53889894702324,16.8570558798847));
#50143=CARTESIAN_POINT('Ctrl Pts',(5.73779229993823,-8.56898940139243,16.8749596757298));
#50144=CARTESIAN_POINT('Ctrl Pts',(5.73741169656715,-8.87710997742077,17.058291167545));
#50145=CARTESIAN_POINT('Ctrl Pts',(5.73696095093767,-9.19512783840813,17.2257844016345));
#50146=CARTESIAN_POINT('Ctrl Pts',(5.73644003523888,-9.52122270930497,17.3763183336115));
#50147=CARTESIAN_POINT('Ctrl Pts',(5.99999999930593,-3.99788653301806,9.34660672531438));
#50148=CARTESIAN_POINT('Ctrl Pts',(5.99999999931563,-4.01825012982366,9.49792584373936));
#50149=CARTESIAN_POINT('Ctrl Pts',(5.9999999983592,-4.04202369729047,9.6482576246397));
#50150=CARTESIAN_POINT('Ctrl Pts',(5.99999999609539,-4.06917084355555,9.79770305083865));
#50151=CARTESIAN_POINT('Ctrl Pts',(5.99999999382037,-4.09645246638317,9.94788877242653));
#50152=CARTESIAN_POINT('Ctrl Pts',(5.99999999024014,-4.12714128052617,10.0971797858705));
#50153=CARTESIAN_POINT('Ctrl Pts',(5.9999999903916,-4.16125231177404,10.2456707880721));
#50154=CARTESIAN_POINT('Ctrl Pts',(5.99999999048551,-4.1824037372745,10.3377464672779));
#50155=CARTESIAN_POINT('Ctrl Pts',(5.99999999231395,-4.20487200130163,10.429514367737));
#50156=CARTESIAN_POINT('Ctrl Pts',(5.9999999950529,-4.22867039396756,10.520994409904));
#50157=CARTESIAN_POINT('Ctrl Pts',(5.99999999721691,-4.24747319330309,10.5932715968644));
#50158=CARTESIAN_POINT('Ctrl Pts',(5.99999999999964,-4.26710645549874,10.6653690537662));
#50159=CARTESIAN_POINT('Ctrl Pts',(5.99999999999964,-4.28757894249402,10.7372995926901));
#50160=CARTESIAN_POINT('Ctrl Pts',(5.99999999999964,-4.33786650262272,10.913986054968));
#50161=CARTESIAN_POINT('Ctrl Pts',(5.99999998462024,-4.39314035947195,11.0896695374196));
#50162=CARTESIAN_POINT('Ctrl Pts',(5.99999998025194,-4.45330084831765,11.2638532253973));
#50163=CARTESIAN_POINT('Ctrl Pts',(5.99999997588668,-4.51341958947054,11.4379160405689));
#50164=CARTESIAN_POINT('Ctrl Pts',(5.99999998175302,-4.57841806285475,11.6104807002592));
#50165=CARTESIAN_POINT('Ctrl Pts',(5.99999999007194,-4.64814658232175,11.7810647426391));
#50166=CARTESIAN_POINT('Ctrl Pts',(5.99999999337619,-4.6758425268787,11.8488201778063));
#50167=CARTESIAN_POINT('Ctrl Pts',(5.99999999675164,-4.7042841621304,11.9162633242021));
#50168=CARTESIAN_POINT('Ctrl Pts',(5.99999999861006,-4.73345997583683,11.983364769614));
#50169=CARTESIAN_POINT('Ctrl Pts',(5.99999999947164,-4.74698602854524,12.0144733342829));
#50170=CARTESIAN_POINT('Ctrl Pts',(5.99999999999964,-4.76066986105812,12.0455084646858));
#50171=CARTESIAN_POINT('Ctrl Pts',(5.99999999999964,-4.77450986189331,12.0764672982565));
#50172=CARTESIAN_POINT('Ctrl Pts',(5.99999999999964,-4.86135084173874,12.2707227375566));
#50173=CARTESIAN_POINT('Ctrl Pts',(5.99999998564321,-4.95440528223575,12.4619539561128));
#50174=CARTESIAN_POINT('Ctrl Pts',(5.99999998504707,-5.05350675322791,12.6499606228551));
#50175=CARTESIAN_POINT('Ctrl Pts',(5.99999998445021,-5.15272817727757,12.8381948540754));
#50176=CARTESIAN_POINT('Ctrl Pts',(5.99999999412994,-5.25801152344585,13.023197247302));
#50177=CARTESIAN_POINT('Ctrl Pts',(5.99999999838049,-5.36923749341353,13.2047460650019));
#50178=CARTESIAN_POINT('Ctrl Pts',(5.99999999937176,-5.39517633608685,13.2470847941782));
#50179=CARTESIAN_POINT('Ctrl Pts',(5.99999999999964,-5.42143857101673,13.2892355886078));
#50180=CARTESIAN_POINT('Ctrl Pts',(5.99999999999964,-5.44802303613172,13.3311954268116));
#50181=CARTESIAN_POINT('Ctrl Pts',(5.99999999999964,-5.45163185422273,13.3368914384691));
#50182=CARTESIAN_POINT('Ctrl Pts',(5.99999999998809,-5.45524657348537,13.3425839531359));
#50183=CARTESIAN_POINT('Ctrl Pts',(5.99999999996604,-5.4588671850516,13.34827295269));
#50184=CARTESIAN_POINT('Ctrl Pts',(5.99999999925237,-5.57604776336622,13.5323966140054));
#50185=CARTESIAN_POINT('Ctrl Pts',(5.99999999047919,-5.69940422499466,13.7128361170636));
#50186=CARTESIAN_POINT('Ctrl Pts',(5.99999999007259,-5.82856611522884,13.8890432899602));
#50187=CARTESIAN_POINT('Ctrl Pts',(5.99999998966574,-5.95780780329363,14.0653593258513));
#50188=CARTESIAN_POINT('Ctrl Pts',(5.99999999693161,-6.0928617689166,14.2374373446999));
#50189=CARTESIAN_POINT('Ctrl Pts',(5.99999999941399,-6.23331420401645,14.4047579275877));
#50190=CARTESIAN_POINT('Ctrl Pts',(5.9999999997784,-6.25393267611085,14.4293206542263));
#50191=CARTESIAN_POINT('Ctrl Pts',(5.99999999999964,-6.27466741733337,14.4537809157782));
#50192=CARTESIAN_POINT('Ctrl Pts',(5.99999999999964,-6.2955170479287,14.4781371321465));
#50193=CARTESIAN_POINT('Ctrl Pts',(5.99999999999964,-6.32570224107129,14.5133990084633));
#50194=CARTESIAN_POINT('Ctrl Pts',(5.99999999953037,-6.35612917108748,14.5484417054598));
#50195=CARTESIAN_POINT('Ctrl Pts',(5.99999999872727,-6.38679633278149,14.5832632927422));
#50196=CARTESIAN_POINT('Ctrl Pts',(5.99999999501559,-6.52853212226999,14.7441997763321));
#50197=CARTESIAN_POINT('Ctrl Pts',(5.99999998445152,-6.6753964956604,14.9004162347669));
#50198=CARTESIAN_POINT('Ctrl Pts',(5.999999984192,-6.82720752829195,15.0517246168236));
#50199=CARTESIAN_POINT('Ctrl Pts',(5.99999998393248,-6.9790185609235,15.2030329988804));
#50200=CARTESIAN_POINT('Ctrl Pts',(5.99999999999964,-7.13577669839019,15.3494336839672));
#50201=CARTESIAN_POINT('Ctrl Pts',(5.99999999999964,-7.29733250616056,15.4906976787841));
#50202=CARTESIAN_POINT('Ctrl Pts',(5.99999999999964,-7.36277743002716,15.5479225567596));
#50203=CARTESIAN_POINT('Ctrl Pts',(5.99999999597136,-7.42900259215504,15.6043159764659));
#50204=CARTESIAN_POINT('Ctrl Pts',(5.99999999157427,-7.4959686438229,15.6598380057875));
#50205=CARTESIAN_POINT('Ctrl Pts',(5.99999998233622,-7.63666088216823,15.7764869404068));
#50206=CARTESIAN_POINT('Ctrl Pts',(5.99999997355915,-7.78062539150357,15.8892868534789));
#50207=CARTESIAN_POINT('Ctrl Pts',(5.9999999766057,-7.92744931055709,15.9979550108572));
#50208=CARTESIAN_POINT('Ctrl Pts',(5.99999997965606,-8.07445659054523,16.1067588783776));
#50209=CARTESIAN_POINT('Ctrl Pts',(5.99999999487359,-8.22433003955843,16.2114204204104));
#50210=CARTESIAN_POINT('Ctrl Pts',(5.99999999914227,-8.3766267401238,16.3116995118965));
#50211=CARTESIAN_POINT('Ctrl Pts',(5.99999999968358,-8.39593950507439,16.3244159168884));
#50212=CARTESIAN_POINT('Ctrl Pts',(5.99999999999964,-8.41529120489321,16.3370619088378));
#50213=CARTESIAN_POINT('Ctrl Pts',(5.99999999999964,-8.43468090863971,16.3496370511817));
#50214=CARTESIAN_POINT('Ctrl Pts',(5.99999999999964,-8.54220010411144,16.4193683480303));
#50215=CARTESIAN_POINT('Ctrl Pts',(5.99999999306097,-8.65090020066499,16.4868824523981));
#50216=CARTESIAN_POINT('Ctrl Pts',(5.99999999145041,-8.76082946575123,16.5522391036968));
#50217=CARTESIAN_POINT('Ctrl Pts',(5.99999998952811,-8.89203617744543,16.6302459137806));
#50218=CARTESIAN_POINT('Ctrl Pts',(5.99999999274889,-9.02499344698057,16.7051805038707));
#50219=CARTESIAN_POINT('Ctrl Pts',(5.99999999547939,-9.15977660596245,16.77710082022));
#50220=CARTESIAN_POINT('Ctrl Pts',(5.99999999819764,-9.29395486698284,16.8486983629151));
#50221=CARTESIAN_POINT('Ctrl Pts',(5.99999999961508,-9.42994306423093,16.9173088546184));
#50222=CARTESIAN_POINT('Ctrl Pts',(5.99999999985075,-9.56784005909749,16.9829441671397));
#50223=CARTESIAN_POINT('Ctrl Pts',(5.99999999991363,-9.60463569607508,17.000457914519));
#50224=CARTESIAN_POINT('Ctrl Pts',(5.99999999993318,-9.6415673578591,17.0177595662489));
#50225=CARTESIAN_POINT('Ctrl Pts',(5.99999999993287,-9.67863716454406,17.0348487658757));
#50226=CARTESIAN_POINT('Ctrl Pts',(-5.843530343888,-3.68102569951235,9.52189994868111));
#50227=CARTESIAN_POINT('Ctrl Pts',(-3.895686895925,-3.12103648012649,10.4637294176103));
#50228=CARTESIAN_POINT('Ctrl Pts',(0.0001666015752724,-2.56022887445691,
11.4058027387879));
#50229=CARTESIAN_POINT('Ctrl Pts',(3.896020099076,-3.1210844467252,10.4636488408523));
#50230=CARTESIAN_POINT('Ctrl Pts',(5.844030148614,-3.68116939546044,9.52165827066205));
#50231=CARTESIAN_POINT('Ctrl Pts',(-5.843530343888,-3.79662279658476,10.3005519341134));
#50232=CARTESIAN_POINT('Ctrl Pts',(-3.895686895925,-3.28186758282363,11.18029373168));
#50233=CARTESIAN_POINT('Ctrl Pts',(0.0001666015752724,-2.76485680927171,
12.0606419220534));
#50234=CARTESIAN_POINT('Ctrl Pts',(3.896020099076,-3.28191180342724,11.1802184343602));
#50235=CARTESIAN_POINT('Ctrl Pts',(5.844030148614,-3.79675488524719,10.3003261880898));
#50236=CARTESIAN_POINT('Ctrl Pts',(-5.843530343888,-4.23585843751791,11.9385072545362));
#50237=CARTESIAN_POINT('Ctrl Pts',(-3.895686895925,-3.77925766167596,12.680422361665));
#50238=CARTESIAN_POINT('Ctrl Pts',(0.0001666015752724,-3.32387356034649,
13.4219941444237));
#50239=CARTESIAN_POINT('Ctrl Pts',(3.896020099076,-3.77929661126955,12.680358934072));
#50240=CARTESIAN_POINT('Ctrl Pts',(5.844030148614,-4.23597560350961,11.9383168755067));
#50241=CARTESIAN_POINT('Ctrl Pts',(-5.843530343888,-5.50359507107154,14.2139339843199));
#50242=CARTESIAN_POINT('Ctrl Pts',(-3.895686895925,-5.0227305589228,14.7660279845532));
#50243=CARTESIAN_POINT('Ctrl Pts',(0.0001666015752723,-4.54131537343371,
15.3185232177626));
#50244=CARTESIAN_POINT('Ctrl Pts',(3.896020099076,-5.02277173499103,14.7659807289254));
#50245=CARTESIAN_POINT('Ctrl Pts',(5.844030148614,-5.50371846323605,14.2137923143161));
#50246=CARTESIAN_POINT('Ctrl Pts',(-5.843530343888,-7.3885036558207,16.1560614685031));
#50247=CARTESIAN_POINT('Ctrl Pts',(-3.895686895925,-6.77499014877311,16.5818442606898));
#50248=CARTESIAN_POINT('Ctrl Pts',(0.0001666015752726,-6.16225463083715,
17.0065471100577));
#50249=CARTESIAN_POINT('Ctrl Pts',(3.896020099076,-6.77504255683397,16.5818079353));
#50250=CARTESIAN_POINT('Ctrl Pts',(5.844030148614,-7.38866108637799,16.1559522105549));
#50251=CARTESIAN_POINT('Ctrl Pts',(-5.843530343888,-8.93341404016312,17.0810032252174));
#50252=CARTESIAN_POINT('Ctrl Pts',(-3.895686895925,-8.18554344792886,17.4915898940687));
#50253=CARTESIAN_POINT('Ctrl Pts',(0.0001666015752719,-7.43613134758468,
17.9044809341154));
#50254=CARTESIAN_POINT('Ctrl Pts',(3.896020099076,-8.1856075461192,17.4915545789671));
#50255=CARTESIAN_POINT('Ctrl Pts',(5.844030148614,-8.93360594737697,17.0808978667065));
#50256=CARTESIAN_POINT('Ctrl Pts',(-5.843530343888,-9.7478162324362,17.4349042421601));
#50257=CARTESIAN_POINT('Ctrl Pts',(-3.895686895925,-8.92797948591053,17.8601610805119));
#50258=CARTESIAN_POINT('Ctrl Pts',(0.0001666015752719,-8.10806017489658,
18.2855080497002));
#50259=CARTESIAN_POINT('Ctrl Pts',(3.896020099076,-8.92804961467074,17.8601247000316));
#50260=CARTESIAN_POINT('Ctrl Pts',(5.844030148614,-9.74802660653542,17.4347951191954));
#50261=CARTESIAN_POINT('Ctrl Pts',(-5.73278975507593,-3.68906394503202,
9.81543852465543));
#50262=CARTESIAN_POINT('Ctrl Pts',(-5.37827938811351,-3.5926364172673,9.98669208751431));
#50263=CARTESIAN_POINT('Ctrl Pts',(-5.01472906935724,-3.5020771266496,10.1416940408098));
#50264=CARTESIAN_POINT('Ctrl Pts',(-4.64374065706591,-3.41910155232867,
10.2799308470485));
#50265=CARTESIAN_POINT('Ctrl Pts',(-4.36982475309857,-3.35783729529447,
10.3819967296689));
#50266=CARTESIAN_POINT('Ctrl Pts',(-4.09185399305988,-3.300710650761,10.4749208688385));
#50267=CARTESIAN_POINT('Ctrl Pts',(-3.8104731320656,-3.24841333385155,10.5585213690633));
#50268=CARTESIAN_POINT('Ctrl Pts',(-3.56966629229311,-3.20365708579314,
10.6300670036577));
#50269=CARTESIAN_POINT('Ctrl Pts',(-3.32636189347357,-3.16243849649299,
10.6947833712621));
#50270=CARTESIAN_POINT('Ctrl Pts',(-3.08096406234829,-3.12517322062064,
10.7525923015923));
#50271=CARTESIAN_POINT('Ctrl Pts',(-3.03961649590347,-3.11889432050505,
10.7623326427231));
#50272=CARTESIAN_POINT('Ctrl Pts',(-2.99820949786317,-3.11272759517701,
10.771876989757));
#50273=CARTESIAN_POINT('Ctrl Pts',(-2.95674500133169,-3.10667495605758,
10.7812251058998));
#50274=CARTESIAN_POINT('Ctrl Pts',(-2.75869126751695,-3.07776473460763,
10.8258760593922));
#50275=CARTESIAN_POINT('Ctrl Pts',(-2.55931851145658,-3.05147470370263,
10.866112310125));
#50276=CARTESIAN_POINT('Ctrl Pts',(-2.3588938886275,-3.02798173187965,10.9018069262272));
#50277=CARTESIAN_POINT('Ctrl Pts',(-2.16496946930528,-3.00525068788607,
10.9363438888161));
#50278=CARTESIAN_POINT('Ctrl Pts',(-1.97006030543694,-2.9851382609123,10.9666289729053));
#50279=CARTESIAN_POINT('Ctrl Pts',(-1.77440839311645,-2.96778003865636,
10.9925888897745));
#50280=CARTESIAN_POINT('Ctrl Pts',(-1.58213143387715,-2.95072124197205,
11.0181010037043));
#50281=CARTESIAN_POINT('Ctrl Pts',(-1.38913712967679,-2.93632253343784,
11.0394357553739));
#50282=CARTESIAN_POINT('Ctrl Pts',(-1.19565516824816,-2.92468739892694,
11.0565659989504));
#50283=CARTESIAN_POINT('Ctrl Pts',(-0.997079050885878,-2.91274592480137,
11.0741472619982));
#50284=CARTESIAN_POINT('Ctrl Pts',(-0.797989259347558,-2.90371574544053,
11.0872992420739));
#50285=CARTESIAN_POINT('Ctrl Pts',(-0.598634105458042,-2.89767892437813,
11.0960425446415));
#50286=CARTESIAN_POINT('Ctrl Pts',(-0.410109704659265,-2.89197007737159,
11.104310832897));
#50287=CARTESIAN_POINT('Ctrl Pts',(-0.221347991964562,-2.88893803264954,
11.1086367045487));
#50288=CARTESIAN_POINT('Ctrl Pts',(-0.0325589666053618,-2.88862552635304,
11.1090821638272));
#50289=CARTESIAN_POINT('Ctrl Pts',(-0.021713010796759,-2.88860757282277,
11.1091077555248));
#50290=CARTESIAN_POINT('Ctrl Pts',(-0.0108669648422019,-2.88859858781384,
11.1091205521597));
#50291=CARTESIAN_POINT('Ctrl Pts',(-2.08685607461212E-5,-2.88859857671928,
11.1091205700193));
#50292=CARTESIAN_POINT('Ctrl Pts',(-1.39123740674034E-5,-2.88859857671216,
11.1091205700308));
#50293=CARTESIAN_POINT('Ctrl Pts',(-6.95618740951635E-6,-2.88859857670874,
11.1091205700369));
#50294=CARTESIAN_POINT('Ctrl Pts',(-7.71824779259152E-13,-2.888598576709,
11.1091205700379));
#50295=CARTESIAN_POINT('Ctrl Pts',(0.189138135939297,-2.88859858396895,
11.1091205956408));
#50296=CARTESIAN_POINT('Ctrl Pts',(0.378261102849913,-2.8913297812093,11.1052308718856));
#50297=CARTESIAN_POINT('Ctrl Pts',(0.567157735032297,-2.89675072938151,
11.097386492419));
#50298=CARTESIAN_POINT('Ctrl Pts',(0.758596842520583,-2.90224464141074,
11.0894365306513));
#50299=CARTESIAN_POINT('Ctrl Pts',(0.9498034815225,-2.91050114709193,11.0774248224279));
#50300=CARTESIAN_POINT('Ctrl Pts',(1.14055784443443,-2.92144963097601,11.0613297422791));
#50301=CARTESIAN_POINT('Ctrl Pts',(1.33593682192776,-2.93266354794085,11.0448444558922));
#50302=CARTESIAN_POINT('Ctrl Pts',(1.53084132769911,-2.9467015227625,11.0240754452359));
#50303=CARTESIAN_POINT('Ctrl Pts',(1.72503517650004,-2.96345959006647,10.9990465232928));
#50304=CARTESIAN_POINT('Ctrl Pts',(1.93231732485309,-2.98134711953489,10.9723306991647));
#50305=CARTESIAN_POINT('Ctrl Pts',(2.13878979419026,-3.00233390089858,10.9407611301654));
#50306=CARTESIAN_POINT('Ctrl Pts',(2.3441653530124,-3.02626068936978,10.9044219674174));
#50307=CARTESIAN_POINT('Ctrl Pts',(2.54954091183454,-3.05018747784097,10.8680828046695));
#50308=CARTESIAN_POINT('Ctrl Pts',(2.75381956014164,-3.07705404236012,10.8269744144489));
#50309=CARTESIAN_POINT('Ctrl Pts',(2.95671406643458,-3.10667058743364,10.7812326584043));
#50310=CARTESIAN_POINT('Ctrl Pts',(3.20113148620673,-3.14234823914386,10.7261297273662));
#50311=CARTESIAN_POINT('Ctrl Pts',(3.4435512564494,-3.18199220866165,10.6642045337227));
#50312=CARTESIAN_POINT('Ctrl Pts',(3.6835774224282,-3.22519952773969,10.5955259435043));
#50313=CARTESIAN_POINT('Ctrl Pts',(3.97270114029476,-3.27724493987194,10.5127990905348));
#50314=CARTESIAN_POINT('Ctrl Pts',(4.25835187551307,-3.33445985228253,10.4202739795983));
#50315=CARTESIAN_POINT('Ctrl Pts',(4.53983760443492,-3.3961047918017,10.318138965713));
#50316=CARTESIAN_POINT('Ctrl Pts',(4.90288791141567,-3.47561224783496,10.1864088482163));
#50317=CARTESIAN_POINT('Ctrl Pts',(5.25900976155327,-3.56248371088252,10.0386967436174));
#50318=CARTESIAN_POINT('Ctrl Pts',(5.6067184086683,-3.6551237001607,9.87547719539454));
#50319=CARTESIAN_POINT('Ctrl Pts',(5.6488656544825,-3.6663529877632,9.85569265889333));
#50320=CARTESIAN_POINT('Ctrl Pts',(5.69088928597589,-3.67766709728277,9.83568028366369));
#50321=CARTESIAN_POINT('Ctrl Pts',(5.73278665883251,-3.68906325960823,9.81544090739529));
#50322=CARTESIAN_POINT('Ctrl Pts',(-5.8453425191731,-3.7231328100584,9.78106691208113));
#50323=CARTESIAN_POINT('Ctrl Pts',(-5.67506455328666,-3.67640115211964,
9.86772733904583));
#50324=CARTESIAN_POINT('Ctrl Pts',(-5.16554261231927,-3.54223933518448,
10.1122105914422));
#50325=CARTESIAN_POINT('Ctrl Pts',(-4.2479673722814,-3.3315423036423,10.4776605637613));
#50326=CARTESIAN_POINT('Ctrl Pts',(-3.01809829204943,-3.11148833491602,
10.8376786076768));
#50327=CARTESIAN_POINT('Ctrl Pts',(-1.5847636096142,-2.94366648313399,11.0983867442987));
#50328=CARTESIAN_POINT('Ctrl Pts',(-0.000577220786009364,-2.87785633358549,
11.197120468893));
#50329=CARTESIAN_POINT('Ctrl Pts',(1.58371386520435,-2.94357748223322,11.0985217867746));
#50330=CARTESIAN_POINT('Ctrl Pts',(3.01728962515512,-3.11136351464933,10.8378775916792));
#50331=CARTESIAN_POINT('Ctrl Pts',(4.24739718405343,-3.33142250739312,10.4778629558088));
#50332=CARTESIAN_POINT('Ctrl Pts',(5.16523409169761,-3.54216090499289,10.1123513050415));
#50333=CARTESIAN_POINT('Ctrl Pts',(5.67493343697088,-3.67636527157484,9.86779379746524));
#50334=CARTESIAN_POINT('Ctrl Pts',(5.84532822576121,-3.72312888450214,9.78107419617581));
#50335=CARTESIAN_POINT('Ctrl Pts',(-5.72604640297174,-3.64453078977728,
9.50066684202224));
#50336=CARTESIAN_POINT('Ctrl Pts',(-5.55920897504384,-3.59938887890874,
9.58541783912223));
#50337=CARTESIAN_POINT('Ctrl Pts',(-5.05998748611983,-3.46975016126909,
9.82453542560563));
#50338=CARTESIAN_POINT('Ctrl Pts',(-4.16100412910273,-3.26599618147832,
10.1820357658773));
#50339=CARTESIAN_POINT('Ctrl Pts',(-2.95616914600619,-3.05303432798076,
10.5342751778561));
#50340=CARTESIAN_POINT('Ctrl Pts',(-1.55217413832987,-2.89053739077631,
10.789367770727));
#50341=CARTESIAN_POINT('Ctrl Pts',(-0.000565337860044441,-2.82679815128164,
10.8859758425079));
#50342=CARTESIAN_POINT('Ctrl Pts',(1.55114593661906,-2.8904511972708,10.789499906014));
#50343=CARTESIAN_POINT('Ctrl Pts',(2.95537697819746,-3.05291349664009,10.534469871294));
#50344=CARTESIAN_POINT('Ctrl Pts',(4.16044551304384,-3.26588029055499,10.1822337713712));
#50345=CARTESIAN_POINT('Ctrl Pts',(5.05968520530428,-3.46967435460816,9.82467306139067));
#50346=CARTESIAN_POINT('Ctrl Pts',(5.55908050810257,-3.59935421833968,9.58548283353558));
#50347=CARTESIAN_POINT('Ctrl Pts',(5.7260323983644,-3.6445269978645,9.50067396559784));
#50348=CARTESIAN_POINT('Ctrl Pts',(-5.72051779202094,-3.37344235740397,
9.34118936873082));
#50349=CARTESIAN_POINT('Ctrl Pts',(-5.55415467081518,-3.32879645284527,
9.42508071207038));
#50350=CARTESIAN_POINT('Ctrl Pts',(-5.05630407037826,-3.20054253028145,
9.66183113507364));
#50351=CARTESIAN_POINT('Ctrl Pts',(-4.15940711858513,-2.99876113157881,
10.0160784557331));
#50352=CARTESIAN_POINT('Ctrl Pts',(-2.95633243052256,-2.78754959294785,
10.3655357023154));
#50353=CARTESIAN_POINT('Ctrl Pts',(-1.5529049313792,-2.62613144283214,10.6189509912225));
#50354=CARTESIAN_POINT('Ctrl Pts',(-0.000565719984574329,-2.56273619156729,
10.7150256790838));
#50355=CARTESIAN_POINT('Ctrl Pts',(1.55187664827042,-2.62604575142131,10.6190823491583));
#50356=CARTESIAN_POINT('Ctrl Pts',(2.95554107092965,-2.78742966586911,10.3657289784477));
#50357=CARTESIAN_POINT('Ctrl Pts',(4.15884962684187,-2.99864629259101,10.0162747578376));
#50358=CARTESIAN_POINT('Ctrl Pts',(5.05600259450201,-3.20046751258044,9.66196743919455));
#50359=CARTESIAN_POINT('Ctrl Pts',(5.55402656806235,-3.32876217187809,9.4251450482282));
#50360=CARTESIAN_POINT('Ctrl Pts',(5.72050382722823,-3.37343860686065,9.34119641994125));
#50361=CARTESIAN_POINT('Ctrl Pts',(-5.8321369521679,-3.08677373258812,9.40625311678606));
#50362=CARTESIAN_POINT('Ctrl Pts',(-5.6629787715248,-3.04120920698067,9.49089236294299));
#50363=CARTESIAN_POINT('Ctrl Pts',(-5.15669403421204,-2.91030605895675,
9.72980983428538));
#50364=CARTESIAN_POINT('Ctrl Pts',(-4.24405124974489,-2.70425182829767,
10.0876100470662));
#50365=CARTESIAN_POINT('Ctrl Pts',(-3.01836174675186,-2.48831932058566,
10.4410836918675));
#50366=CARTESIAN_POINT('Ctrl Pts',(-1.58641566211653,-2.32303952972319,
10.6978445692024));
#50367=CARTESIAN_POINT('Ctrl Pts',(-0.000578094601629952,-2.25804067749337,
10.7953224050997));
#50368=CARTESIAN_POINT('Ctrl Pts',(1.58536576833291,-2.32295171259286,10.6979777817111));
#50369=CARTESIAN_POINT('Ctrl Pts',(3.0175550085335,-2.48819663021148,10.4412793413565));
#50370=CARTESIAN_POINT('Ctrl Pts',(4.24348372250814,-2.70413450834432,10.0878084330091));
#50371=CARTESIAN_POINT('Ctrl Pts',(5.15638741473864,-2.91022948542556,9.72994741671057));
#50372=CARTESIAN_POINT('Ctrl Pts',(5.66284851503276,-3.04117421967098,9.49095727370096));
#50373=CARTESIAN_POINT('Ctrl Pts',(5.83212275275338,-3.08676990438137,9.40626023074137));
#50374=CARTESIAN_POINT('Ctrl Pts',(-5.72001848982158,-3.07996758646315,
9.45352556453397));
#50375=CARTESIAN_POINT('Ctrl Pts',(-5.58622578267763,-3.04453966207226,
9.51893357204611));
#50376=CARTESIAN_POINT('Ctrl Pts',(-5.44977387166592,-3.00953603645086,
9.5826456141395));
#50377=CARTESIAN_POINT('Ctrl Pts',(-5.31065166372667,-2.97511769228166,
9.64449101662499));
#50378=CARTESIAN_POINT('Ctrl Pts',(-5.13208489793212,-2.93094090344732,
9.72387110744355));
#50379=CARTESIAN_POINT('Ctrl Pts',(-4.94911791823773,-2.88772691608189,
9.80017676710201));
#50380=CARTESIAN_POINT('Ctrl Pts',(-4.76175997779212,-2.8458635140101,9.87302804119503));
#50381=CARTESIAN_POINT('Ctrl Pts',(-4.7051486885805,-2.83321424408094,9.89504047652233));
#50382=CARTESIAN_POINT('Ctrl Pts',(-4.64813670743062,-2.82068854073505,
9.91673738375662));
#50383=CARTESIAN_POINT('Ctrl Pts',(-4.59072480806432,-2.80829778838811,
9.9381078908515));
#50384=CARTESIAN_POINT('Ctrl Pts',(-4.4857722613471,-2.78564671728773,9.97717451587178));
#50385=CARTESIAN_POINT('Ctrl Pts',(-4.37948383410515,-2.76344222716346,
10.0151514952229));
#50386=CARTESIAN_POINT('Ctrl Pts',(-4.27186582327879,-2.74174263669791,
10.0519746286223));
#50387=CARTESIAN_POINT('Ctrl Pts',(-4.17673451642801,-2.7225608066003,10.0845252470152));
#50388=CARTESIAN_POINT('Ctrl Pts',(-4.08056426553211,-2.70377355566689,
10.1161742105508));
#50389=CARTESIAN_POINT('Ctrl Pts',(-3.98336429796612,-2.68542343476573,
10.1468761006882));
#50390=CARTESIAN_POINT('Ctrl Pts',(-3.87978521472512,-2.6658690177438,10.1795929185415));
#50391=CARTESIAN_POINT('Ctrl Pts',(-3.7750360592736,-2.6468099807019,10.2112347704345));
#50392=CARTESIAN_POINT('Ctrl Pts',(-3.66912935139674,-2.62829352068104,
10.2417467237293));
#50393=CARTESIAN_POINT('Ctrl Pts',(-3.6161759974583,-2.61903529067062,10.2570027003767));
#50394=CARTESIAN_POINT('Ctrl Pts',(-3.56293325208084,-2.60991270167467,
10.2719761901948));
#50395=CARTESIAN_POINT('Ctrl Pts',(-3.509403031323,-2.60093137580247,10.2866602299529));
#50396=CARTESIAN_POINT('Ctrl Pts',(-3.48263792094408,-2.59644071286637,
10.294002249832));
#50397=CARTESIAN_POINT('Ctrl Pts',(-3.45580094155328,-2.59198536552492,
10.3012719064436));
#50398=CARTESIAN_POINT('Ctrl Pts',(-3.42889234295528,-2.58756602568168,
10.3084683245832));
#50399=CARTESIAN_POINT('Ctrl Pts',(-3.41543804365629,-2.58535635576006,
10.312066533653));
#50400=CARTESIAN_POINT('Ctrl Pts',(-3.40196583954607,-2.58315568770107,
10.3156464330547));
#50401=CARTESIAN_POINT('Ctrl Pts',(-3.38847576308459,-2.58096410694689,
10.3192079130426));
#50402=CARTESIAN_POINT('Ctrl Pts',(-3.38173072485385,-2.5798683165698,10.3209886530365));
#50403=CARTESIAN_POINT('Ctrl Pts',(-3.37498121853475,-2.57877479801818,
10.3227647881738));
#50404=CARTESIAN_POINT('Ctrl Pts',(-3.36822724826745,-2.5776835619006,10.3245363047155));
#50405=CARTESIAN_POINT('Ctrl Pts',(-3.36147327800015,-2.57659232578302,
10.3263078212572));
#50406=CARTESIAN_POINT('Ctrl Pts',(-3.35627145380202,-2.57575348794432,
10.3276690999076));
#50407=CARTESIAN_POINT('Ctrl Pts',(-3.3479519497851,-2.57441671143473,10.3298369848019));
#50408=CARTESIAN_POINT('Ctrl Pts',(-3.25356415140478,-2.5592504958275,10.3544324272589));
#50409=CARTESIAN_POINT('Ctrl Pts',(-3.15870247896028,-2.54463161966691,
10.3780134172734));
#50410=CARTESIAN_POINT('Ctrl Pts',(-3.06338153310827,-2.53058637637817,
10.4005674015095));
#50411=CARTESIAN_POINT('Ctrl Pts',(-2.82247525276361,-2.49508958931858,
10.4575684771985));
#50412=CARTESIAN_POINT('Ctrl Pts',(-2.57863516797202,-2.46325459397254,
10.5080123788613));
#50413=CARTESIAN_POINT('Ctrl Pts',(-2.33218278235404,-2.43545349318644,
10.5516955911938));
#50414=CARTESIAN_POINT('Ctrl Pts',(-2.10395730382933,-2.40970848157087,
10.5921481192271));
#50415=CARTESIAN_POINT('Ctrl Pts',(-1.87349141229418,-2.38742283707054,
10.6268027113683));
#50416=CARTESIAN_POINT('Ctrl Pts',(-1.64104497974962,-2.36891812822664,
10.6554678629544));
#50417=CARTESIAN_POINT('Ctrl Pts',(-1.3922221275377,-2.3491097173877,10.6861525445761));
#50418=CARTESIAN_POINT('Ctrl Pts',(-1.14112895901219,-2.33363391051612,
10.7099744151135));
#50419=CARTESIAN_POINT('Ctrl Pts',(-0.888194890405294,-2.32271175966412,
10.7267278495743));
#50420=CARTESIAN_POINT('Ctrl Pts',(-0.642857048742712,-2.31211762763951,
10.7429781375394));
#50421=CARTESIAN_POINT('Ctrl Pts',(-0.39578685941527,-2.30580769801516,
10.7525781133018));
#50422=CARTESIAN_POINT('Ctrl Pts',(-0.147396649499607,-2.30401191327079,
10.7553051728695));
#50423=CARTESIAN_POINT('Ctrl Pts',(-0.098524625314327,-2.30365858358244,
10.7558417355673));
#50424=CARTESIAN_POINT('Ctrl Pts',(-0.0496015747295809,-2.3034800992254,
10.756112120393));
#50425=CARTESIAN_POINT('Ctrl Pts',(-0.000630754449614001,-2.30347834825338,
10.7561144689972));
#50426=CARTESIAN_POINT('Ctrl Pts',(-0.000533215627239487,-2.30347834476584,
10.7561144736751));
#50427=CARTESIAN_POINT('Ctrl Pts',(-0.000435676615370138,-2.30347834197944,
10.7561144772896));
#50428=CARTESIAN_POINT('Ctrl Pts',(-0.000338137414028911,-2.30347833989419,
10.7561144798408));
#50429=CARTESIAN_POINT('Ctrl Pts',(0.244409904318021,-2.30347310752446,
10.7561208812728));
#50430=CARTESIAN_POINT('Ctrl Pts',(0.487933354864567,-2.30778625269226,
10.7494552516389));
#50431=CARTESIAN_POINT('Ctrl Pts',(0.729872147671101,-2.31627266092412,
10.7363207591529));
#50432=CARTESIAN_POINT('Ctrl Pts',(0.979162356039925,-2.32501693236518,
10.7227871693939));
#50433=CARTESIAN_POINT('Ctrl Pts',(1.22677062301498,-2.33819212181328,10.7023856402231));
#50434=CARTESIAN_POINT('Ctrl Pts',(1.47230782490225,-2.35567297733128,10.6752950678761));
#50435=CARTESIAN_POINT('Ctrl Pts',(1.528321383462,-2.35966082486195,10.6691149886501));
#50436=CARTESIAN_POINT('Ctrl Pts',(1.58422716278209,-2.36387287435707,10.6625866267576));
#50437=CARTESIAN_POINT('Ctrl Pts',(1.64002053878389,-2.36830785902908,10.6557118041948));
#50438=CARTESIAN_POINT('Ctrl Pts',(1.66262960639652,-2.37010504133809,10.6529259299695));
#50439=CARTESIAN_POINT('Ctrl Pts',(1.6852202161838,-2.3719388327086,10.6500831621575));
#50440=CARTESIAN_POINT('Ctrl Pts',(1.70779213306391,-2.37380899889092,10.6471836667687));
#50441=CARTESIAN_POINT('Ctrl Pts',(1.96542943282148,-2.39515519504559,10.6140886413609));
#50442=CARTESIAN_POINT('Ctrl Pts',(2.2206321287962,-2.42118695686794,10.5736172429053));
#50443=CARTESIAN_POINT('Ctrl Pts',(2.4730072388591,-2.45145930067294,10.5260280642484));
#50444=CARTESIAN_POINT('Ctrl Pts',(2.49462591754807,-2.45405245684322,10.5219515324454));
#50445=CARTESIAN_POINT('Ctrl Pts',(2.51622385526068,-2.45667675055344,10.51782274966));
#50446=CARTESIAN_POINT('Ctrl Pts',(2.53780080883655,-2.45933191372699,10.5136418660488));
#50447=CARTESIAN_POINT('Ctrl Pts',(2.67453329246864,-2.47615760016557,10.4871477366566));
#50448=CARTESIAN_POINT('Ctrl Pts',(2.81042370077703,-2.4942183611075,10.4585625221685));
#50449=CARTESIAN_POINT('Ctrl Pts',(2.94541467454037,-2.51342296590514,10.4279279256618));
#50450=CARTESIAN_POINT('Ctrl Pts',(2.98455461983106,-2.51899124325105,10.4190455804365));
#50451=CARTESIAN_POINT('Ctrl Pts',(3.02361901368985,-2.52465562262786,10.4099909370238));
#50452=CARTESIAN_POINT('Ctrl Pts',(3.062606395271,-2.53041373041998,10.4007650315162));
#50453=CARTESIAN_POINT('Ctrl Pts',(3.0908514097118,-2.53458528108956,10.3940811809029));
#50454=CARTESIAN_POINT('Ctrl Pts',(3.11905600485032,-2.53880602549,10.3873074429548));
#50455=CARTESIAN_POINT('Ctrl Pts',(3.14721977094275,-2.54307494828719,10.3804442461762));
#50456=CARTESIAN_POINT('Ctrl Pts',(3.18073927009834,-2.54815566631426,10.3722759167749));
#50457=CARTESIAN_POINT('Ctrl Pts',(3.21420086917299,-2.55330468622933,10.3639808691688));
#50458=CARTESIAN_POINT('Ctrl Pts',(3.24760374504299,-2.55852039067303,10.3555598279387));
#50459=CARTESIAN_POINT('Ctrl Pts',(3.26430518297799,-2.56112824289488,10.3513493073237));
#50460=CARTESIAN_POINT('Ctrl Pts',(3.28099194011519,-2.56375276624447,10.3471072882752));
#50461=CARTESIAN_POINT('Ctrl Pts',(3.29766391504872,-2.56639375418664,10.3428338619783));
#50462=CARTESIAN_POINT('Ctrl Pts',(3.30599990251548,-2.56771424815772,10.3406971488299));
#50463=CARTESIAN_POINT('Ctrl Pts',(3.31433219443153,-2.56903885827675,10.3385525838679));
#50464=CARTESIAN_POINT('Ctrl Pts',(3.32266077821784,-2.57036755844855,10.3364001785307));
#50465=CARTESIAN_POINT('Ctrl Pts',(3.33098936200414,-2.57169625862036,10.3342477731935));
#50466=CARTESIAN_POINT('Ctrl Pts',(3.34087181527658,-2.57327928504732,10.3316817010557));
#50467=CARTESIAN_POINT('Ctrl Pts',(3.34763539263782,-2.57436590294479,10.3299194528409));
#50468=CARTESIAN_POINT('Ctrl Pts',(3.55089958588706,-2.60702177401758,10.2769590233857));
#50469=CARTESIAN_POINT('Ctrl Pts',(3.75013357593846,-2.64183173682445,10.2197943054953));
#50470=CARTESIAN_POINT('Ctrl Pts',(3.94524370460647,-2.67839851809335,10.158815086571));
#50471=CARTESIAN_POINT('Ctrl Pts',(4.0552261841343,-2.69901100653647,10.1244414446553));
#50472=CARTESIAN_POINT('Ctrl Pts',(4.16389879090913,-2.72018245532118,10.0888553228505));
#50473=CARTESIAN_POINT('Ctrl Pts',(4.27124838423353,-2.74184714293357,10.0521233937558));
#50474=CARTESIAN_POINT('Ctrl Pts',(4.46895191147968,-2.78174655032778,9.98447495914437));
#50475=CARTESIAN_POINT('Ctrl Pts',(4.66216685332365,-2.82331649695166,9.91294166868344));
#50476=CARTESIAN_POINT('Ctrl Pts',(4.85086295645824,-2.86617782292787,9.83792425129904));
#50477=CARTESIAN_POINT('Ctrl Pts',(5.00709279590326,-2.90166460810482,9.77581401754829));
#50478=CARTESIAN_POINT('Ctrl Pts',(5.16022547334113,-2.93803744985436,9.7113149597602));
#50479=CARTESIAN_POINT('Ctrl Pts',(5.3102552388505,-2.97510203019643,9.64464181156364));
#50480=CARTESIAN_POINT('Ctrl Pts',(5.44951286408245,-3.00950537290067,9.58275579679139));
#50481=CARTESIAN_POINT('Ctrl Pts',(5.58609733333168,-3.04450498702027,9.5189965480568));
#50482=CARTESIAN_POINT('Ctrl Pts',(5.72001565386956,-3.07996615527252,9.45352717993155));
#50483=CARTESIAN_POINT('Ctrl Pts',(6.00000005199879,6.44013554119082,7.42971628364908));
#50484=CARTESIAN_POINT('Ctrl Pts',(6.00000005199403,9.01014101712317,5.2020156589276));
#50485=CARTESIAN_POINT('Ctrl Pts',(6.00000005199597,9.65438823628283,1.86247620859738));
#50486=CARTESIAN_POINT('Ctrl Pts',(-1.77480316135306E-8,8.02987800172561,
9.26373598251951));
#50487=CARTESIAN_POINT('Ctrl Pts',(-1.77539708778783E-8,11.2342873349703,
6.48612918736558));
#50488=CARTESIAN_POINT('Ctrl Pts',(-1.77515442403932E-8,12.0375664802193,
2.32222701533043));
#50489=CARTESIAN_POINT('Ctrl Pts',(-6.00000008250361,6.44013553309638,7.42971627433652));
#50490=CARTESIAN_POINT('Ctrl Pts',(-6.00000008250837,9.01014100581212,5.20201565240322));
#50491=CARTESIAN_POINT('Ctrl Pts',(-6.00000008250642,9.65438822416544,1.86247620625276));
#50492=CARTESIAN_POINT('',(5.7200157459055,6.64701177631153,7.39409270204038));
#50493=CARTESIAN_POINT('',(5.99999953411714,6.4401355833762,7.4297163323166));
#50494=CARTESIAN_POINT('Ctrl Pts',(5.72001583931743,6.64701193944996,7.39409288350795));
#50495=CARTESIAN_POINT('Ctrl Pts',(5.77253148998233,6.61781801791691,7.39330532480335));
#50496=CARTESIAN_POINT('Ctrl Pts',(5.82202450461072,6.5858191061159,7.39608179412492));
#50497=CARTESIAN_POINT('Ctrl Pts',(5.86865900539029,6.55130191359264,7.40207789646962));
#50498=CARTESIAN_POINT('Ctrl Pts',(5.91529350616986,6.51678472106939,7.40807399881431));
#50499=CARTESIAN_POINT('Ctrl Pts',(5.95906967163339,6.47974956148326,7.41729007990723));
#50500=CARTESIAN_POINT('Ctrl Pts',(5.99999937684364,6.44013572009114,7.42971649001226));
#50501=CARTESIAN_POINT('Origin',(6.,0.,0.));
#50502=CARTESIAN_POINT('Origin',(-6.,0.,0.));
#50503=CARTESIAN_POINT('Ctrl Pts',(-5.72001846589485,6.6470094591946,7.39409290851757));
#50504=CARTESIAN_POINT('Ctrl Pts',(-5.5231394901781,6.75643001701867,7.39707039774803));
#50505=CARTESIAN_POINT('Ctrl Pts',(-5.32171545225581,6.86151613067316,7.39900784396097));
#50506=CARTESIAN_POINT('Ctrl Pts',(-5.11578943779626,6.96176314152386,7.40010341334367));
#50507=CARTESIAN_POINT('Ctrl Pts',(-4.91516479974086,7.05942938500864,7.40117077829727));
#50508=CARTESIAN_POINT('Ctrl Pts',(-4.71026659833169,7.1525025851152,7.40143882576999));
#50509=CARTESIAN_POINT('Ctrl Pts',(-4.50119423812476,7.24046082476656,7.40113344297331));
#50510=CARTESIAN_POINT('Ctrl Pts',(-4.46405236415797,7.25608667721419,7.40107919147237));
#50511=CARTESIAN_POINT('Ctrl Pts',(-4.42677882349615,7.27155100068417,7.40100689257849));
#50512=CARTESIAN_POINT('Ctrl Pts',(-4.38937426489685,7.28685073592356,7.40091787860229));
#50513=CARTESIAN_POINT('Ctrl Pts',(-4.17290200939842,7.3753952427918,7.40040272598668));
#50514=CARTESIAN_POINT('Ctrl Pts',(-3.95203428931582,7.45845302868536,7.39930682641914));
#50515=CARTESIAN_POINT('Ctrl Pts',(-3.7269248624741,7.5355061201909,7.39778910172017));
#50516=CARTESIAN_POINT('Ctrl Pts',(-3.71074103037603,7.54104571181556,7.3976799876682));
#50517=CARTESIAN_POINT('Ctrl Pts',(-3.69453527868055,7.54655424740712,7.39756870270795));
#50518=CARTESIAN_POINT('Ctrl Pts',(-3.67830766648862,7.55203152508966,7.39745531031399));
#50519=CARTESIAN_POINT('Ctrl Pts',(-3.60089666987613,7.57815992396402,7.39691439165503));
#50520=CARTESIAN_POINT('Ctrl Pts',(-3.52298895693033,7.60357773171555,7.39632456351004));
#50521=CARTESIAN_POINT('Ctrl Pts',(-3.44459143400836,7.62826428789934,7.39569108136119));
#50522=CARTESIAN_POINT('Ctrl Pts',(-3.40047427644871,7.64215631724125,7.39533459775393));
#50523=CARTESIAN_POINT('Ctrl Pts',(-3.35620200852254,7.6558167669054,7.39496429626105));
#50524=CARTESIAN_POINT('Ctrl Pts',(-3.31177650809438,7.66924224160979,7.39458087586784));
#50525=CARTESIAN_POINT('Ctrl Pts',(-3.25009102911909,7.68788371620499,7.39404849085527));
#50526=CARTESIAN_POINT('Ctrl Pts',(-3.18810964288943,7.70607203893023,7.39349109916318));
#50527=CARTESIAN_POINT('Ctrl Pts',(-3.12583671604774,7.72379802072698,7.39291073386073));
#50528=CARTESIAN_POINT('Ctrl Pts',(-3.09470025262689,7.73266101162535,7.3926205512095));
#50529=CARTESIAN_POINT('Ctrl Pts',(-3.06349090352057,7.74140841611209,7.39232462394246));
#50530=CARTESIAN_POINT('Ctrl Pts',(-3.03220922812262,7.75003908895116,7.39202318308018));
#50531=CARTESIAN_POINT('Ctrl Pts',(-3.00884507995295,7.75648530119685,7.39179803820284));
#50532=CARTESIAN_POINT('Ctrl Pts',(-2.98452267292826,7.76311520667045,7.39156074387149));
#50533=CARTESIAN_POINT('Ctrl Pts',(-2.96129868966198,7.76936973295334,7.39133170399724));
#50534=CARTESIAN_POINT('Ctrl Pts',(-2.95342866082446,7.77148923595362,7.39125408809498));
#50535=CARTESIAN_POINT('Ctrl Pts',(-2.94568489488984,7.77356606825519,7.39117742788552));
#50536=CARTESIAN_POINT('Ctrl Pts',(-2.9381477896787,7.77557976789438,7.39110253765057));
#50537=CARTESIAN_POINT('Ctrl Pts',(-2.68063742192718,7.84437919686656,7.38854386142102));
#50538=CARTESIAN_POINT('Ctrl Pts',(-2.42065148233588,7.90438548668657,7.38592323930718));
#50539=CARTESIAN_POINT('Ctrl Pts',(-2.15860855950913,7.95529807856872,7.38352069964086));
#50540=CARTESIAN_POINT('Ctrl Pts',(-2.01267631483025,7.98365140609092,7.38218272034092));
#50541=CARTESIAN_POINT('Ctrl Pts',(-1.86610582915604,8.00918356196372,7.38091238473016));
#50542=CARTESIAN_POINT('Ctrl Pts',(-1.71896772590052,8.03183579119116,7.37975842699033));
#50543=CARTESIAN_POINT('Ctrl Pts',(-1.45705453073431,8.07215789405457,7.3777043244021));
#50544=CARTESIAN_POINT('Ctrl Pts',(-1.19334276940858,8.10335765529222,7.37601877690129));
#50545=CARTESIAN_POINT('Ctrl Pts',(-0.928342879505017,8.1252642313035,7.37479855228938));
#50546=CARTESIAN_POINT('Ctrl Pts',(-0.668537591582842,8.14674138848295,
7.3736022468617));
#50547=CARTESIAN_POINT('Ctrl Pts',(-0.407493628490775,8.15928616787887,
7.37285308614969));
#50548=CARTESIAN_POINT('Ctrl Pts',(-0.145694535144678,8.16268769725533,
7.372646938407));
#50549=CARTESIAN_POINT('Ctrl Pts',(-0.0970991151635496,8.16331909267582,
7.37260867304861));
#50550=CARTESIAN_POINT('Ctrl Pts',(-0.0484776976229812,8.16363531386543,
7.37258913331296));
#50551=CARTESIAN_POINT('Ctrl Pts',(0.000166591020086083,8.16363481584133,
7.37258895560197));
#50552=CARTESIAN_POINT('Ctrl Pts',(0.00190546548824369,8.1636347980386,
7.37258894924938));
#50553=CARTESIAN_POINT('Ctrl Pts',(0.00364430926348846,8.16363437718273,
7.37258896579267));
#50554=CARTESIAN_POINT('Ctrl Pts',(0.00538312221381099,8.16363355325788,
7.3725890052864));
#50555=CARTESIAN_POINT('Ctrl Pts',(0.259912769618426,8.16351294609251,7.37259478642919));
#50556=CARTESIAN_POINT('Ctrl Pts',(0.513782238937853,8.15476007749901,7.37309182573407));
#50557=CARTESIAN_POINT('Ctrl Pts',(0.766576370396224,8.13753903915246,7.37403648893198));
#50558=CARTESIAN_POINT('Ctrl Pts',(1.00754521736796,8.12112357202875,7.37493696237361));
#50559=CARTESIAN_POINT('Ctrl Pts',(1.24753735727697,8.09701304609678,7.37624432959361));
#50560=CARTESIAN_POINT('Ctrl Pts',(1.48618589673797,8.06530630036304,7.37792465400272));
#50561=CARTESIAN_POINT('Ctrl Pts',(1.56754515871502,8.0544969426422,7.37849750458088));
#50562=CARTESIAN_POINT('Ctrl Pts',(1.6487503410598,8.04280946435164,7.3791078552369));
#50563=CARTESIAN_POINT('Ctrl Pts',(1.72978561822472,8.03024812918833,7.37975303236793));
#50564=CARTESIAN_POINT('Ctrl Pts',(1.89313269532141,8.00492758417209,7.3810535498987));
#50565=CARTESIAN_POINT('Ctrl Pts',(2.05578951477151,7.97605676126106,7.3824955366271));
#50566=CARTESIAN_POINT('Ctrl Pts',(2.21765372151952,7.94371404951127,7.38401368809007));
#50567=CARTESIAN_POINT('Ctrl Pts',(2.33873564296813,7.9195202035573,7.38514933567936));
#50568=CARTESIAN_POINT('Ctrl Pts',(2.45937279180157,7.89338226720244,7.38632911534868));
#50569=CARTESIAN_POINT('Ctrl Pts',(2.57952171143478,7.86533439980899,7.38752196222305));
#50570=CARTESIAN_POINT('Ctrl Pts',(2.63959617125139,7.85131046611226,7.38811838566023));
#50571=CARTESIAN_POINT('Ctrl Pts',(2.69954857141069,7.83680903390877,7.38871806148018));
#50572=CARTESIAN_POINT('Ctrl Pts',(2.7593736446158,7.82183476231597,7.38931646224121));
#50573=CARTESIAN_POINT('Ctrl Pts',(2.78928618121835,7.81434762651956,7.38961566262172));
#50574=CARTESIAN_POINT('Ctrl Pts',(2.81916688587343,7.80674227990913,7.38991454333619));
#50575=CARTESIAN_POINT('Ctrl Pts',(2.84901510459825,7.79901931313223,7.39021251677589));
#50576=CARTESIAN_POINT('Ctrl Pts',(2.87148424617008,7.79320561833642,7.39043682521665));
#50577=CARTESIAN_POINT('Ctrl Pts',(2.89300660022682,7.7875698938843,7.39065136963934));
#50578=CARTESIAN_POINT('Ctrl Pts',(2.91567876299272,7.78156096265451,7.39087679799907));
#50579=CARTESIAN_POINT('Ctrl Pts',(2.92312451421291,7.77958757319457,7.39095083078994));
#50580=CARTESIAN_POINT('Ctrl Pts',(2.93069416777718,7.77757354050241,7.39102603214866));
#50581=CARTESIAN_POINT('Ctrl Pts',(2.93846165110485,7.77549814727366,7.39110311474753));
#50582=CARTESIAN_POINT('Ctrl Pts',(3.1129971918326,7.72886401056257,7.39283516263321));
#50583=CARTESIAN_POINT('Ctrl Pts',(3.2853220231655,7.67854873869928,7.39445121691232));
#50584=CARTESIAN_POINT('Ctrl Pts',(3.45533244333518,7.62478460087811,7.39587259330837));
#50585=CARTESIAN_POINT('Ctrl Pts',(3.67851266022001,7.5542060332375,7.39773849712785));
#50586=CARTESIAN_POINT('Ctrl Pts',(3.89770434676101,7.47768574414708,7.39926806331439));
#50587=CARTESIAN_POINT('Ctrl Pts',(4.11277404326721,7.39575790599373,7.4002663862923));
#50588=CARTESIAN_POINT('Ctrl Pts',(4.33342340127712,7.31170457265415,7.40129060926625));
#50589=CARTESIAN_POINT('Ctrl Pts',(4.54973416432406,7.22195941871552,7.40175575729507));
#50590=CARTESIAN_POINT('Ctrl Pts',(4.76157917497623,7.12705170436546,7.4014738087237));
#50591=CARTESIAN_POINT('Ctrl Pts',(4.88434076837461,7.07205384435666,7.40131042297403));
#50592=CARTESIAN_POINT('Ctrl Pts',(5.00560304486508,7.01532149034196,7.4008965645055));
#50593=CARTESIAN_POINT('Ctrl Pts',(5.12534365331553,6.95695073152344,7.4001987774091));
#50594=CARTESIAN_POINT('Ctrl Pts',(5.32794536978775,6.85818711171679,7.39901811810486));
#50595=CARTESIAN_POINT('Ctrl Pts',(5.52619035504277,6.75473480708681,7.3970239419566));
#50596=CARTESIAN_POINT('Ctrl Pts',(5.72001565335726,6.64701161468287,7.39409252225231));
#50597=CARTESIAN_POINT('Ctrl Pts',(6.00000005305837,9.65438841513202,-1.86247527920914));
#50598=CARTESIAN_POINT('Ctrl Pts',(6.00000005303346,9.01014286082918,-5.20200782794672));
#50599=CARTESIAN_POINT('Ctrl Pts',(6.00000005304398,6.44014582844665,-7.42970736600423));
#50600=CARTESIAN_POINT('Ctrl Pts',(-1.7587155508212E-8,12.0375667041905,
-2.32222585665684));
#50601=CARTESIAN_POINT('Ctrl Pts',(-1.7618217734301E-8,11.2342896346967,
-6.48611942381034));
#50602=CARTESIAN_POINT('Ctrl Pts',(-1.76051041844286E-8,8.02989082900566,
-9.26372486430082));
#50603=CARTESIAN_POINT('Ctrl Pts',(-6.00000008328868,9.65438840314804,-1.86247527680773));
#50604=CARTESIAN_POINT('Ctrl Pts',(-6.0000000833136,9.01014284963475,-5.20200782145258));
#50605=CARTESIAN_POINT('Ctrl Pts',(-6.00000008330308,6.44014582040185,-7.42970735677997));
#50606=CARTESIAN_POINT('Origin',(6.,0.,0.));
#50607=CARTESIAN_POINT('Origin',(-6.,0.,0.));
#50608=CARTESIAN_POINT('Ctrl Pts',(6.00000005573429,3.21424330149493,-9.2921832640953));
#50609=CARTESIAN_POINT('Ctrl Pts',(6.00000005573452,4.88217919558463E-7,
-10.4040165263461));
#50610=CARTESIAN_POINT('Ctrl Pts',(6.00000005573716,-3.2142424294058,-9.29218356575536));
#50611=CARTESIAN_POINT('Ctrl Pts',(-1.69778360931036E-8,4.00767676717802,
-11.5859514948856));
#50612=CARTESIAN_POINT('Ctrl Pts',(-1.69775501936307E-8,6.08730473134062E-7,
-12.9722399354743));
#50613=CARTESIAN_POINT('Ctrl Pts',(-1.69742616027712E-8,-4.00767567982168,
-11.5859518710102));
#50614=CARTESIAN_POINT('Ctrl Pts',(-6.00000008491477,3.21424329763521,-9.29218325293956));
#50615=CARTESIAN_POINT('Ctrl Pts',(-6.00000008491454,4.8821256750661E-7,
-10.4040165138571));
#50616=CARTESIAN_POINT('Ctrl Pts',(-6.00000008491191,-3.21424242555678,
-9.29218355459962));
#50617=CARTESIAN_POINT('Origin',(6.,0.,0.));
#50618=CARTESIAN_POINT('Origin',(-6.,0.,0.));
#50619=CARTESIAN_POINT('Ctrl Pts',(6.00000005306065,-6.44014511329475,-7.42970798589525));
#50620=CARTESIAN_POINT('Ctrl Pts',(6.00000005305654,-9.01014216102169,-5.20200886777526));
#50621=CARTESIAN_POINT('Ctrl Pts',(6.00000005306017,-9.65438814672,-1.86247667057917));
#50622=CARTESIAN_POINT('Ctrl Pts',(-1.75871222825539E-8,-8.02988993733495,
-9.26372563720854));
#50623=CARTESIAN_POINT('Ctrl Pts',(-1.75922418001345E-8,-11.2342887621353,
-6.48612072033671));
#50624=CARTESIAN_POINT('Ctrl Pts',(-1.75877127682732E-8,-12.0375663695084,
-2.32222759153221));
#50625=CARTESIAN_POINT('Ctrl Pts',(-6.0000000832888,-6.44014510527518,-7.42970797666555));
#50626=CARTESIAN_POINT('Ctrl Pts',(-6.00000008329291,-9.01014214981644,
-5.20200886130693));
#50627=CARTESIAN_POINT('Ctrl Pts',(-6.00000008328928,-9.65438813471616,
-1.86247666825039));
#50628=CARTESIAN_POINT('Origin',(6.,0.,0.));
#50629=CARTESIAN_POINT('Origin',(-6.,0.,0.));
#50630=CARTESIAN_POINT('Ctrl Pts',(6.000000013908,-9.65439079723555,1.86246301485801));
#50631=CARTESIAN_POINT('Ctrl Pts',(6.00000001391134,-9.01014839527905,5.20200203764751));
#50632=CARTESIAN_POINT('Ctrl Pts',(6.00000001391262,-6.44014751247661,7.42970592721792));
#50633=CARTESIAN_POINT('Ctrl Pts',(-1.18290251301301E-8,-12.0375696345227,
2.32221055724884));
#50634=CARTESIAN_POINT('Ctrl Pts',(-1.18248668144419E-8,-11.2342964981915,
6.48611218277015));
#50635=CARTESIAN_POINT('Ctrl Pts',(-1.18232696314301E-8,-8.02989290222649,
9.26372303973634));
#50636=CARTESIAN_POINT('Ctrl Pts',(-6.00000003423866,-9.65439078915668,
1.86246301331147));
#50637=CARTESIAN_POINT('Ctrl Pts',(-6.00000003423532,-9.01014838773964,
5.20200203330458));
#50638=CARTESIAN_POINT('Ctrl Pts',(-6.00000003423404,-6.4401475070892,7.42970592100962));
#50639=CARTESIAN_POINT('Origin',(6.,0.,0.));
#50640=CARTESIAN_POINT('Origin',(-6.,0.,0.));
#50641=CARTESIAN_POINT('Ctrl Pts',(6.00000005197452,-3.21424126676338,9.29218396954236));
#50642=CARTESIAN_POINT('Ctrl Pts',(6.00000005200753,6.38646761553304E-7,
10.4040161294932));
#50643=CARTESIAN_POINT('Ctrl Pts',(6.00000005199697,3.21424240755215,9.29218357491516));
#50644=CARTESIAN_POINT('Ctrl Pts',(-1.77795276204544E-8,-4.00767422901088,
11.5859523713311));
#50645=CARTESIAN_POINT('Ctrl Pts',(-1.77383742545913E-8,7.96323979804973E-7,
12.9722394371238));
#50646=CARTESIAN_POINT('Ctrl Pts',(-1.7751541202668E-8,4.007675651458,11.5859518792905));
#50647=CARTESIAN_POINT('Ctrl Pts',(-6.00000008253,-3.2142412626098,9.29218395789083));
#50648=CARTESIAN_POINT('Ctrl Pts',(-6.00000008249699,6.38688659984361E-7,
10.4040161164194));
#50649=CARTESIAN_POINT('Ctrl Pts',(-6.00000008250755,3.21424240348237,9.29218356326364));
#50650=CARTESIAN_POINT('Origin',(6.,0.,0.));
#50651=CARTESIAN_POINT('Origin',(-6.,0.,0.));
#50652=CARTESIAN_POINT('Origin',(-7.4,0.,0.));
#50653=CARTESIAN_POINT('',(-7.4,-6.00000000007803,-10.3923048453649));
#50654=CARTESIAN_POINT('Origin',(-7.4,-6.75000000009103,-11.6913429510374));
#50655=CARTESIAN_POINT('Origin',(-6.,-6.75000000009103,-11.6913429510374));
#50656=CARTESIAN_POINT('',(-6.,-6.00000000007803,-10.3923048453649));
#50657=CARTESIAN_POINT('Origin',(-6.,-6.75000000009103,-11.6913429510374));
#50658=CARTESIAN_POINT('',(-6.,-6.00000000008095,-10.3923048453666));
#50659=CARTESIAN_POINT('Origin',(-7.4,-7.10542735750424E-15,1.23069611929084E-14));
#50660=CARTESIAN_POINT('',(-7.4,11.9999999999972,-9.50004519495451E-11));
#50661=CARTESIAN_POINT('Origin',(-7.4,13.5,-1.05000452776949E-10));
#50662=CARTESIAN_POINT('Origin',(-6.,13.5,-1.05000452776949E-10));
#50663=CARTESIAN_POINT('',(-6.,11.9999999999972,-9.50004519495451E-11));
#50664=CARTESIAN_POINT('Origin',(-6.,13.5,-1.05000452776949E-10));
#50665=CARTESIAN_POINT('',(-6.,12.,-9.33005511289567E-11));
#50666=CARTESIAN_POINT('Origin',(-6.,0.,0.));
#50667=CARTESIAN_POINT('Ctrl Pts',(-6.00000000001697,9.91329802718485,16.8993701947934));
#50668=CARTESIAN_POINT('Ctrl Pts',(-6.00000000001004,9.90992616536129,16.9013320391245));
#50669=CARTESIAN_POINT('Ctrl Pts',(-6.00000000000346,9.90655400604938,16.9032934158647));
#50670=CARTESIAN_POINT('Ctrl Pts',(-5.9999999999973,9.90318155035889,16.9052543221561));
#50671=CARTESIAN_POINT('Ctrl Pts',(-5.99999999993207,9.86751358933603,16.9259933727437));
#50672=CARTESIAN_POINT('Ctrl Pts',(-5.99999999990816,9.83181247294486,16.9466797991169));
#50673=CARTESIAN_POINT('Ctrl Pts',(-5.99999999990816,9.79607949297214,16.9673102431511));
#50674=CARTESIAN_POINT('Ctrl Pts',(-5.99999999990816,9.76034664910791,16.9879406086031));
#50675=CARTESIAN_POINT('Ctrl Pts',(-5.99999999993207,9.72458194169295,17.0085149922637));
#50676=CARTESIAN_POINT('Ctrl Pts',(-5.9999999999973,9.68878892570787,17.0290339621741));
#50677=CARTESIAN_POINT('Ctrl Pts',(-6.00000000000346,9.68540449666687,17.030974145077));
#50678=CARTESIAN_POINT('Ctrl Pts',(-6.00000000001005,9.68201981451976,17.0329138325694));
#50679=CARTESIAN_POINT('Ctrl Pts',(-6.00000000001698,9.67863488229756,17.0348530251257));
#50680=CARTESIAN_POINT('Ctrl Pts',(-5.59335880963394,10.1144382223412,17.2450574867612));
#50681=CARTESIAN_POINT('Ctrl Pts',(-5.59335897597996,10.1110305794363,17.2470401530682));
#50682=CARTESIAN_POINT('Ctrl Pts',(-5.59336249921667,10.0355852078339,17.290921844848));
#50683=CARTESIAN_POINT('Ctrl Pts',(-5.59336249921667,9.95658496883867,17.3365326540989));
#50684=CARTESIAN_POINT('Ctrl Pts',(-5.59335897597996,9.8808596232004,17.3799294166115));
#50685=CARTESIAN_POINT('Ctrl Pts',(-5.59335880963394,9.87743876235887,17.3818891887806));
#50686=CARTESIAN_POINT('Ctrl Pts',(-5.83074004399705,10.1164205431219,17.2484645412161));
#50687=CARTESIAN_POINT('Ctrl Pts',(-5.83074021197843,10.1130125214895,17.2504473136498));
#50688=CARTESIAN_POINT('Ctrl Pts',(-5.83074376985068,10.0375588131129,17.2943314352281));
#50689=CARTESIAN_POINT('Ctrl Pts',(-5.83074376985068,9.95855095808478,17.3399466416001));
#50690=CARTESIAN_POINT('Ctrl Pts',(-5.83074021197843,9.88281933979067,17.3833494090707));
#50691=CARTESIAN_POINT('Ctrl Pts',(-5.83074004399706,9.87939819767688,17.3853094561641));
#50692=CARTESIAN_POINT('Ctrl Pts',(-6.00000347488293,10.032698310508,17.1045694621537));
#50693=CARTESIAN_POINT('Ctrl Pts',(-6.00000357361913,10.0293041517828,17.1065440873071));
#50694=CARTESIAN_POINT('Ctrl Pts',(-6.0000056648664,9.9541574005552,17.150247947096));
#50695=CARTESIAN_POINT('Ctrl Pts',(-6.0000056648664,9.87547170337378,17.1956771555442));
#50696=CARTESIAN_POINT('Ctrl Pts',(-6.00000357361913,9.80004967494153,17.2389042212267));
#50697=CARTESIAN_POINT('Ctrl Pts',(-6.00000347488293,9.79664252003297,17.2408563363307));
#50698=CARTESIAN_POINT('Ctrl Pts',(-5.9999999999769,9.91330295482226,16.8993622715434));
#50699=CARTESIAN_POINT('Ctrl Pts',(-5.99999999996752,9.90992861632677,16.9013253647289));
#50700=CARTESIAN_POINT('Ctrl Pts',(-5.99999999976692,9.83522068214671,16.9447739934753));
#50701=CARTESIAN_POINT('Ctrl Pts',(-5.99999999976692,9.75699439892178,16.9899379591503));
#50702=CARTESIAN_POINT('Ctrl Pts',(-5.99999999996752,9.68201281558242,17.0329126136427));
#50703=CARTESIAN_POINT('Ctrl Pts',(-5.9999999999769,9.67862555776604,17.0348533299082));
#50704=CARTESIAN_POINT('Origin',(-5.47627002207303,-8.61187340852115,-14.9162298767998));
#50705=CARTESIAN_POINT('Ctrl Pts',(-5.67764080609729,10.3018641582453,17.1369991243702));
#50706=CARTESIAN_POINT('Ctrl Pts',(-3.78509387073152,11.0754256155854,16.6434327621663));
#50707=CARTESIAN_POINT('Ctrl Pts',(-2.06625885672274E-10,11.8428793690334,
16.139965968215));
#50708=CARTESIAN_POINT('Ctrl Pts',(3.78509387031849,11.0754256156717,16.6434327621122));
#50709=CARTESIAN_POINT('Ctrl Pts',(5.67764080547772,10.3018641584994,17.1369991242081));
#50710=CARTESIAN_POINT('Ctrl Pts',(-5.67764080609729,10.1072228441386,17.2516559727875));
#50711=CARTESIAN_POINT('Ctrl Pts',(-3.78509387073152,10.3777222791838,17.0590267241778));
#50712=CARTESIAN_POINT('Ctrl Pts',(-2.06625885672274E-10,10.7263798579245,
16.9926767289465));
#50713=CARTESIAN_POINT('Ctrl Pts',(3.78509387031849,10.3777222792149,17.0590267241666));
#50714=CARTESIAN_POINT('Ctrl Pts',(5.67764080547772,10.1072228442253,17.2516559727239));
#50715=CARTESIAN_POINT('Ctrl Pts',(-5.67764080609729,9.91156711681775,17.3647101833925));
#50716=CARTESIAN_POINT('Ctrl Pts',(-3.78509387073152,9.67398347124902,17.4658476572635));
#50717=CARTESIAN_POINT('Ctrl Pts',(-2.06625885672274E-10,9.51038903349187,
17.703153565319));
#50718=CARTESIAN_POINT('Ctrl Pts',(3.78509387031849,9.67398347122895,17.4658476572803));
#50719=CARTESIAN_POINT('Ctrl Pts',(5.67764080547772,9.9115671167385,17.3647101834302));
#50720=CARTESIAN_POINT('Ctrl Pts',(-5.67764080609729,9.71502525886082,17.476087692197));
#50721=CARTESIAN_POINT('Ctrl Pts',(-3.78509387073152,8.96560581046126,17.8630892232464));
#50722=CARTESIAN_POINT('Ctrl Pts',(-2.06625885672274E-10,8.21991077201455,
18.2569604826357));
#50723=CARTESIAN_POINT('Ctrl Pts',(3.78509387031849,8.9656058103827,17.8630892232866));
#50724=CARTESIAN_POINT('Ctrl Pts',(5.67764080547772,9.71502525861462,17.4760876923232));
#50725=CARTESIAN_POINT('Ctrl Pts',(-5.59336169625725,10.1144356127312,17.2450590604929));
#50726=CARTESIAN_POINT('Ctrl Pts',(-5.58009644052922,10.1196464220428,17.2417725309575));
#50727=CARTESIAN_POINT('Ctrl Pts',(-5.56074614028905,10.1272433830581,17.2369826570738));
#50728=CARTESIAN_POINT('Ctrl Pts',(-5.5352745867697,10.1371658803818,17.230732297382));
#50729=CARTESIAN_POINT('Ctrl Pts',(-5.50989210967062,10.1470536777985,17.2245037957864));
#50730=CARTESIAN_POINT('Ctrl Pts',(-5.47843096196783,10.1592509013913,17.2168250726809));
#50731=CARTESIAN_POINT('Ctrl Pts',(-5.44083463512139,10.173657996845,17.20776445536));
#50732=CARTESIAN_POINT('Ctrl Pts',(-5.41345000605419,10.1841519200026,17.2011648307354));
#50733=CARTESIAN_POINT('Ctrl Pts',(-5.38280993445691,10.1958174830056,17.1938325924219));
#50734=CARTESIAN_POINT('Ctrl Pts',(-5.34888648441894,10.2086021906203,17.1858024957018));
#50735=CARTESIAN_POINT('Ctrl Pts',(-5.30328426186975,10.2257882693128,17.1750078902796));
#50736=CARTESIAN_POINT('Ctrl Pts',(-5.25174934345171,10.2449983658296,17.1629512115716));
#50737=CARTESIAN_POINT('Ctrl Pts',(-5.19419938890525,10.2660693387113,17.1497389007395));
#50738=CARTESIAN_POINT('Ctrl Pts',(-5.15774847940527,10.2794152419642,17.1413705058342));
#50739=CARTESIAN_POINT('Ctrl Pts',(-5.11888420999868,10.2935068469148,17.1325389958659));
#50740=CARTESIAN_POINT('Ctrl Pts',(-5.07758279459578,10.3082935510227,17.1232765115135));
#50741=CARTESIAN_POINT('Ctrl Pts',(-5.01428717611989,10.330954604466,17.1090814852658));
#50742=CARTESIAN_POINT('Ctrl Pts',(-4.94526809232021,10.3552503413877,17.0938729633411));
#50743=CARTESIAN_POINT('Ctrl Pts',(-4.87042927208283,10.3809642545926,17.077788318177));
#50744=CARTESIAN_POINT('Ctrl Pts',(-4.84061551893453,10.3912079791507,17.0713806324482));
#50745=CARTESIAN_POINT('Ctrl Pts',(-4.80987804824268,10.4016762852682,17.064834182456));
#50746=CARTESIAN_POINT('Ctrl Pts',(-4.77821033099659,10.412353497345,17.0581587754218));
#50747=CARTESIAN_POINT('Ctrl Pts',(-4.70107154407374,10.4383619140844,17.0418982790671));
#50748=CARTESIAN_POINT('Ctrl Pts',(-4.61841362703178,10.4656129205248,17.0248708085413));
#50749=CARTESIAN_POINT('Ctrl Pts',(-4.53013604596957,10.4938502952785,17.0072373680404));
#50750=CARTESIAN_POINT('Ctrl Pts',(-4.5029336634511,10.5025515290473,17.0018036940787));
#50751=CARTESIAN_POINT('Ctrl Pts',(-4.47519762107238,10.5113461063362,16.9963126659037));
#50752=CARTESIAN_POINT('Ctrl Pts',(-4.44692485278666,10.5202256645349,16.9907694986755));
#50753=CARTESIAN_POINT('Ctrl Pts',(-4.35781685157385,10.5482115934237,16.9732989578675));
#50754=CARTESIAN_POINT('Ctrl Pts',(-4.26337760064318,10.5770449555143,16.9553085241858));
#50755=CARTESIAN_POINT('Ctrl Pts',(-4.16350896194574,10.6064361864374,16.9369795343976));
#50756=CARTESIAN_POINT('Ctrl Pts',(-4.13544397238834,10.6146956821079,16.9318287391759));
#50757=CARTESIAN_POINT('Ctrl Pts',(-4.10695019584106,10.6229989651231,16.9266513682192));
#50758=CARTESIAN_POINT('Ctrl Pts',(-4.07802541751535,10.6313389654857,16.9214518301025));
#50759=CARTESIAN_POINT('Ctrl Pts',(-3.98974865386987,10.6567921680142,16.9055831381382));
#50760=CARTESIAN_POINT('Ctrl Pts',(-3.89745734345782,10.6825893275272,16.8895067819342));
#50761=CARTESIAN_POINT('Ctrl Pts',(-3.80108980519495,10.7085129050089,16.8733587990892));
#50762=CARTESIAN_POINT('Ctrl Pts',(-3.75649682711523,10.7205087445128,16.865886504393));
#50763=CARTESIAN_POINT('Ctrl Pts',(-3.71103102545146,10.7325312845965,16.8583990963389));
#50764=CARTESIAN_POINT('Ctrl Pts',(-3.66468636943619,10.744556982028,16.8509112588752));
#50765=CARTESIAN_POINT('Ctrl Pts',(-3.62924738986443,10.7537528307461,16.8451854354097));
#50766=CARTESIAN_POINT('Ctrl Pts',(-3.59329450802114,10.7629504997334,16.8394593763233));
#50767=CARTESIAN_POINT('Ctrl Pts',(-3.55682518416501,10.7721390106437,16.8337399403038));
#50768=CARTESIAN_POINT('Ctrl Pts',(-3.51474448759309,10.7827413168748,16.8271404800932));
#50769=CARTESIAN_POINT('Ctrl Pts',(-3.47197612996742,10.793331619192,16.8205497196155));
#50770=CARTESIAN_POINT('Ctrl Pts',(-3.42851638099064,10.8038920970697,16.8139787813401));
#50771=CARTESIAN_POINT('Ctrl Pts',(-3.40678650650224,10.8091723360085,16.8106933122025));
#50772=CARTESIAN_POINT('Ctrl Pts',(-3.38488378417552,10.8144451187503,16.807412798479));
#50773=CARTESIAN_POINT('Ctrl Pts',(-3.36280774501983,10.8197081683452,16.8041386601616));
#50774=CARTESIAN_POINT('Ctrl Pts',(-3.35176972544199,10.8223396931427,16.8025015910029));
#50775=CARTESIAN_POINT('Ctrl Pts',(-3.34068837665689,10.824968784646,16.8008661156837));
#50776=CARTESIAN_POINT('Ctrl Pts',(-3.329563641285,10.8275951534672,16.7992324146027));
#50777=CARTESIAN_POINT('Ctrl Pts',(-3.32400127359906,10.8289083378778,16.7984155640621));
#50778=CARTESIAN_POINT('Ctrl Pts',(-3.31842805926641,10.8302208416174,16.7975991570803));
#50779=CARTESIAN_POINT('Ctrl Pts',(-3.31284399116671,10.8315326281783,16.7967832164111));
#50780=CARTESIAN_POINT('Ctrl Pts',(-3.30725992306701,10.8328444147391,16.7959672757419));
#50781=CARTESIAN_POINT('Ctrl Pts',(-3.30284643875128,10.8338793307461,16.7953235622363));
#50782=CARTESIAN_POINT('Ctrl Pts',(-3.29605921846272,10.8354657997138,16.7943368161553));
#50783=CARTESIAN_POINT('Ctrl Pts',(-3.26420947511142,10.8429104718047,16.7897064066363));
#50784=CARTESIAN_POINT('Ctrl Pts',(-3.23246236016097,10.8502239577099,16.7851582556376));
#50785=CARTESIAN_POINT('Ctrl Pts',(-3.20081930670522,10.8574079585424,16.7806912635389));
#50786=CARTESIAN_POINT('Ctrl Pts',(-3.02528053486219,10.8972609608712,16.7559107755265));
#50787=CARTESIAN_POINT('Ctrl Pts',(-2.85294730102254,10.9331280561869,16.7336284739108));
#50788=CARTESIAN_POINT('Ctrl Pts',(-2.68405734170938,10.965319242956,16.7136456366304));
#50789=CARTESIAN_POINT('Ctrl Pts',(-2.50183512068232,11.000051618844,16.6920853437245));
#50790=CARTESIAN_POINT('Ctrl Pts',(-2.32362196374915,11.0305054291441,16.673201482853));
#50791=CARTESIAN_POINT('Ctrl Pts',(-2.14968414968948,11.0570992276331,16.6567269918556));
#50792=CARTESIAN_POINT('Ctrl Pts',(-2.13682519185225,11.0590652666761,16.6555090578125));
#50793=CARTESIAN_POINT('Ctrl Pts',(-2.12398957734927,11.0610102121526,16.6543042908842));
#50794=CARTESIAN_POINT('Ctrl Pts',(-2.11117740281031,11.0629342344934,16.6531125827101));
#50795=CARTESIAN_POINT('Ctrl Pts',(-1.93621865371079,11.0892080368811,16.6368390164403));
#50796=CARTESIAN_POINT('Ctrl Pts',(-1.76563532274712,11.1115805033522,16.6230001913334));
#50797=CARTESIAN_POINT('Ctrl Pts',(-1.59966047058675,11.1305046374962,16.611306904573));
#50798=CARTESIAN_POINT('Ctrl Pts',(-1.55744727000663,11.1353177056208,16.608332893432));
#50799=CARTESIAN_POINT('Ctrl Pts',(-1.51553191253223,11.1399076896846,16.6054976961029));
#50800=CARTESIAN_POINT('Ctrl Pts',(-1.4739177101694,11.144281984227,16.6027966142496));
#50801=CARTESIAN_POINT('Ctrl Pts',(-1.30946665141412,11.1615683270611,16.592122475486));
#50802=CARTESIAN_POINT('Ctrl Pts',(-1.14972249376552,11.1754876800011,16.5835416973234));
#50803=CARTESIAN_POINT('Ctrl Pts',(-0.994867947072776,11.1865094923556,
16.5767553295172));
#50804=CARTESIAN_POINT('Ctrl Pts',(-0.92299758165632,11.1916248841758,16.5736056723421));
#50805=CARTESIAN_POINT('Ctrl Pts',(-0.852179763570651,11.1961158964594,
16.5708427266013));
#50806=CARTESIAN_POINT('Ctrl Pts',(-0.782429370895834,11.2000281392655,
16.5684376238844));
#50807=CARTESIAN_POINT('Ctrl Pts',(-0.63313574563942,11.2084018973047,16.5632897460024));
#50808=CARTESIAN_POINT('Ctrl Pts',(-0.488734980008948,11.2141260764705,
16.5597796943306));
#50809=CARTESIAN_POINT('Ctrl Pts',(-0.349348861740403,11.217649377585,16.5576195692001));
#50810=CARTESIAN_POINT('Ctrl Pts',(-0.262235556568476,11.219851364476,16.5562695377763));
#50811=CARTESIAN_POINT('Ctrl Pts',(-0.177080119921806,11.2211931540916,
16.5554472184677));
#50812=CARTESIAN_POINT('Ctrl Pts',(-0.0939047510573158,11.2217787688429,
16.5550866247168));
#50813=CARTESIAN_POINT('Ctrl Pts',(0.0408608595924439,11.2227276162076,
16.5545023695735));
#50814=CARTESIAN_POINT('Ctrl Pts',(0.170426606793054,11.2216933965749,16.5551294163659));
#50815=CARTESIAN_POINT('Ctrl Pts',(0.294722175599717,11.2191050882499,16.5567121120903));
#50816=CARTESIAN_POINT('Ctrl Pts',(0.343048653829801,11.2180987464541,16.5573274687857));
#50817=CARTESIAN_POINT('Ctrl Pts',(0.39057881329367,11.2168570902673,16.5580874888303));
#50818=CARTESIAN_POINT('Ctrl Pts',(0.437309818782762,11.2154038620237,16.5589779158886));
#50819=CARTESIAN_POINT('Ctrl Pts',(0.473889189930983,11.2142663265752,16.5596749105606));
#50820=CARTESIAN_POINT('Ctrl Pts',(0.509978917654201,11.2129991403243,16.5604518167948));
#50821=CARTESIAN_POINT('Ctrl Pts',(0.54557792579095,11.2116133394693,16.5613019839969));
#50822=CARTESIAN_POINT('Ctrl Pts',(0.57526124286935,11.2104578250789,16.562010874046));
#50823=CARTESIAN_POINT('Ctrl Pts',(0.604603386602295,11.2092198383741,16.5627707017228));
#50824=CARTESIAN_POINT('Ctrl Pts',(0.63360395775032,11.2079057382371,16.5635776247857));
#50825=CARTESIAN_POINT('Ctrl Pts',(0.66549434102706,11.2064606923165,16.5644649550944));
#50826=CARTESIAN_POINT('Ctrl Pts',(0.696971607506147,11.2049236195612,16.565409227215));
#50827=CARTESIAN_POINT('Ctrl Pts',(0.72803544167861,11.2033027340259,16.566405465553));
#50828=CARTESIAN_POINT('Ctrl Pts',(0.743567358764841,11.2024922912583,16.5669035847219));
#50829=CARTESIAN_POINT('Ctrl Pts',(0.758995917773488,11.2016608950771,16.5674146951219));
#50830=CARTESIAN_POINT('Ctrl Pts',(0.774321073540383,11.2008095475201,16.5679381887524));
#50831=CARTESIAN_POINT('Ctrl Pts',(0.78198365142383,11.2003838737417,16.5681999355677));
#50832=CARTESIAN_POINT('Ctrl Pts',(0.789620378496776,11.1999532121061,16.5684647781712));
#50833=CARTESIAN_POINT('Ctrl Pts',(0.797231250412047,11.1995176869327,16.568732641022));
#50834=CARTESIAN_POINT('Ctrl Pts',(0.804842122327319,11.1990821617592,16.5690005038728));
#50835=CARTESIAN_POINT('Ctrl Pts',(0.814188517455632,11.1985380526612,16.5693351922555));
#50836=CARTESIAN_POINT('Ctrl Pts',(0.819986296560143,11.1981966446342,16.5695452149902));
#50837=CARTESIAN_POINT('Ctrl Pts',(0.912968818906988,11.1927212757168,16.572913477781));
#50838=CARTESIAN_POINT('Ctrl Pts',(1.01085354095602,11.1860331615183,16.5770308029976));
#50839=CARTESIAN_POINT('Ctrl Pts',(1.11358303372777,11.1778352860948,16.582083555389));
#50840=CARTESIAN_POINT('Ctrl Pts',(1.22623354122959,11.1688457077178,16.587624273111));
#50841=CARTESIAN_POINT('Ctrl Pts',(1.34471056847521,11.1580407498769,16.594289802264));
#50842=CARTESIAN_POINT('Ctrl Pts',(1.46890926180699,11.1450008094671,16.6023433050796));
#50843=CARTESIAN_POINT('Ctrl Pts',(1.5153838009226,11.1401213280138,16.6053568861534));
#50844=CARTESIAN_POINT('Ctrl Pts',(1.56265915901644,11.1349285741414,16.6085650327152));
#50845=CARTESIAN_POINT('Ctrl Pts',(1.61072854597778,11.1293994266995,16.6119823022452));
#50846=CARTESIAN_POINT('Ctrl Pts',(1.74017461065096,11.1145099841127,16.6211846682527));
#50847=CARTESIAN_POINT('Ctrl Pts',(1.87538177215511,11.0971828232636,16.6319023435538));
#50848=CARTESIAN_POINT('Ctrl Pts',(2.01619359516505,11.0769554205139,16.6444269216333));
#50849=CARTESIAN_POINT('Ctrl Pts',(2.02948594729991,11.0750459944843,16.6456092165473));
#50850=CARTESIAN_POINT('Ctrl Pts',(2.04282821055348,11.073110706827,16.6468076250757));
#50851=CARTESIAN_POINT('Ctrl Pts',(2.05622023291824,11.0711491577268,16.6480224000727));
#50852=CARTESIAN_POINT('Ctrl Pts',(2.18611588770076,11.0521231512119,16.6598050860141));
#50853=CARTESIAN_POINT('Ctrl Pts',(2.32069562423643,11.0306273685102,16.6731268726598));
#50854=CARTESIAN_POINT('Ctrl Pts',(2.45980641009447,11.0062966218195,16.6882185446969));
#50855=CARTESIAN_POINT('Ctrl Pts',(2.57751721923923,10.9857087726287,16.7009886035811));
#50856=CARTESIAN_POINT('Ctrl Pts',(2.69847171418945,10.9630906897146,16.7150261711485));
#50857=CARTESIAN_POINT('Ctrl Pts',(2.8225610436928,10.9382204193277,16.7304718941296));
#50858=CARTESIAN_POINT('Ctrl Pts',(2.92925609545944,10.9168363503106,16.7437525059247));
#50859=CARTESIAN_POINT('Ctrl Pts',(3.0382684385968,10.8937870905112,16.7580742686304));
#50860=CARTESIAN_POINT('Ctrl Pts',(3.14952010302847,10.8689331626843,16.773525861029));
#50861=CARTESIAN_POINT('Ctrl Pts',(3.24640822738952,10.8472880892155,16.7869825208781));
#50862=CARTESIAN_POINT('Ctrl Pts',(3.3449946083139,10.8242742071437,16.8012961393943));
#50863=CARTESIAN_POINT('Ctrl Pts',(3.44522290323984,10.7998013031438,16.8165243674134));
#50864=CARTESIAN_POINT('Ctrl Pts',(3.44872500220626,10.7989461900056,16.8170564602885));
#50865=CARTESIAN_POINT('Ctrl Pts',(3.45222910514424,10.7980892956838,16.8175896697499));
#50866=CARTESIAN_POINT('Ctrl Pts',(3.45573520958506,10.7972306164005,16.8181239982249));
#50867=CARTESIAN_POINT('Ctrl Pts',(3.53381527626721,10.7781080440915,16.8300233593707));
#50868=CARTESIAN_POINT('Ctrl Pts',(3.61288815689678,10.7581001783265,16.8424777122093));
#50869=CARTESIAN_POINT('Ctrl Pts',(3.69292540360855,10.7371656451114,16.8555137028688));
#50870=CARTESIAN_POINT('Ctrl Pts',(3.69954958158591,10.7354330258674,16.8565926095752));
#50871=CARTESIAN_POINT('Ctrl Pts',(3.70618036529556,10.7336940593849,16.8576755002928));
#50872=CARTESIAN_POINT('Ctrl Pts',(3.71281773766541,10.7319487224599,16.8587623900056));
#50873=CARTESIAN_POINT('Ctrl Pts',(3.74627869988891,10.7231499614955,16.8642417233314));
#50874=CARTESIAN_POINT('Ctrl Pts',(3.77990711605412,10.7141892955713,16.8698226908658));
#50875=CARTESIAN_POINT('Ctrl Pts',(3.81370081314067,10.7050637966849,16.875507197817));
#50876=CARTESIAN_POINT('Ctrl Pts',(3.83394934879054,10.6995959726392,16.8789132454405));
#50877=CARTESIAN_POINT('Ctrl Pts',(3.85425722354602,10.6940689701107,16.8823564659578));
#50878=CARTESIAN_POINT('Ctrl Pts',(3.8746239679551,10.6884821641204,16.8858372669345));
#50879=CARTESIAN_POINT('Ctrl Pts',(3.88480734015964,10.6856887611252,16.8875776674229));
#50880=CARTESIAN_POINT('Ctrl Pts',(3.89500542977759,10.6828804072687,16.8893274630326));
#50881=CARTESIAN_POINT('Ctrl Pts',(3.90521817699174,10.6800570246534,16.8910867046236));
#50882=CARTESIAN_POINT('Ctrl Pts',(3.91032455059882,10.6786453333457,16.8919663254192));
#50883=CARTESIAN_POINT('Ctrl Pts',(3.91543458860496,10.6772298848486,16.8928483077104));
#50884=CARTESIAN_POINT('Ctrl Pts',(3.92054828348311,10.675810669452,16.8937326578414));
#50885=CARTESIAN_POINT('Ctrl Pts',(3.92566197836127,10.6743914540554,16.8946170079723));
#50886=CARTESIAN_POINT('Ctrl Pts',(3.93254611569438,10.6724762287361,16.895810469717));
#50887=CARTESIAN_POINT('Ctrl Pts',(3.93590033118955,10.6715417128619,16.8963928180947));
#50888=CARTESIAN_POINT('Ctrl Pts',(3.94215184180214,10.6697999834134,16.8974781857667));
#50889=CARTESIAN_POINT('Ctrl Pts',(3.94838636554841,10.6680589024911,16.8985631804318));
#50890=CARTESIAN_POINT('Ctrl Pts',(3.95460391944251,10.6663185318536,16.8996477635096));
#50891=CARTESIAN_POINT('Ctrl Pts',(4.02981766553141,10.6452652691942,16.9127679644141));
#50892=CARTESIAN_POINT('Ctrl Pts',(4.10254807846764,10.6243167745196,16.9258274386836));
#50893=CARTESIAN_POINT('Ctrl Pts',(4.17282587990966,10.6035771746011,16.9387612046173));
#50894=CARTESIAN_POINT('Ctrl Pts',(4.24075388489511,10.5835310203709,16.9512625193824));
#50895=CARTESIAN_POINT('Ctrl Pts',(4.30639057590207,10.5636799432642,16.9636464456261));
#50896=CARTESIAN_POINT('Ctrl Pts',(4.36976383142682,10.5441095500937,16.9758595468081));
#50897=CARTESIAN_POINT('Ctrl Pts',(4.43121450937757,10.5251328710808,16.9877021346836));
#50898=CARTESIAN_POINT('Ctrl Pts',(4.4905370197739,10.5064200395023,16.9993841484537));
#50899=CARTESIAN_POINT('Ctrl Pts',(4.54775645034366,10.4880420601335,17.010861252205));
#50900=CARTESIAN_POINT('Ctrl Pts',(4.60351117571902,10.4701345209906,17.022044564611));
#50901=CARTESIAN_POINT('Ctrl Pts',(4.65726912320849,10.4525448611279,17.0330333575748));
#50902=CARTESIAN_POINT('Ctrl Pts',(4.70905288634901,10.4353327752034,17.0437903335549));
#50903=CARTESIAN_POINT('Ctrl Pts',(4.75987167753236,10.4184414303612,17.0543468571241));
#50904=CARTESIAN_POINT('Ctrl Pts',(4.80878918164385,10.401913682668,17.0646801492342));
#50905=CARTESIAN_POINT('Ctrl Pts',(4.85582595139816,10.3858007083745,17.0747581939838));
#50906=CARTESIAN_POINT('Ctrl Pts',(4.90207917597453,10.3699561462908,17.0846683572354));
#50907=CARTESIAN_POINT('Ctrl Pts',(4.94651380654213,10.3545126244029,17.0943317286087));
#50908=CARTESIAN_POINT('Ctrl Pts',(4.98914847135176,10.339514167028,17.103720703033));
#50909=CARTESIAN_POINT('Ctrl Pts',(4.98949673383339,10.339391651699,17.1037973971397));
#50910=CARTESIAN_POINT('Ctrl Pts',(4.9898448762078,10.3392691660419,17.1038740729512));
#50911=CARTESIAN_POINT('Ctrl Pts',(4.99019289848491,10.3391467100793,17.103950730453));
#50912=CARTESIAN_POINT('Ctrl Pts',(5.03325928084211,10.3239932683266,17.1134367935652));
#50913=CARTESIAN_POINT('Ctrl Pts',(5.07448668094134,10.3092949186304,17.122642277991));
#50914=CARTESIAN_POINT('Ctrl Pts',(5.11389326224849,10.2950925682147,17.1315414279138));
#50915=CARTESIAN_POINT('Ctrl Pts',(5.15369851217184,10.2807465354191,17.1405306087824));
#50916=CARTESIAN_POINT('Ctrl Pts',(5.19164591938828,10.2669065813742,17.1492072354232));
#50917=CARTESIAN_POINT('Ctrl Pts',(5.22775300182795,10.2536103929835,17.1575474221413));
#50918=CARTESIAN_POINT('Ctrl Pts',(5.2645392540316,10.2400641049303,17.1660444867422));
#50919=CARTESIAN_POINT('Ctrl Pts',(5.2994153039346,10.2270822307516,17.1741923411339));
#50920=CARTESIAN_POINT('Ctrl Pts',(5.33239832281596,10.2147000575187,17.1819683887808));
#50921=CARTESIAN_POINT('Ctrl Pts',(5.36641335057651,10.2019304572657,17.1899877419372));
#50922=CARTESIAN_POINT('Ctrl Pts',(5.39841504349945,10.1897986823172,17.1976116558626));
#50923=CARTESIAN_POINT('Ctrl Pts',(5.42842066614186,10.1783385418951,17.2048181455367));
#50924=CARTESIAN_POINT('Ctrl Pts',(5.45996866099105,10.1662893184773,17.2123950687631));
#50925=CARTESIAN_POINT('Ctrl Pts',(5.4893101307546,10.1549825787082,17.2195105357911));
#50926=CARTESIAN_POINT('Ctrl Pts',(5.51646318129051,10.1444519643233,17.2261421901412));
#50927=CARTESIAN_POINT('Ctrl Pts',(5.54440810081889,10.1336142438549,17.2329672445457));
#50928=CARTESIAN_POINT('Ctrl Pts',(5.57003513091122,10.1235985826726,17.2392798431885));
#50929=CARTESIAN_POINT('Ctrl Pts',(5.5933616601283,10.1144355424442,17.2450591004647));
#50930=CARTESIAN_POINT('Ctrl Pts',(-5.8463733010073,10.2457285249441,16.949086006428));
#50931=CARTESIAN_POINT('Ctrl Pts',(-5.81071183845632,10.2597918252233,16.9400660732668));
#50932=CARTESIAN_POINT('Ctrl Pts',(-5.69191996054832,10.3062057866106,16.9103322240196));
#50933=CARTESIAN_POINT('Ctrl Pts',(-5.48049741245665,10.38625136138,16.8592278496599));
#50934=CARTESIAN_POINT('Ctrl Pts',(-5.20215554396402,10.4866532305168,16.7953196613188));
#50935=CARTESIAN_POINT('Ctrl Pts',(-4.8941493129655,10.5916725641874,16.7286085483737));
#50936=CARTESIAN_POINT('Ctrl Pts',(-4.55276913235771,10.7006290440657,16.6595003165788));
#50937=CARTESIAN_POINT('Ctrl Pts',(-4.17238356880022,10.8128325911058,16.5884207304473));
#50938=CARTESIAN_POINT('Ctrl Pts',(-3.74657439469726,10.9269282942293,16.5162276658936));
#50939=CARTESIAN_POINT('Ctrl Pts',(-3.27003381845878,11.040174418721,16.4446648480292));
#50940=CARTESIAN_POINT('Ctrl Pts',(-2.7386885358987,11.1484347150953,16.3763620028265));
#50941=CARTESIAN_POINT('Ctrl Pts',(-2.14775624702771,11.2465694809231,16.3145802149633));
#50942=CARTESIAN_POINT('Ctrl Pts',(-1.49664356863671,11.3274377514689,16.2638265111147));
#50943=CARTESIAN_POINT('Ctrl Pts',(-0.805427675793565,11.3814836225517,
16.2300643076986));
#50944=CARTESIAN_POINT('Ctrl Pts',(-0.113326822037204,11.4024992910628,
16.2170495538243));
#50945=CARTESIAN_POINT('Ctrl Pts',(0.53617904501584,11.3923351802427,16.2233294580765));
#50946=CARTESIAN_POINT('Ctrl Pts',(1.11984701048415,11.3587959812637,16.2442251910393));
#50947=CARTESIAN_POINT('Ctrl Pts',(1.63691896299704,11.3100216749588,16.2747552179192));
#50948=CARTESIAN_POINT('Ctrl Pts',(2.09763398174282,11.251537564875,16.3114723839704));
#50949=CARTESIAN_POINT('Ctrl Pts',(2.51226399840957,11.1867259151241,16.352250871855));
#50950=CARTESIAN_POINT('Ctrl Pts',(2.88624760864777,11.1183574017561,16.3953378720742));
#50951=CARTESIAN_POINT('Ctrl Pts',(3.22326429257175,11.0487107246453,16.4392863234276));
#50952=CARTESIAN_POINT('Ctrl Pts',(3.5276819915208,10.9792486772936,16.4831632372597));
#50953=CARTESIAN_POINT('Ctrl Pts',(3.80292724584096,10.9110843998516,16.5262573892699));
#50954=CARTESIAN_POINT('Ctrl Pts',(4.05164145117326,10.8451121085737,16.567997008493));
#50955=CARTESIAN_POINT('Ctrl Pts',(4.27616841465673,10.7819862052094,16.6079630105325));
#50956=CARTESIAN_POINT('Ctrl Pts',(4.47886355109388,10.7220901690397,16.6459087067021));
#50957=CARTESIAN_POINT('Ctrl Pts',(4.66208312275494,10.665574932594,16.6817355221251));
#50958=CARTESIAN_POINT('Ctrl Pts',(4.82814550061594,10.6124043230814,16.7154642022297));
#50959=CARTESIAN_POINT('Ctrl Pts',(4.97929162609239,10.5623996874633,16.7472065332161));
#50960=CARTESIAN_POINT('Ctrl Pts',(5.11758619996814,10.5153019885475,16.7771259862501));
#50961=CARTESIAN_POINT('Ctrl Pts',(5.24463111730424,10.4709008672825,16.8053557320035));
#50962=CARTESIAN_POINT('Ctrl Pts',(5.36151871454931,10.4290880708158,16.8319644193218));
#50963=CARTESIAN_POINT('Ctrl Pts',(5.46895006319928,10.3898443662126,16.8569640935366));
#50964=CARTESIAN_POINT('Ctrl Pts',(5.56756311190895,10.3531353396374,16.8803762516901));
#50965=CARTESIAN_POINT('Ctrl Pts',(5.65800137336307,10.3188910900565,16.9022446821647));
#50966=CARTESIAN_POINT('Ctrl Pts',(5.74091079056104,10.2870108104913,16.9226324749478));
#50967=CARTESIAN_POINT('Ctrl Pts',(5.80284291074193,10.2628628056022,16.9380991790113));
#50968=CARTESIAN_POINT('Ctrl Pts',(5.83721317799972,10.2493407521394,16.9467699786851));
#50969=CARTESIAN_POINT('Ctrl Pts',(5.8463475785683,10.2457385387449,16.9490805710439));
#50970=CARTESIAN_POINT('Ctrl Pts',(-5.81214048410627,10.2495588935256,17.0923498933693));
#50971=CARTESIAN_POINT('Ctrl Pts',(-5.77669382793542,10.2635850491913,17.0833822545817));
#50972=CARTESIAN_POINT('Ctrl Pts',(-5.65860909322797,10.3098800300599,17.0538187973008));
#50973=CARTESIAN_POINT('Ctrl Pts',(-5.44840462333573,10.3897376720867,17.0029977853316));
#50974=CARTESIAN_POINT('Ctrl Pts',(-5.17162939485601,10.4899212401681,16.9394359874193));
#50975=CARTESIAN_POINT('Ctrl Pts',(-4.86534603850363,10.5947210968573,16.8730845645311));
#50976=CARTESIAN_POINT('Ctrl Pts',(-4.52588138421029,10.7034540320265,16.8043505326476));
#50977=CARTESIAN_POINT('Ctrl Pts',(-4.14764846583199,10.8154286837038,16.7336596024664));
#50978=CARTESIAN_POINT('Ctrl Pts',(-3.72427691755522,10.9292912020793,16.6618663983565));
#50979=CARTESIAN_POINT('Ctrl Pts',(-3.25050020753745,11.0423043121599,16.590705725778));
#50980=CARTESIAN_POINT('Ctrl Pts',(-2.72227770251836,11.15033962184,16.522792381771));
#50981=CARTESIAN_POINT('Ctrl Pts',(-2.13486068559317,11.2482679994735,16.4613676733713));
#50982=CARTESIAN_POINT('Ctrl Pts',(-1.48765672131871,11.3289640567501,16.4109103803494));
#50983=CARTESIAN_POINT('Ctrl Pts',(-0.800609992132193,11.3828936033401,
16.3773462735944));
#50984=CARTESIAN_POINT('Ctrl Pts',(-0.112656412763598,11.4038639976422,
16.3644072235699));
#50985=CARTESIAN_POINT('Ctrl Pts',(0.532982300217447,11.3937217510365,16.3706507298466));
#50986=CARTESIAN_POINT('Ctrl Pts',(1.11313112312745,11.3602548559676,16.3914240619341));
#50987=CARTESIAN_POINT('Ctrl Pts',(1.62709005444509,11.3115851034049,16.4217752045558));
#50988=CARTESIAN_POINT('Ctrl Pts',(2.08504101968106,11.2532253592082,16.458278206289));
#50989=CARTESIAN_POINT('Ctrl Pts',(2.49719897986104,11.1885503635626,16.4988204899594));
#50990=CARTESIAN_POINT('Ctrl Pts',(2.86896944948211,11.1203248275706,16.5416599927212));
#50991=CARTESIAN_POINT('Ctrl Pts',(3.20400785780452,11.0508227302716,16.585358255767));
#50992=CARTESIAN_POINT('Ctrl Pts',(3.50665331436974,10.9815039732325,16.6289876548034));
#50993=CARTESIAN_POINT('Ctrl Pts',(3.78030901480038,10.913479603221,16.6718408587469));
#50994=CARTESIAN_POINT('Ctrl Pts',(4.02759771527588,10.8476422395178,16.713349047024));
#50995=CARTESIAN_POINT('Ctrl Pts',(4.25084657567494,10.7846452014045,16.7530951266326));
#50996=CARTESIAN_POINT('Ctrl Pts',(4.45239467779643,10.7248714440366,16.7908333899151));
#50997=CARTESIAN_POINT('Ctrl Pts',(4.63458237830649,10.6684718441651,16.8264654138834));
#50998=CARTESIAN_POINT('Ctrl Pts',(4.79971278139797,10.6154105462015,16.8600114553183));
#50999=CARTESIAN_POINT('Ctrl Pts',(4.95001237250278,10.5655095013055,16.8915823408029));
#51000=CARTESIAN_POINT('Ctrl Pts',(5.08753268216066,10.5185104478698,16.9213403268495));
#51001=CARTESIAN_POINT('Ctrl Pts',(5.21386523142879,10.4742037174266,16.9494175499695));
#51002=CARTESIAN_POINT('Ctrl Pts',(5.33009497893724,10.432481545317,16.9758819840215));
#51003=CARTESIAN_POINT('Ctrl Pts',(5.43691796894504,10.3933249838663,17.0007453247105));
#51004=CARTESIAN_POINT('Ctrl Pts',(5.53496769036703,10.3566998929772,17.0240287063314));
#51005=CARTESIAN_POINT('Ctrl Pts',(5.62488345963333,10.3225366416241,17.0457754968935));
#51006=CARTESIAN_POINT('Ctrl Pts',(5.7073074330221,10.2907346235822,17.0660483615429));
#51007=CARTESIAN_POINT('Ctrl Pts',(5.76887172101577,10.2666481665187,17.0814266234462));
#51008=CARTESIAN_POINT('Ctrl Pts',(5.8030360081916,10.25316138296,17.0900473914712));
#51009=CARTESIAN_POINT('Ctrl Pts',(5.81211556016687,10.2495686125498,17.0923446256674));
#51010=CARTESIAN_POINT('Ctrl Pts',(-5.75637626233754,10.1837201417723,17.2118536969054));
#51011=CARTESIAN_POINT('Ctrl Pts',(-5.72124177183205,10.1976628995511,17.2029857527102));
#51012=CARTESIAN_POINT('Ctrl Pts',(-5.60419197535415,10.2436849161472,17.1737500606415));
#51013=CARTESIAN_POINT('Ctrl Pts',(-5.39580847211975,10.3230818240993,17.1234891203679));
#51014=CARTESIAN_POINT('Ctrl Pts',(-5.12142638366231,10.422693332199,17.0606301153465));
#51015=CARTESIAN_POINT('Ctrl Pts',(-4.81781612208664,10.5268917270792,16.9950214475401));
#51016=CARTESIAN_POINT('Ctrl Pts',(-4.4813608879283,10.6349920036448,16.9270704092175));
#51017=CARTESIAN_POINT('Ctrl Pts',(-4.10654736969582,10.746302542252,16.8572016117894));
#51018=CARTESIAN_POINT('Ctrl Pts',(-3.6870885478391,10.8594742827435,16.7862625466688));
#51019=CARTESIAN_POINT('Ctrl Pts',(-3.21779412721873,10.9717844531648,16.7159688619445));
#51020=CARTESIAN_POINT('Ctrl Pts',(-2.69468813604672,11.0791301006442,16.6489027355764));
#51021=CARTESIAN_POINT('Ctrl Pts',(-2.11308889884579,11.1764171542247,16.5882613465945));
#51022=CARTESIAN_POINT('Ctrl Pts',(-1.47241765961012,11.2565721948536,16.5384595621686));
#51023=CARTESIAN_POINT('Ctrl Pts',(-0.792400884630377,11.3101333762541,
16.5053368948279));
#51024=CARTESIAN_POINT('Ctrl Pts',(-0.111506716586297,11.3309592637304,
16.4925680681425));
#51025=CARTESIAN_POINT('Ctrl Pts',(0.527523869479962,11.3208869439873,16.4987295537772));
#51026=CARTESIAN_POINT('Ctrl Pts',(1.1017189194122,11.2876496094038,16.5192293101599));
#51027=CARTESIAN_POINT('Ctrl Pts',(1.61044309404501,11.2393099586255,16.5491830326528));
#51028=CARTESIAN_POINT('Ctrl Pts',(2.06377799636403,11.1813404285803,16.5852128420941));
#51029=CARTESIAN_POINT('Ctrl Pts',(2.471835069819,11.1170910356783,16.6252361147083));
#51030=CARTESIAN_POINT('Ctrl Pts',(2.8399587584862,11.049307038833,16.6675348168625));
#51031=CARTESIAN_POINT('Ctrl Pts',(3.17175878031802,10.9802473078334,16.7106894353203));
#51032=CARTESIAN_POINT('Ctrl Pts',(3.47152170733553,10.9113626526124,16.7537839684948));
#51033=CARTESIAN_POINT('Ctrl Pts',(3.74260813031438,10.8437577418764,16.7961193514205));
#51034=CARTESIAN_POINT('Ctrl Pts',(3.98760666094978,10.7783205269083,16.8371328805859));
#51035=CARTESIAN_POINT('Ctrl Pts',(4.2088142490919,10.715701342194,16.8764114516135));
#51036=CARTESIAN_POINT('Ctrl Pts',(4.40854095591408,10.6562818812914,16.9137111633865));
#51037=CARTESIAN_POINT('Ctrl Pts',(4.58909944985825,10.6002131348132,16.948933651213));
#51038=CARTESIAN_POINT('Ctrl Pts',(4.75276676007855,10.5474603926735,16.9820979165458));
#51039=CARTESIAN_POINT('Ctrl Pts',(4.9017451190426,10.4978474838834,17.0133125992741));
#51040=CARTESIAN_POINT('Ctrl Pts',(5.03806430892174,10.4511183877206,17.0427373075265));
#51041=CARTESIAN_POINT('Ctrl Pts',(5.16329886926211,10.4070653142114,17.0705019749049));
#51042=CARTESIAN_POINT('Ctrl Pts',(5.27852170413661,10.3655817362365,17.0966731628961));
#51043=CARTESIAN_POINT('Ctrl Pts',(5.38442057509479,10.3266493824282,17.1212618367615));
#51044=CARTESIAN_POINT('Ctrl Pts',(5.48162162178821,10.2902348018342,17.1442883625899));
#51045=CARTESIAN_POINT('Ctrl Pts',(5.57075720609127,10.2562691463666,17.1657951865642));
#51046=CARTESIAN_POINT('Ctrl Pts',(5.65246304775603,10.22465260939,17.1858439664136));
#51047=CARTESIAN_POINT('Ctrl Pts',(5.71348822191349,10.2007079571406,17.2010518028893));
#51048=CARTESIAN_POINT('Ctrl Pts',(5.74735238451962,10.1873010376137,17.2095768782592));
#51049=CARTESIAN_POINT('Ctrl Pts',(5.75635212911942,10.1837295664958,17.2118486069642));
#51050=CARTESIAN_POINT('Ctrl Pts',(-5.69417655262727,10.0659550938109,17.2751196141304));
#51051=CARTESIAN_POINT('Ctrl Pts',(-5.65936703870486,10.0797907515111,17.2663717926203));
#51052=CARTESIAN_POINT('Ctrl Pts',(-5.54339967722055,10.1254596259212,17.2375325657588));
#51053=CARTESIAN_POINT('Ctrl Pts',(-5.33694689371025,10.2042475512871,17.1879568994398));
#51054=CARTESIAN_POINT('Ctrl Pts',(-5.06513642187847,10.3030878613366,17.1259669913686));
#51055=CARTESIAN_POINT('Ctrl Pts',(-4.76442569371336,10.4064653591534,17.0612832475125));
#51056=CARTESIAN_POINT('Ctrl Pts',(-4.43125897055681,10.5136948306663,16.9943122258059));
#51057=CARTESIAN_POINT('Ctrl Pts',(-4.06020584535738,10.6240854956199,16.9254766893615));
#51058=CARTESIAN_POINT('Ctrl Pts',(-3.64507557266572,10.7362955187036,16.8556150441424));
#51059=CARTESIAN_POINT('Ctrl Pts',(-3.18076844304463,10.8476227562837,16.7864187240801));
#51060=CARTESIAN_POINT('Ctrl Pts',(-2.66338764499731,10.954000403985,16.7204284189311));
#51061=CARTESIAN_POINT('Ctrl Pts',(-2.0883338678018,11.0503844700961,16.660784761969));
#51062=CARTESIAN_POINT('Ctrl Pts',(-1.45505107693594,11.1297758587313,16.6118203238809));
#51063=CARTESIAN_POINT('Ctrl Pts',(-0.783022235707487,11.1828161548434,
16.5792630691678));
#51064=CARTESIAN_POINT('Ctrl Pts',(-0.110188903191932,11.2034373433835,
16.5667129564925));
#51065=CARTESIAN_POINT('Ctrl Pts',(0.521281123172272,11.1934641215224,16.5727689772592));
#51066=CARTESIAN_POINT('Ctrl Pts',(1.08869926730035,11.160551584388,16.5929179599979));
#51067=CARTESIAN_POINT('Ctrl Pts',(1.59148386671455,11.1126783998152,16.6223631937593));
#51068=CARTESIAN_POINT('Ctrl Pts',(2.03960018326053,11.0552595066297,16.6577887420727));
#51069=CARTESIAN_POINT('Ctrl Pts',(2.44303760716516,10.9916096766539,16.6971505484544));
#51070=CARTESIAN_POINT('Ctrl Pts',(2.80706804716866,10.9244464844029,16.7387613933694));
#51071=CARTESIAN_POINT('Ctrl Pts',(3.13524621666746,10.8560073839613,16.7812259290856));
#51072=CARTESIAN_POINT('Ctrl Pts',(3.4317966606496,10.7877303502555,16.8236428919148));
#51073=CARTESIAN_POINT('Ctrl Pts',(3.7000296333615,10.7207111125095,16.8653236203182));
#51074=CARTESIAN_POINT('Ctrl Pts',(3.94249333601839,10.6558311443833,16.9057130400457));
#51075=CARTESIAN_POINT('Ctrl Pts',(4.1614491203754,10.5937366998712,16.9444029536336));
#51076=CARTESIAN_POINT('Ctrl Pts',(4.35917319283043,10.5348078145404,16.9811516032074));
#51077=CARTESIAN_POINT('Ctrl Pts',(4.53794624447247,10.4791957319084,17.0158605727866));
#51078=CARTESIAN_POINT('Ctrl Pts',(4.70001547858034,10.4268674063087,17.0485471811394));
#51079=CARTESIAN_POINT('Ctrl Pts',(4.84755564240603,10.3776493108809,17.0793172456371));
#51080=CARTESIAN_POINT('Ctrl Pts',(4.98257207879255,10.3312885255543,17.108327008496));
#51081=CARTESIAN_POINT('Ctrl Pts',(5.10662033523898,10.2875798190821,17.1357036274334));
#51082=CARTESIAN_POINT('Ctrl Pts',(5.22075984776427,10.2464183166914,17.1615118961645));
#51083=CARTESIAN_POINT('Ctrl Pts',(5.32566908184452,10.2077866315443,17.1857618662613));
#51084=CARTESIAN_POINT('Ctrl Pts',(5.42196592776539,10.171652230936,17.2084729378999));
#51085=CARTESIAN_POINT('Ctrl Pts',(5.51027491708016,10.1379473510794,17.2296863832694));
#51086=CARTESIAN_POINT('Ctrl Pts',(5.59122442533868,10.1065733678469,17.249462542477));
#51087=CARTESIAN_POINT('Ctrl Pts',(5.65168521434887,10.082812435781,17.2644640766896));
#51088=CARTESIAN_POINT('Ctrl Pts',(5.68523639401818,10.0695083794281,17.2728736875046));
#51089=CARTESIAN_POINT('Ctrl Pts',(5.69415298772929,10.0659643045932,17.2751146638057));
#51090=CARTESIAN_POINT('Ctrl Pts',(-5.73644387793316,10.2877346863031,16.9337810350644));
#51091=CARTESIAN_POINT('Ctrl Pts',(-5.66411037901632,10.3157397302585,16.9158630923735));
#51092=CARTESIAN_POINT('Ctrl Pts',(-5.58548128436389,10.345652422121,16.8967577750015));
#51093=CARTESIAN_POINT('Ctrl Pts',(-5.50055659235639,10.3771725884928,16.8766547495792));
#51094=CARTESIAN_POINT('Ctrl Pts',(-5.41741952890743,10.4080292688012,16.8569748842709));
#51095=CARTESIAN_POINT('Ctrl Pts',(-5.32824911790177,10.4404263047604,16.8363389710469));
#51096=CARTESIAN_POINT('Ctrl Pts',(-5.23304535782008,10.4740375249085,16.8149530194337));
#51097=CARTESIAN_POINT('Ctrl Pts',(-5.13477096437687,10.5087328170914,16.7928773007731));
#51098=CARTESIAN_POINT('Ctrl Pts',(-5.03006775494901,10.544722138694,16.7700022177755));
#51099=CARTESIAN_POINT('Ctrl Pts',(-4.91893572786536,10.5815974241754,16.7465854223469));
#51100=CARTESIAN_POINT('Ctrl Pts',(-4.80780370078171,10.6184727096568,16.7231686269183));
#51101=CARTESIAN_POINT('Ctrl Pts',(-4.69024285604226,10.6562339622146,16.699210116964));
#51102=CARTESIAN_POINT('Ctrl Pts',(-4.56625319197586,10.6944229852801,16.6749991241893));
#51103=CARTESIAN_POINT('Ctrl Pts',(-4.44622762213337,10.7313910607216,16.6515621851015));
#51104=CARTESIAN_POINT('Ctrl Pts',(-4.32017773748643,10.7687597473468,16.6278888032932));
#51105=CARTESIAN_POINT('Ctrl Pts',(-4.18810353803503,10.8060686117601,16.6042695666098));
#51106=CARTESIAN_POINT('Ctrl Pts',(-4.05161768088946,10.8446236994286,16.579861379566));
#51107=CARTESIAN_POINT('Ctrl Pts',(-3.90869832845551,10.8831151723678,16.5555108443855));
#51108=CARTESIAN_POINT('Ctrl Pts',(-3.75934548073319,10.9209853985322,16.5315698407257));
#51109=CARTESIAN_POINT('Ctrl Pts',(-3.60999263301087,10.9588556246966,16.5076288370659));
#51110=CARTESIAN_POINT('Ctrl Pts',(-3.45420629000018,10.9961046088078,16.4840973614737));
#51111=CARTESIAN_POINT('Ctrl Pts',(-3.29198645170111,11.0321243382672,16.4613590428076));
#51112=CARTESIAN_POINT('Ctrl Pts',(-3.21175044287551,11.0499401575966,16.4501123792904));
#51113=CARTESIAN_POINT('Ctrl Pts',(-3.12994053214575,11.0674544734859,16.4390602443938));
#51114=CARTESIAN_POINT('Ctrl Pts',(-3.04655672419778,11.0845891516794,16.428251951463));
#51115=CARTESIAN_POINT('Ctrl Pts',(-3.00486482022379,11.0931564907761,16.4228478049976));
#51116=CARTESIAN_POINT('Ctrl Pts',(-2.9627794332184,11.1016288762653,16.4175046172165));
#51117=CARTESIAN_POINT('Ctrl Pts',(-2.92030057443875,11.1099962543511,16.4122287688642));
#51118=CARTESIAN_POINT('Ctrl Pts',(-2.89906114504893,11.1141799433939,16.4095908446881));
#51119=CARTESIAN_POINT('Ctrl Pts',(-2.87772334714861,11.1183373778354,16.4069697552516));
#51120=CARTESIAN_POINT('Ctrl Pts',(-2.85628718059005,11.1224672837817,16.4043663037934));
#51121=CARTESIAN_POINT('Ctrl Pts',(-2.84556909731076,11.1245322367549,16.4030645780643));
#51122=CARTESIAN_POINT('Ctrl Pts',(-2.83482642183447,11.1265903074306,16.4017672618231));
#51123=CARTESIAN_POINT('Ctrl Pts',(-2.82405915415227,11.128641335461,16.4004744562027));
#51124=CARTESIAN_POINT('Ctrl Pts',(-2.81867552031118,11.1296668494762,16.3998280533925));
#51125=CARTESIAN_POINT('Ctrl Pts',(-2.81328573841659,11.1306906028192,16.399182778237));
#51126=CARTESIAN_POINT('Ctrl Pts',(-2.80788980846857,11.131712575377,16.3985386434259));
#51127=CARTESIAN_POINT('Ctrl Pts',(-2.80249387852054,11.1327345479348,16.3978945086147));
#51128=CARTESIAN_POINT('Ctrl Pts',(-2.79531885000099,11.1340885934571,16.3970411026223));
#51129=CARTESIAN_POINT('Ctrl Pts',(-2.79168357446015,11.1347731305368,16.3966096727281));
#51130=CARTESIAN_POINT('Ctrl Pts',(-2.04577399270848,11.2752309200605,16.3080860688738));
#51131=CARTESIAN_POINT('Ctrl Pts',(-1.29987672192816,11.3594145287903,16.2552346233375));
#51132=CARTESIAN_POINT('Ctrl Pts',(-0.553962161422298,11.3872886566001,
16.2380598751199));
#51133=CARTESIAN_POINT('Ctrl Pts',(-0.369309316851761,11.3941889602844,
16.2338082271684));
#51134=CARTESIAN_POINT('Ctrl Pts',(-0.184655412730056,11.3976383199709,
16.2317430976133));
#51135=CARTESIAN_POINT('Ctrl Pts',(1.07492380563405E-12,11.3976358484824,
16.2318648996165));
#51136=CARTESIAN_POINT('Ctrl Pts',(6.93460617175366E-5,11.3976358475542,
16.2318649453584));
#51137=CARTESIAN_POINT('Ctrl Pts',(0.000138692122572115,11.3976358461392,
16.2318649914088));
#51138=CARTESIAN_POINT('Ctrl Pts',(0.000208038183639729,11.3976358442374,
16.2318650377675));
#51139=CARTESIAN_POINT('Ctrl Pts',(0.465532887795667,11.397623082842,16.2321761135824));
#51140=CARTESIAN_POINT('Ctrl Pts',(0.93085773638585,11.3756953661397,16.2460734179067));
#51141=CARTESIAN_POINT('Ctrl Pts',(1.39618258395421,11.3318637068722,16.2735530077344));
#51142=CARTESIAN_POINT('Ctrl Pts',(1.62884500773839,11.3099478772385,16.2872928026482));
#51143=CARTESIAN_POINT('Ctrl Pts',(1.86150743137387,11.2825562791905,16.304427889156));
#51144=CARTESIAN_POINT('Ctrl Pts',(2.09416985349857,11.2496916138933,16.3249560837549));
#51145=CARTESIAN_POINT('Ctrl Pts',(2.21050106456092,11.2332592812448,16.3352201810544));
#51146=CARTESIAN_POINT('Ctrl Pts',(2.32683227716226,11.2154586948964,16.3463325557894));
#51147=CARTESIAN_POINT('Ctrl Pts',(2.44316348898306,11.1962902777384,16.3582928083244));
#51148=CARTESIAN_POINT('Ctrl Pts',(2.50132909489346,11.1867060691593,16.3642729345919));
#51149=CARTESIAN_POINT('Ctrl Pts',(2.55949470071167,11.1767799037176,16.3704650303328));
#51150=CARTESIAN_POINT('Ctrl Pts',(2.61766030645565,11.1665118394568,16.3768690421441));
#51151=CARTESIAN_POINT('Ctrl Pts',(2.64674310932764,11.1613778073265,16.3800710480498));
#51152=CARTESIAN_POINT('Ctrl Pts',(2.6758259121901,11.1561583005427,16.3833260329749));
#51153=CARTESIAN_POINT('Ctrl Pts',(2.70490871504478,11.1508533266947,16.3866339898157));
#51154=CARTESIAN_POINT('Ctrl Pts',(2.73217384272104,11.1458799137123,16.3897351993539));
#51155=CARTESIAN_POINT('Ctrl Pts',(2.75943897039075,11.1408313831947,16.3928829662399));
#51156=CARTESIAN_POINT('Ctrl Pts',(2.78670409806019,11.135707741571,16.3960772844348));
#51157=CARTESIAN_POINT('Ctrl Pts',(2.78852177323815,11.1353661654627,16.3962902389811));
#51158=CARTESIAN_POINT('Ctrl Pts',(2.7917217802675,11.1347639810534,16.3966656658502));
#51159=CARTESIAN_POINT('Ctrl Pts',(2.79215712359383,11.1346820117671,16.396716768754));
#51160=CARTESIAN_POINT('Ctrl Pts',(2.80635022328155,11.1320096422105,16.398382829915));
#51161=CARTESIAN_POINT('Ctrl Pts',(2.82656862381981,11.1281855968624,16.4007798930427));
#51162=CARTESIAN_POINT('Ctrl Pts',(2.85281232520862,11.1231359515119,16.4039546435487));
#51163=CARTESIAN_POINT('Ctrl Pts',(2.87905632057885,11.1180862495954,16.4071294296181));
#51164=CARTESIAN_POINT('Ctrl Pts',(2.91132575179097,11.1118109200526,16.4110819203721));
#51165=CARTESIAN_POINT('Ctrl Pts',(2.94962061884499,11.1041919647284,16.4158866461266));
#51166=CARTESIAN_POINT('Ctrl Pts',(2.98791593921205,11.0965729192152,16.4206914287567));
#51167=CARTESIAN_POINT('Ctrl Pts',(3.03223683807327,11.0876102158814,16.4263484663581));
#51168=CARTESIAN_POINT('Ctrl Pts',(3.08258331542866,11.0771417830772,16.4329601381591));
#51169=CARTESIAN_POINT('Ctrl Pts',(3.13293077927501,11.0666731451541,16.4395719395095));
#51170=CARTESIAN_POINT('Ctrl Pts',(3.18930405774871,11.0546987185142,16.4471384121424));
#51171=CARTESIAN_POINT('Ctrl Pts',(3.25170315084976,11.0410123546368,16.455789792554));
#51172=CARTESIAN_POINT('Ctrl Pts',(3.31410294885478,11.0273258361485,16.4644412706976));
#51173=CARTESIAN_POINT('Ctrl Pts',(3.38252869763159,11.0119273413779,16.4741776807566));
#51174=CARTESIAN_POINT('Ctrl Pts',(3.45698039718018,10.9945666515411,16.4851571204632));
#51175=CARTESIAN_POINT('Ctrl Pts',(3.53143351514183,10.9772056309579,16.4961367693441));
#51176=CARTESIAN_POINT('Ctrl Pts',(3.61191281348369,10.957882340169,16.5083594947387));
#51177=CARTESIAN_POINT('Ctrl Pts',(3.69841829220576,10.9363024868442,16.5220112677421));
#51178=CARTESIAN_POINT('Ctrl Pts',(3.77371777394213,10.9175181069955,16.533894577876));
#51179=CARTESIAN_POINT('Ctrl Pts',(3.85358328686691,10.8970232575265,16.5468611021372));
#51180=CARTESIAN_POINT('Ctrl Pts',(3.9380148309801,10.8745966667332,16.5610506886561));
#51181=CARTESIAN_POINT('Ctrl Pts',(3.98561399049141,10.8619534433541,16.5690502153639));
#51182=CARTESIAN_POINT('Ctrl Pts',(4.03466435231841,10.8486958059363,16.5774387518806));
#51183=CARTESIAN_POINT('Ctrl Pts',(4.08516592204748,10.8347805625576,16.5862436136911));
#51184=CARTESIAN_POINT('Ctrl Pts',(4.11041670691202,10.8278229408682,16.5906460445963));
#51185=CARTESIAN_POINT('Ctrl Pts',(4.13603028420328,10.820700881924,16.5951525547403));
#51186=CARTESIAN_POINT('Ctrl Pts',(4.16200666602408,10.8134087423863,16.5997667430059));
#51187=CARTESIAN_POINT('Ctrl Pts',(4.17499485693448,10.8097626726174,16.6020738371387));
#51188=CARTESIAN_POINT('Ctrl Pts',(4.18807374838966,10.8060740804569,16.6044078506744));
#51189=CARTESIAN_POINT('Ctrl Pts',(4.20124334024048,10.8023422462392,16.6067692381573));
#51190=CARTESIAN_POINT('Ctrl Pts',(4.2078281361659,10.8004763291304,16.6079499318988));
#51191=CARTESIAN_POINT('Ctrl Pts',(4.21443560715221,10.7985996013682,16.6091374691186));
#51192=CARTESIAN_POINT('Ctrl Pts',(4.22106575320089,10.7967119720507,16.6103319072856));
#51193=CARTESIAN_POINT('Ctrl Pts',(4.22769589924957,10.7948243427332,16.6115263454525));
#51194=CARTESIAN_POINT('Ctrl Pts',(4.23593743780306,10.7924713596529,16.6130152502058));
#51195=CARTESIAN_POINT('Ctrl Pts',(4.2410242164579,10.7910162879412,16.6139359822734));
#51196=CARTESIAN_POINT('Ctrl Pts',(4.3703949964166,10.7540098099686,16.6373527325978));
#51197=CARTESIAN_POINT('Ctrl Pts',(4.49373992023327,10.7170369625673,16.6607652887357));
#51198=CARTESIAN_POINT('Ctrl Pts',(4.61105898920646,10.6805483865231,16.6838892449829));
#51199=CARTESIAN_POINT('Ctrl Pts',(4.72934236899263,10.6437598905363,16.707203269914));
#51200=CARTESIAN_POINT('Ctrl Pts',(4.84150042710314,10.6074637179565,16.7302238946238));
#51201=CARTESIAN_POINT('Ctrl Pts',(4.94753316486883,10.5720763462447,16.7526882263514));
#51202=CARTESIAN_POINT('Ctrl Pts',(5.0527582749985,10.5369585122244,16.7749814522913));
#51203=CARTESIAN_POINT('Ctrl Pts',(5.15195101980991,10.5027356280522,16.7967268648974));
#51204=CARTESIAN_POINT('Ctrl Pts',(5.2451114006037,10.4697704218163,16.8176954447603));
#51205=CARTESIAN_POINT('Ctrl Pts',(5.33934432336991,10.4364256919352,16.8389054328465));
#51206=CARTESIAN_POINT('Ctrl Pts',(5.42740518308715,10.4043678502821,16.8593205447843));
#51207=CARTESIAN_POINT('Ctrl Pts',(5.50929398110152,10.3739263971821,16.8787326755966));
#51208=CARTESIAN_POINT('Ctrl Pts',(5.59118277911589,10.3434849440822,16.8981448064088));
#51209=CARTESIAN_POINT('Ctrl Pts',(5.66689951542738,10.3146598775781,16.9165539572384));
#51210=CARTESIAN_POINT('Ctrl Pts',(5.73644419138209,10.2877345675704,16.9337810842153));
#51211=CARTESIAN_POINT('Ctrl Pts',(-5.843530343931,6.40544352337877,7.94861259136425));
#51212=CARTESIAN_POINT('Ctrl Pts',(-3.895686895954,7.5011174617541,7.93455912692836));
#51213=CARTESIAN_POINT('Ctrl Pts',(0.0001666015277053,8.59741135523303,
7.91991927812663));
#51214=CARTESIAN_POINT('Ctrl Pts',(3.896020099009,7.50102369434968,7.93456037909693));
#51215=CARTESIAN_POINT('Ctrl Pts',(5.844030148514,6.40516236820509,7.94861619754387));
#51216=CARTESIAN_POINT('Ctrl Pts',(-5.843530343931,7.02207626292374,8.43809571307178));
#51217=CARTESIAN_POINT('Ctrl Pts',(-3.895686895954,8.04135143326013,8.43217787140772));
#51218=CARTESIAN_POINT('Ctrl Pts',(0.0001666015277053,9.06227985942128,
8.42460953303723));
#51219=CARTESIAN_POINT('Ctrl Pts',(3.896020099009,8.04126411194929,8.43217851873466));
#51220=CARTESIAN_POINT('Ctrl Pts',(5.844030148514,7.02181471204778,8.4380972315977));
#51221=CARTESIAN_POINT('Ctrl Pts',(-5.843530343931,8.22106606565346,9.63752218475374));
#51222=CARTESIAN_POINT('Ctrl Pts',(-3.895686895954,9.0918900806387,9.61305666122109));
#51223=CARTESIAN_POINT('Ctrl Pts',(0.0001666015277053,9.96180836750487,
9.58947319442851));
#51224=CARTESIAN_POINT('Ctrl Pts',(3.896020099009,9.09181567541838,9.61305867834303));
#51225=CARTESIAN_POINT('Ctrl Pts',(5.844030148514,8.22084260802873,9.63752846273313));
#51226=CARTESIAN_POINT('Ctrl Pts',(-5.843530343931,9.557830382581,11.8732201358499));
#51227=CARTESIAN_POINT('Ctrl Pts',(-3.895686895954,10.2763900681474,11.7328262526707));
#51228=CARTESIAN_POINT('Ctrl Pts',(0.0001666015277054,10.9955725683271,
11.5921560888775));
#51229=CARTESIAN_POINT('Ctrl Pts',(3.896020099009,10.2763285555535,11.7328382843686));
#51230=CARTESIAN_POINT('Ctrl Pts',(5.844030148514,9.55764599673119,11.8732561615899));
#51231=CARTESIAN_POINT('Ctrl Pts',(-5.843530343931,10.2973084060429,14.4766646280625));
#51232=CARTESIAN_POINT('Ctrl Pts',(-3.895686895954,10.972803840489,14.1582376025316));
#51233=CARTESIAN_POINT('Ctrl Pts',(0.0001666015277051,11.6469750209433,
13.8399443642564));
#51234=CARTESIAN_POINT('Ctrl Pts',(3.896020099009,10.9727461777759,14.1582648265603));
#51235=CARTESIAN_POINT('Ctrl Pts',(5.844030148514,10.2971350706646,14.4767463379645));
#51236=CARTESIAN_POINT('Ctrl Pts',(-5.843530343931,10.3258757620666,16.2770693368357));
#51237=CARTESIAN_POINT('Ctrl Pts',(-3.895686895954,11.0553896705852,15.8346874489017));
#51238=CARTESIAN_POINT('Ctrl Pts',(0.0001666015277058,11.7876699867244,
15.3921227606342));
#51239=CARTESIAN_POINT('Ctrl Pts',(3.896020099009,11.0553270377124,15.8347253020195));
#51240=CARTESIAN_POINT('Ctrl Pts',(5.844030148514,10.3256885653351,16.2771828541457));
#51241=CARTESIAN_POINT('Ctrl Pts',(-5.843530343931,10.2251611575698,17.159314850801));
#51242=CARTESIAN_POINT('Ctrl Pts',(-3.895686895954,11.0033631004084,16.661943431523));
#51243=CARTESIAN_POINT('Ctrl Pts',(0.0001666015277058,11.7816843623499,
16.1645455758364));
#51244=CARTESIAN_POINT('Ctrl Pts',(3.896020099009,11.0032965296051,16.6619859745965));
#51245=CARTESIAN_POINT('Ctrl Pts',(5.844030148514,10.2249614672313,17.1594424786931));
#51246=CARTESIAN_POINT('',(5.73278665926685,6.65588954520332,8.10254295276797));
#51247=CARTESIAN_POINT('Ctrl Pts',(5.73278665926685,6.65588954520332,8.10254295276797));
#51248=CARTESIAN_POINT('Ctrl Pts',(5.73375888620758,6.99202136443375,8.38525883796284));
#51249=CARTESIAN_POINT('Ctrl Pts',(5.73463611962229,7.31053409065034,8.68980953075562));
#51250=CARTESIAN_POINT('Ctrl Pts',(5.73539800543143,7.60866057961232,9.01380228009759));
#51251=CARTESIAN_POINT('Ctrl Pts',(5.7358525360122,7.78651873701786,9.20709189220604));
#51252=CARTESIAN_POINT('Ctrl Pts',(5.73626601263528,7.95712059774996,9.4073003281479));
#51253=CARTESIAN_POINT('Ctrl Pts',(5.73663411343628,8.1198745794402,9.61391171627937));
#51254=CARTESIAN_POINT('Ctrl Pts',(5.73680084043203,8.19359211099577,9.70749395227842));
#51255=CARTESIAN_POINT('Ctrl Pts',(5.73695825843206,8.26569958462528,9.80238969913112));
#51256=CARTESIAN_POINT('Ctrl Pts',(5.73710596584106,8.33615716844976,9.89853823864722));
#51257=CARTESIAN_POINT('Ctrl Pts',(5.73762707028046,8.5847280422313,10.2377455344846));
#51258=CARTESIAN_POINT('Ctrl Pts',(5.73808755028673,8.81277732605215,10.5925991843482));
#51259=CARTESIAN_POINT('Ctrl Pts',(5.7384511752828,9.01856735398873,10.9604768333983));
#51260=CARTESIAN_POINT('Ctrl Pts',(5.73875620561864,9.19119630418346,11.2690745482264));
#51261=CARTESIAN_POINT('Ctrl Pts',(5.73899308048749,9.34816097570251,11.5868367228597));
#51262=CARTESIAN_POINT('Ctrl Pts',(5.73914041321966,9.48841420861512,11.9121967999306));
#51263=CARTESIAN_POINT('Ctrl Pts',(5.73916137871713,9.50837229094943,11.9584956486033));
#51264=CARTESIAN_POINT('Ctrl Pts',(5.73918053104131,9.52799194545917,12.0049483191629));
#51265=CARTESIAN_POINT('Ctrl Pts',(5.73919780856664,9.54727141212101,12.0515497100057));
#51266=CARTESIAN_POINT('Ctrl Pts',(5.73934667546454,9.71338746988924,12.4530773803036));
#51267=CARTESIAN_POINT('Ctrl Pts',(5.73938505124021,9.85421925005767,12.8656005110965));
#51268=CARTESIAN_POINT('Ctrl Pts',(5.73932699215388,9.96862920325058,13.2858435141329));
#51269=CARTESIAN_POINT('Ctrl Pts',(5.73927451059684,10.0720482004273,13.665715271193));
#51270=CARTESIAN_POINT('Ctrl Pts',(5.73914323250993,10.1538778096344,14.0518946860673));
#51271=CARTESIAN_POINT('Ctrl Pts',(5.73894353985269,10.2132541970825,14.4419342915027));
#51272=CARTESIAN_POINT('Ctrl Pts',(5.73893603912074,10.215484456184,14.4565847176629));
#51273=CARTESIAN_POINT('Ctrl Pts',(5.7389283964977,10.2176830628771,14.4712406634984));
#51274=CARTESIAN_POINT('Ctrl Pts',(5.73892061255889,10.2198499690232,14.4859019942209));
#51275=CARTESIAN_POINT('Ctrl Pts',(5.73870205362586,10.2806927771524,14.897565662103));
#51276=CARTESIAN_POINT('Ctrl Pts',(5.73837208348003,10.3165409130782,15.3134787414899));
#51277=CARTESIAN_POINT('Ctrl Pts',(5.73794343795648,10.3271730562598,15.7305176790661));
#51278=CARTESIAN_POINT('Ctrl Pts',(5.73753129228904,10.3373959362556,16.1315035329577));
#51279=CARTESIAN_POINT('Ctrl Pts',(5.73702792165988,10.3243069727082,16.5335294805983));
#51280=CARTESIAN_POINT('Ctrl Pts',(5.73644464706835,10.2877344027066,16.9337810712876));
#51281=CARTESIAN_POINT('Ctrl Pts',(-5.7327897547535,6.65588713928974,8.10254235490551));
#51282=CARTESIAN_POINT('Ctrl Pts',(-5.37903306893985,6.85199393532157,8.1046567014769));
#51283=CARTESIAN_POINT('Ctrl Pts',(-5.01625135988035,7.03117595252705,8.1037396655483));
#51284=CARTESIAN_POINT('Ctrl Pts',(-4.6460573053147,7.19212481080525,8.10101244173934));
#51285=CARTESIAN_POINT('Ctrl Pts',(-4.37169929920774,7.31140713664976,8.098991243189));
#51286=CARTESIAN_POINT('Ctrl Pts',(-4.09327000298005,7.42067123776832,8.0959775624238));
#51287=CARTESIAN_POINT('Ctrl Pts',(-3.81142588255404,7.5194084477233,8.09248201619626));
#51288=CARTESIAN_POINT('Ctrl Pts',(-3.57233107521407,7.60316947901887,8.08951666446013));
#51289=CARTESIAN_POINT('Ctrl Pts',(-3.33077878398178,7.67935406186102,8.08620479042068));
#51290=CARTESIAN_POINT('Ctrl Pts',(-3.08716977929676,7.74769216833986,8.08286047253372));
#51291=CARTESIAN_POINT('Ctrl Pts',(-3.04361334355598,7.75991078212773,8.0822625202235));
#51292=CARTESIAN_POINT('Ctrl Pts',(-2.99999115841705,7.77187869233266,8.08166353316822));
#51293=CARTESIAN_POINT('Ctrl Pts',(-2.95630551460348,7.783594544369,8.08106530891504));
#51294=CARTESIAN_POINT('Ctrl Pts',(-2.75784036736928,7.83682000006536,8.07834755877739));
#51295=CARTESIAN_POINT('Ctrl Pts',(-2.55806426654974,7.88488745634565,8.07569240201061));
#51296=CARTESIAN_POINT('Ctrl Pts',(-2.35724376584312,7.92759984415222,8.07318988699391));
#51297=CARTESIAN_POINT('Ctrl Pts',(-2.16325032346373,7.96886018915527,8.07077244703639));
#51298=CARTESIAN_POINT('Ctrl Pts',(-1.96828228463633,8.00512331767119,8.06849745748605));
#51299=CARTESIAN_POINT('Ctrl Pts',(-1.77257993163001,8.03625973710509,8.06644561273015));
#51300=CARTESIAN_POINT('Ctrl Pts',(-1.57996180764706,8.06690545294229,8.0644261046276));
#51301=CARTESIAN_POINT('Ctrl Pts',(-1.38663233238503,8.09258461604006,8.06262277294384));
#51302=CARTESIAN_POINT('Ctrl Pts',(-1.19282060581187,8.11322305871492,8.06111193464765));
#51303=CARTESIAN_POINT('Ctrl Pts',(-0.994702314851606,8.13432009480826,
8.05956752499583));
#51304=CARTESIAN_POINT('Ctrl Pts',(-0.796080102885767,8.15014941282128,
8.05832876462942));
#51305=CARTESIAN_POINT('Ctrl Pts',(-0.59719868379037,8.16068915179076,8.05747633859425));
#51306=CARTESIAN_POINT('Ctrl Pts',(-0.408374169346901,8.17069592417969,
8.05666701747757));
#51307=CARTESIAN_POINT('Ctrl Pts',(-0.219315999797635,8.17593478931577,
8.0562059446956));
#51308=CARTESIAN_POINT('Ctrl Pts',(-0.0302336110270316,8.1764388741411,
8.05616136972021));
#51309=CARTESIAN_POINT('Ctrl Pts',(-0.0201629718368322,8.17646572199525,
8.05615899563082));
#51310=CARTESIAN_POINT('Ctrl Pts',(-0.0100922639442051,8.17647915107978,
8.05615780282402));
#51311=CARTESIAN_POINT('Ctrl Pts',(-2.15189915158098E-5,8.17647917058928,
8.05615780154597));
#51312=CARTESIAN_POINT('Ctrl Pts',(-1.43459939669992E-5,8.17647917060317,
8.05615780154506));
#51313=CARTESIAN_POINT('Ctrl Pts',(-7.17299643689954E-6,8.17647917061026,
8.05615780154476));
#51314=CARTESIAN_POINT('Ctrl Pts',(1.07469816165171E-12,8.17647917061055,
8.05615780154506));
#51315=CARTESIAN_POINT('Ctrl Pts',(0.18943579711537,8.17647917827287,8.05615780943295));
#51316=CARTESIAN_POINT('Ctrl Pts',(0.378858612885447,8.17173001867108,8.05657949522161));
#51317=CARTESIAN_POINT('Ctrl Pts',(0.568057836295289,8.16219561556172,8.05735427144708));
#51318=CARTESIAN_POINT('Ctrl Pts',(0.769443680254818,8.15204708650211,8.05817895223188));
#51319=CARTESIAN_POINT('Ctrl Pts',(0.970576200329105,8.13647662698269,8.05940367890533));
#51320=CARTESIAN_POINT('Ctrl Pts',(1.17120141047458,8.11550423737469,8.06094475234051));
#51321=CARTESIAN_POINT('Ctrl Pts',(1.36703229033906,8.09503302387756,8.06244899882344));
#51322=CARTESIAN_POINT('Ctrl Pts',(1.56237981688653,8.0694154937033,8.06425464009947));
#51323=CARTESIAN_POINT('Ctrl Pts',(1.75700778088661,8.03872640369093,8.06628301653371));
#51324=CARTESIAN_POINT('Ctrl Pts',(1.95878306564105,8.00691031853628,8.06838588101525));
#51325=CARTESIAN_POINT('Ctrl Pts',(2.15978496848557,7.96964334863419,8.07072813122281));
#51326=CARTESIAN_POINT('Ctrl Pts',(2.35975028992456,7.92706670092953,8.07322138619571));
#51327=CARTESIAN_POINT('Ctrl Pts',(2.55971561136355,7.88449005322488,8.0757146411686));
#51328=CARTESIAN_POINT('Ctrl Pts',(2.75864435139702,7.83660410476304,8.07835888608861));
#51329=CARTESIAN_POINT('Ctrl Pts',(2.95627331052934,7.783603529238,8.08106520728543));
#51330=CARTESIAN_POINT('Ctrl Pts',(3.19882930073948,7.71855432220565,8.08438675702491));
#51331=CARTESIAN_POINT('Ctrl Pts',(3.4394292441421,7.64573016185184,8.08773178925052));
#51332=CARTESIAN_POINT('Ctrl Pts',(3.67768100681231,7.56538588953542,8.09079284969756));
#51333=CARTESIAN_POINT('Ctrl Pts',(3.96257907131849,7.46931135300075,8.09445322218305));
#51334=CARTESIAN_POINT('Ctrl Pts',(4.24411946379384,7.36248453264372,8.09770721708057));
#51335=CARTESIAN_POINT('Ctrl Pts',(4.52163169077914,7.24541657642252,8.10003238704001));
#51336=CARTESIAN_POINT('Ctrl Pts',(4.88861255955403,7.09060645959825,8.10310718090057));
#51337=CARTESIAN_POINT('Ctrl Pts',(5.24854925703452,6.91789304800925,8.10455499757065));
#51338=CARTESIAN_POINT('Ctrl Pts',(5.5998912593694,6.72853477684402,8.10319558761065));
#51339=CARTESIAN_POINT('Ctrl Pts',(5.64432825807231,6.70458514032395,8.10302365229341));
#51340=CARTESIAN_POINT('Ctrl Pts',(5.68862777036575,6.68036922783882,8.10280688011413));
#51341=CARTESIAN_POINT('Ctrl Pts',(5.73278665919283,6.65588954516668,8.10254295270319));
#51342=CARTESIAN_POINT('Ctrl Pts',(-5.84424404754221,6.60982561991869,8.11494609712149));
#51343=CARTESIAN_POINT('Ctrl Pts',(-5.61083003141265,6.74470098061893,8.11886064004874));
#51344=CARTESIAN_POINT('Ctrl Pts',(-4.83877334320068,7.15840509626737,8.12664832309506));
#51345=CARTESIAN_POINT('Ctrl Pts',(-3.4739964644456,7.71340775361018,8.11883512382398));
#51346=CARTESIAN_POINT('Ctrl Pts',(-1.74184413166379,8.12609642238157,8.0994612827205));
#51347=CARTESIAN_POINT('Ctrl Pts',(0.00546389148000443,8.26248517348045,
8.09063507506571));
#51348=CARTESIAN_POINT('Ctrl Pts',(1.75277317531105,8.12437426464466,8.09956481566326));
#51349=CARTESIAN_POINT('Ctrl Pts',(3.48454184722242,7.71000021151431,8.11895024293463));
#51350=CARTESIAN_POINT('Ctrl Pts',(4.84546451123536,7.15511681611458,8.12662863672576));
#51351=CARTESIAN_POINT('Ctrl Pts',(5.61402512777244,6.74285772429285,8.11880770412169));
#51352=CARTESIAN_POINT('Ctrl Pts',(5.84435329640009,6.60976254643618,8.1149443088601));
#51353=CARTESIAN_POINT('Ctrl Pts',(-5.72536415493237,6.40694478209925,7.90745488128355));
#51354=CARTESIAN_POINT('Ctrl Pts',(-5.49665064991634,6.53847614205489,7.91194597692562));
#51355=CARTESIAN_POINT('Ctrl Pts',(-4.74015267330978,6.94198191326917,7.92158137971138));
#51356=CARTESIAN_POINT('Ctrl Pts',(-3.40298511486256,7.48347479664365,7.91659886786272));
#51357=CARTESIAN_POINT('Ctrl Pts',(-1.70614179652305,7.88616883277403,7.89960762793621));
#51358=CARTESIAN_POINT('Ctrl Pts',(0.0053517777339369,8.01925550389425,
7.89162120971071));
#51359=CARTESIAN_POINT('Ctrl Pts',(1.71684729000813,7.88448836413846,7.89970073156132));
#51360=CARTESIAN_POINT('Ctrl Pts',(3.41331638270933,7.48014986638464,7.91669525727088));
#51361=CARTESIAN_POINT('Ctrl Pts',(4.74670889513164,6.93877415913986,7.92154621389461));
#51362=CARTESIAN_POINT('Ctrl Pts',(5.4997813999677,6.53667859342793,7.91188514788741));
#51363=CARTESIAN_POINT('Ctrl Pts',(5.72547120249297,6.40688327557001,7.90745282059258));
#51364=CARTESIAN_POINT('Ctrl Pts',(-5.7194149784166,6.40360983160495,7.59392594682071));
#51365=CARTESIAN_POINT('Ctrl Pts',(-5.49136603844791,6.5337759497367,7.59841892092599));
#51366=CARTESIAN_POINT('Ctrl Pts',(-4.73696752025829,6.93323604774542,7.60809613134932));
#51367=CARTESIAN_POINT('Ctrl Pts',(-3.40255792642537,7.47005167289838,7.60327372800129));
#51368=CARTESIAN_POINT('Ctrl Pts',(-1.70680590972389,7.87002583666974,7.58642156961049));
#51369=CARTESIAN_POINT('Ctrl Pts',(0.00535495091468471,8.00237757076679,
7.5784734111445));
#51370=CARTESIAN_POINT('Ctrl Pts',(1.71751142262118,7.86835521722273,7.58651415030087));
#51371=CARTESIAN_POINT('Ctrl Pts',(3.41287492734901,7.46675197777174,7.60336893780237));
#51372=CARTESIAN_POINT('Ctrl Pts',(4.74350648116296,6.93005899438803,7.60806032165927));
#51373=CARTESIAN_POINT('Ctrl Pts',(5.49448772027338,6.53199702945591,7.5983580829355));
#51374=CARTESIAN_POINT('Ctrl Pts',(5.71952172603672,6.40354895607179,7.59392388778129));
#51375=CARTESIAN_POINT('Ctrl Pts',(-5.83025895397455,6.60198838021539,7.3778062669314));
#51376=CARTESIAN_POINT('Ctrl Pts',(-5.59840732478868,6.73365395594057,7.38172521605155));
#51377=CARTESIAN_POINT('Ctrl Pts',(-4.83128643333009,7.13784639841503,7.38961116079864));
#51378=CARTESIAN_POINT('Ctrl Pts',(-3.47299336195986,7.68185251078179,7.38217434496566));
#51379=CARTESIAN_POINT('Ctrl Pts',(-1.74340617768423,8.08814661704716,7.36312745843566));
#51380=CARTESIAN_POINT('Ctrl Pts',(0.0054713540043873,8.22280750341084,
7.35439118899612));
#51381=CARTESIAN_POINT('Ctrl Pts',(1.75433527096293,8.08644761515946,7.36322976207848));
#51382=CARTESIAN_POINT('Ctrl Pts',(3.48350520534007,7.67850429798651,7.38228669101555));
#51383=CARTESIAN_POINT('Ctrl Pts',(4.83793702132043,7.13463029795999,7.38958996088061));
#51384=CARTESIAN_POINT('Ctrl Pts',(5.60158110182676,6.73185449623961,7.38167225921689));
#51385=CARTESIAN_POINT('Ctrl Pts',(5.83036749767586,6.60192679025215,7.37780448255811));
#51386=CARTESIAN_POINT('Origin',(5.89878270283593,6.95921850207614,7.74135566505664));
#51387=CARTESIAN_POINT('Ctrl Pts',(5.71061633139555,6.68825430759423,8.1203063081284));
#51388=CARTESIAN_POINT('Ctrl Pts',(5.71571542223483,6.68567794625997,8.11996801621166));
#51389=CARTESIAN_POINT('Ctrl Pts',(5.76276700635191,6.66117775605966,8.11739155262433));
#51390=CARTESIAN_POINT('Ctrl Pts',(5.84736859742446,6.60432471294745,8.12235110026491));
#51391=CARTESIAN_POINT('Ctrl Pts',(5.94575166176578,6.50451738948382,8.15321624698963));
#51392=CARTESIAN_POINT('Ctrl Pts',(6.01456588634735,6.3959192625854,8.20362766067628));
#51393=CARTESIAN_POINT('Ctrl Pts',(6.04741736776337,6.29826329603432,8.26181413939222));
#51394=CARTESIAN_POINT('Ctrl Pts',(6.05207362756165,6.24151474090948,8.30216609769673));
#51395=CARTESIAN_POINT('Ctrl Pts',(6.05138819518176,6.21914710908527,8.31924280036705));
#51396=CARTESIAN_POINT('Ctrl Pts',(5.59392208653217,6.47899731163308,7.91253200724143));
#51397=CARTESIAN_POINT('Ctrl Pts',(5.59866955743605,6.47661703590363,7.91219372773975));
#51398=CARTESIAN_POINT('Ctrl Pts',(5.6424838618781,6.45398236827702,7.90956757196331));
#51399=CARTESIAN_POINT('Ctrl Pts',(5.72137642495094,6.40146868496194,7.91357340076122));
#51400=CARTESIAN_POINT('Ctrl Pts',(5.81312989580529,6.30944394505649,7.94114488602853));
#51401=CARTESIAN_POINT('Ctrl Pts',(5.87715279420531,6.20973494694733,7.98666537269705));
#51402=CARTESIAN_POINT('Ctrl Pts',(5.90753939606212,6.12074388781985,8.03925603483806));
#51403=CARTESIAN_POINT('Ctrl Pts',(5.91179865681948,6.06956203278856,8.07558361900822));
#51404=CARTESIAN_POINT('Ctrl Pts',(5.91117126135558,6.04949611706124,8.09091432397107));
#51405=CARTESIAN_POINT('Ctrl Pts',(5.57597263223173,6.48127925322056,7.59591028107758));
#51406=CARTESIAN_POINT('Ctrl Pts',(5.58273758482897,6.47792626708818,7.59545099347781));
#51407=CARTESIAN_POINT('Ctrl Pts',(5.64510830703547,6.44608460045405,7.5919303212076));
#51408=CARTESIAN_POINT('Ctrl Pts',(5.75644759897633,6.37296939409402,7.5981443156954));
#51409=CARTESIAN_POINT('Ctrl Pts',(5.88585584667335,6.24539458879271,7.63765045596241));
#51410=CARTESIAN_POINT('Ctrl Pts',(5.97748415205553,6.10548886830425,7.70282854503511));
#51411=CARTESIAN_POINT('Ctrl Pts',(6.02250848732848,5.976818340779,7.77966536946315));
#51412=CARTESIAN_POINT('Ctrl Pts',(6.02923395546078,5.89948703576177,7.834648132105));
#51413=CARTESIAN_POINT('Ctrl Pts',(6.02824683811861,5.868477692758,7.85831508294452));
#51414=CARTESIAN_POINT('Ctrl Pts',(5.66860840586943,6.69359454132171,7.37930452174859));
#51415=CARTESIAN_POINT('Ctrl Pts',(5.67842908309909,6.68874171019614,7.37868303011404));
#51416=CARTESIAN_POINT('Ctrl Pts',(5.76890893218883,6.64269404293812,7.37401309649988));
#51417=CARTESIAN_POINT('Ctrl Pts',(5.92944679261123,6.53762650096011,7.38414049452444));
#51418=CARTESIAN_POINT('Ctrl Pts',(6.11595471194353,6.3546200579059,7.44293675038479));
#51419=CARTESIAN_POINT('Ctrl Pts',(6.24937488282923,6.15194807007878,7.53935356989418));
#51420=CARTESIAN_POINT('Ctrl Pts',(6.31648358865281,5.96142879087898,7.65428422951676));
#51421=CARTESIAN_POINT('Ctrl Pts',(6.32691160405283,5.84348172036974,7.73829558507271));
#51422=CARTESIAN_POINT('Ctrl Pts',(6.3253843013646,5.79550278490975,7.77488190927595));
#51423=CARTESIAN_POINT('',(5.99999999999929,6.09544950676928,8.13560044756764));
#51424=CARTESIAN_POINT('Ctrl Pts',(5.99998827407956,6.09544950560664,8.13560044835052));
#51425=CARTESIAN_POINT('Ctrl Pts',(5.99998537178181,6.0985235188595,8.11167900213626));
#51426=CARTESIAN_POINT('Ctrl Pts',(5.99998616180659,6.1020672978436,8.08790876283193));
#51427=CARTESIAN_POINT('Ctrl Pts',(5.99999964263501,6.10614414461004,8.06438762436252));
#51428=CARTESIAN_POINT('Ctrl Pts',(6.00000808539942,6.10869738953676,8.04965682114416));
#51429=CARTESIAN_POINT('Ctrl Pts',(6.00002053204976,6.11145911940312,8.03502411123104));
#51430=CARTESIAN_POINT('Ctrl Pts',(6.00003309722689,6.11443703572943,8.02051631282948));
#51431=CARTESIAN_POINT('Ctrl Pts',(6.00005418885645,6.11943570048125,7.99616384199079));
#51432=CARTESIAN_POINT('Ctrl Pts',(6.00007686014713,6.12504607350498,7.97216315652948));
#51433=CARTESIAN_POINT('Ctrl Pts',(6.00009746231146,6.13126411378436,7.94863439925196));
#51434=CARTESIAN_POINT('Ctrl Pts',(6.00010841241073,6.13456901695795,7.93612880888857));
#51435=CARTESIAN_POINT('Ctrl Pts',(6.00011838637384,6.13804472091411,7.92375664857546));
#51436=CARTESIAN_POINT('Ctrl Pts',(6.00012560696237,6.14168481188013,7.91153595676546));
#51437=CARTESIAN_POINT('Ctrl Pts',(6.00013953874254,6.14870819328121,7.88795671647509));
#51438=CARTESIAN_POINT('Ctrl Pts',(6.0001421475481,6.15634660115405,7.86494246365324));
#51439=CARTESIAN_POINT('Ctrl Pts',(6.00012604298399,6.16451476811207,7.84261416200171));
#51440=CARTESIAN_POINT('Ctrl Pts',(6.00011913996253,6.16801595146733,7.83304341271422));
#51441=CARTESIAN_POINT('Ctrl Pts',(6.00010897012775,6.17161385499292,7.82359849664904));
#51442=CARTESIAN_POINT('Ctrl Pts',(6.00009598241838,6.17529925506742,7.81428784213583));
#51443=CARTESIAN_POINT('Ctrl Pts',(6.00009379118139,6.1759210417689,7.81271698387312));
#51444=CARTESIAN_POINT('Ctrl Pts',(6.00009152155428,6.17654531603784,7.8111499455311));
#51445=CARTESIAN_POINT('Ctrl Pts',(6.00008918129249,6.17717203250874,7.80958676236975));
#51446=CARTESIAN_POINT('Ctrl Pts',(6.00007044381521,6.18218988379821,7.79707102198934));
#51447=CARTESIAN_POINT('Ctrl Pts',(6.00005227277352,6.18742746363513,7.78463200772731));
#51448=CARTESIAN_POINT('Ctrl Pts',(6.00003127527203,6.19279782868115,7.77248562475542));
#51449=CARTESIAN_POINT('Ctrl Pts',(6.00001008664516,6.19821707635837,7.76022868185808));
#51450=CARTESIAN_POINT('Ctrl Pts',(5.99998556854563,6.20377138573136,7.74827022814555));
#51451=CARTESIAN_POINT('Ctrl Pts',(5.99996740877935,6.20932028803311,7.73682129885285));
#51452=CARTESIAN_POINT('Ctrl Pts',(5.99995691476844,6.21252684038545,7.73020528920647));
#51453=CARTESIAN_POINT('Ctrl Pts',(5.99994883619827,6.21573063522951,7.72375917760543));
#51454=CARTESIAN_POINT('Ctrl Pts',(5.99994773775714,6.21889758122576,7.71752118994764));
#51455=CARTESIAN_POINT('Ctrl Pts',(5.99994375377365,6.2303839142034,7.6948963635589));
#51456=CARTESIAN_POINT('Ctrl Pts',(5.99996351071227,6.24267211096661,7.67263884761238));
#51457=CARTESIAN_POINT('Ctrl Pts',(5.99998940177669,6.2557542052183,7.65091230797903));
#51458=CARTESIAN_POINT('Ctrl Pts',(6.00001515384743,6.26876606950817,7.62930240517918));
#51459=CARTESIAN_POINT('Ctrl Pts',(6.00004625470305,6.28256328239365,7.60821873855136));
#51460=CARTESIAN_POINT('Ctrl Pts',(6.00006686787884,6.29708667041071,7.58781913651103));
#51461=CARTESIAN_POINT('Ctrl Pts',(6.0000726178758,6.3011379353728,7.58212871545434));
#51462=CARTESIAN_POINT('Ctrl Pts',(6.00007759523361,6.30524540300111,7.57649145646077));
#51463=CARTESIAN_POINT('Ctrl Pts',(6.00008158486497,6.30940710200007,7.57091058889349));
#51464=CARTESIAN_POINT('Ctrl Pts',(6.00009591088445,6.32435098414694,7.55087073804807));
#51465=CARTESIAN_POINT('Ctrl Pts',(6.00009642673619,6.33999756707795,7.53155982479057));
#51466=CARTESIAN_POINT('Ctrl Pts',(6.00008390520131,6.35622965439619,7.51311008864557));
#51467=CARTESIAN_POINT('Ctrl Pts',(6.0000712262293,6.37266583277199,7.49442837825795));
#51468=CARTESIAN_POINT('Ctrl Pts',(6.000044816293,6.38970156778594,7.47663037459175));
#51469=CARTESIAN_POINT('Ctrl Pts',(6.00002344711442,6.40717531708069,7.45982218522411));
#51470=CARTESIAN_POINT('Ctrl Pts',(6.00001019823316,6.41800903391686,7.44940111524846));
#51471=CARTESIAN_POINT('Ctrl Pts',(5.99999928041887,6.42901037243094,7.43935984833557));
#51472=CARTESIAN_POINT('Ctrl Pts',(5.99999922550778,6.44013547507157,7.42971620739118));
#51473=CARTESIAN_POINT('Ctrl Pts',(5.73278343882478,6.65588366033016,8.10254996066954));
#51474=CARTESIAN_POINT('Ctrl Pts',(5.74652216226264,6.64290705362911,8.09796672996633));
#51475=CARTESIAN_POINT('Ctrl Pts',(5.75957819268944,6.6297391121596,8.09404270281397));
#51476=CARTESIAN_POINT('Ctrl Pts',(5.77191402195044,6.6165246743462,8.09067264558843));
#51477=CARTESIAN_POINT('Ctrl Pts',(5.78455326508681,6.60298521227193,8.08721969793848));
#51478=CARTESIAN_POINT('Ctrl Pts',(5.79643718469295,6.58939758209051,8.08434749272246));
#51479=CARTESIAN_POINT('Ctrl Pts',(5.80757705713372,6.57590082893888,8.08195774837986));
#51480=CARTESIAN_POINT('Ctrl Pts',(5.81921372581329,6.56180217157,8.07946143046495));
#51481=CARTESIAN_POINT('Ctrl Pts',(5.83003943422937,6.54780315409756,8.07749092628001));
#51482=CARTESIAN_POINT('Ctrl Pts',(5.84010967404772,6.53403521658879,8.07596191120139));
#51483=CARTESIAN_POINT('Ctrl Pts',(5.84591284550348,6.52610117495753,8.07508078653904));
#51484=CARTESIAN_POINT('Ctrl Pts',(5.85146583339613,6.5182433251846,8.07434684899726));
#51485=CARTESIAN_POINT('Ctrl Pts',(5.85678336455151,6.51048234910576,8.07374880498796));
#51486=CARTESIAN_POINT('Ctrl Pts',(5.8670115993516,6.49555416471101,8.07259847142729));
#51487=CARTESIAN_POINT('Ctrl Pts',(5.87634426622871,6.4809886970225,8.07192749106764));
#51488=CARTESIAN_POINT('Ctrl Pts',(5.88485691334425,6.46691376275036,8.07161710097136));
#51489=CARTESIAN_POINT('Ctrl Pts',(5.88966062429399,6.458971237357,8.07144194695828));
#51490=CARTESIAN_POINT('Ctrl Pts',(5.89420384053122,6.4511843623423,8.07138221398306));
#51491=CARTESIAN_POINT('Ctrl Pts',(5.89850363154804,6.44357186666483,8.07142126578559));
#51492=CARTESIAN_POINT('Ctrl Pts',(5.90446335283279,6.43302057420861,8.07147539349966));
#51493=CARTESIAN_POINT('Ctrl Pts',(5.90995415386343,6.42280438722931,8.0717172162624));
#51494=CARTESIAN_POINT('Ctrl Pts',(5.9150194297642,6.41296495876872,8.07210178476554));
#51495=CARTESIAN_POINT('Ctrl Pts',(5.91755206771458,6.40804524453842,8.07229406901711));
#51496=CARTESIAN_POINT('Ctrl Pts',(5.91997825702204,6.40321969767778,8.07252206789));
#51497=CARTESIAN_POINT('Ctrl Pts',(5.92230356304916,6.39849258665512,8.0727806332584));
#51498=CARTESIAN_POINT('Ctrl Pts',(5.92346621606272,6.39612903114379,8.07290991594259));
#51499=CARTESIAN_POINT('Ctrl Pts',(5.92460364371983,6.39379008282668,8.0730468424592));
#51500=CARTESIAN_POINT('Ctrl Pts',(5.92571653121906,6.3914762444007,8.0731907941147));
#51501=CARTESIAN_POINT('Ctrl Pts',(5.92650181455179,6.38984353781373,8.0732923702721));
#51502=CARTESIAN_POINT('Ctrl Pts',(5.9269696212441,6.38886378412244,8.07335487663796));
#51503=CARTESIAN_POINT('Ctrl Pts',(5.92776753993371,6.3871818633714,8.07346749913357));
#51504=CARTESIAN_POINT('Ctrl Pts',(5.92810041531301,6.38648020038837,8.07351448293836));
#51505=CARTESIAN_POINT('Ctrl Pts',(5.92849041668746,6.38565619733019,8.0735703947824));
#51506=CARTESIAN_POINT('Ctrl Pts',(5.92898224825978,6.38461054370544,8.07364311834452));
#51507=CARTESIAN_POINT('Ctrl Pts',(5.93824263884224,6.36492258237076,8.0750123850361));
#51508=CARTESIAN_POINT('Ctrl Pts',(5.94647893757245,6.34554238942372,8.07701435392396));
#51509=CARTESIAN_POINT('Ctrl Pts',(5.95372901404908,6.32660267221935,8.07949390178515));
#51510=CARTESIAN_POINT('Ctrl Pts',(5.96117537732152,6.30715018574758,8.08204058031818));
#51511=CARTESIAN_POINT('Ctrl Pts',(5.96758228145031,6.28816272684888,8.08509044760169));
#51512=CARTESIAN_POINT('Ctrl Pts',(5.97303224009227,6.26975867528639,8.08850160394176));
#51513=CARTESIAN_POINT('Ctrl Pts',(5.9787505155944,6.2504485402737,8.09208070114504));
#51514=CARTESIAN_POINT('Ctrl Pts',(5.98341631050524,6.2317809266297,8.09605707728519));
#51515=CARTESIAN_POINT('Ctrl Pts',(5.9871551247652,6.21385976069274,8.10030389064878));
#51516=CARTESIAN_POINT('Ctrl Pts',(5.99100606181786,6.19540115934611,8.10467806112115));
#51517=CARTESIAN_POINT('Ctrl Pts',(5.99387471606403,6.17773434412722,8.1093391054874));
#51518=CARTESIAN_POINT('Ctrl Pts',(5.9959123780958,6.16093782306683,8.11419052900978));
#51519=CARTESIAN_POINT('Ctrl Pts',(5.99805099892841,6.14330909499754,8.11928232306151));
#51520=CARTESIAN_POINT('Ctrl Pts',(5.99927528159734,6.12663881069711,8.12458397046569));
#51521=CARTESIAN_POINT('Ctrl Pts',(5.99975824748392,6.11098214001741,8.13002891614501));
#51522=CARTESIAN_POINT('Ctrl Pts',(5.99992154067033,6.10568854120467,8.13186987956394));
#51523=CARTESIAN_POINT('Ctrl Pts',(6.0000000065821,6.10051054258625,8.13372757636712));
#51524=CARTESIAN_POINT('Ctrl Pts',(5.99999999999929,6.09544950676928,8.13560044756764));
#51525=CARTESIAN_POINT('Ctrl Pts',(5.99968415523845,6.00656139605184,8.08769837817367));
#51526=CARTESIAN_POINT('Ctrl Pts',(5.99968415523845,6.35078816638231,8.34790825714588));
#51527=CARTESIAN_POINT('Ctrl Pts',(5.99968415523845,7.06928852668172,8.96885076597258));
#51528=CARTESIAN_POINT('Ctrl Pts',(5.99968415523845,8.03053011388277,10.075949619057));
#51529=CARTESIAN_POINT('Ctrl Pts',(5.99968415523845,8.85193945551654,11.3901955327746));
#51530=CARTESIAN_POINT('Ctrl Pts',(5.99968415523845,9.45913036146108,12.8152579698838));
#51531=CARTESIAN_POINT('Ctrl Pts',(5.99968415523845,9.83821289603149,14.3183256849662));
#51532=CARTESIAN_POINT('Ctrl Pts',(5.99968415523845,9.96603145443171,15.7255914318733));
#51533=CARTESIAN_POINT('Ctrl Pts',(5.99968415523845,9.92625398667906,16.6207279726114));
#51534=CARTESIAN_POINT('Ctrl Pts',(5.99968415523845,9.8878432222398,16.9970837242003));
#51535=CARTESIAN_POINT('Ctrl Pts',(6.00710925937989,6.11916148493871,7.93873236047488));
#51536=CARTESIAN_POINT('Ctrl Pts',(6.00710925937989,6.46990577187445,8.20386673730895));
#51537=CARTESIAN_POINT('Ctrl Pts',(6.00710925937989,7.20187340659612,8.83644658604556));
#51538=CARTESIAN_POINT('Ctrl Pts',(6.00710925937989,8.18131791270368,9.96451835081638));
#51539=CARTESIAN_POINT('Ctrl Pts',(6.00710925937989,9.0181474918832,11.3034312647952));
#51540=CARTESIAN_POINT('Ctrl Pts',(6.00710925937989,9.63683604404024,12.7554734616408));
#51541=CARTESIAN_POINT('Ctrl Pts',(6.00710925937989,10.0230315315726,14.2867682665207));
#51542=CARTESIAN_POINT('Ctrl Pts',(6.00710925937989,10.1532734887705,15.7206563920744));
#51543=CARTESIAN_POINT('Ctrl Pts',(6.00710925937989,10.1127513948415,16.6325797415481));
#51544=CARTESIAN_POINT('Ctrl Pts',(6.00710925937989,10.0736127087543,17.0160475747281));
#51545=CARTESIAN_POINT('Ctrl Pts',(5.89995655749497,6.21158111094138,7.81646439622245));
#51546=CARTESIAN_POINT('Ctrl Pts',(5.89995655749497,6.56767482924154,8.08564069038753));
#51547=CARTESIAN_POINT('Ctrl Pts',(5.89995655749497,7.31069610057991,8.72777220655928));
#51548=CARTESIAN_POINT('Ctrl Pts',(5.89995655749497,8.30508115401766,9.87305806657078));
#51549=CARTESIAN_POINT('Ctrl Pts',(5.89995655749497,9.15456731811607,11.2322171007898));
#51550=CARTESIAN_POINT('Ctrl Pts',(5.89995655749497,9.78269288025933,12.7064036789539));
#51551=CARTESIAN_POINT('Ctrl Pts',(5.89995655749497,10.1747265199527,14.2608666456689));
#51552=CARTESIAN_POINT('Ctrl Pts',(5.89995655749497,10.3069575484958,15.7166058221585));
#51553=CARTESIAN_POINT('Ctrl Pts',(5.89995655749497,10.2658242821102,16.6423074075148));
#51554=CARTESIAN_POINT('Ctrl Pts',(5.89995655749497,10.226088134276,17.0316126776586));
#51555=CARTESIAN_POINT('Ctrl Pts',(5.72168991350276,6.2459107561173,7.77104746466054));
#51556=CARTESIAN_POINT('Ctrl Pts',(5.72168991350276,6.60399154240885,8.04172514542314));
#51557=CARTESIAN_POINT('Ctrl Pts',(5.72168991350276,7.35111873193133,8.68740466723007));
#51558=CARTESIAN_POINT('Ctrl Pts',(5.72168991350276,8.35105351231554,9.83908477278564));
#51559=CARTESIAN_POINT('Ctrl Pts',(5.72168991350276,9.20524101624623,11.2057643105373));
#51560=CARTESIAN_POINT('Ctrl Pts',(5.72168991350276,9.83687199405033,12.6881765090173));
#51561=CARTESIAN_POINT('Ctrl Pts',(5.72168991350276,10.2310742390599,14.2512453834785));
#51562=CARTESIAN_POINT('Ctrl Pts',(5.72168991350276,10.3640441162288,15.7151012215239));
#51563=CARTESIAN_POINT('Ctrl Pts',(5.72168991350276,10.3226838273516,16.6459207885187));
#51564=CARTESIAN_POINT('Ctrl Pts',(5.72168991350276,10.2827257499292,17.0373943983161));
#51565=CARTESIAN_POINT('Ctrl Pts',(5.99999999999929,6.09544950676928,8.13560044756764));
#51566=CARTESIAN_POINT('Ctrl Pts',(5.9999999999993,6.21599272915026,8.22864748093463));
#51567=CARTESIAN_POINT('Ctrl Pts',(6.00000000006295,6.33400221607625,8.32414772917356));
#51568=CARTESIAN_POINT('Ctrl Pts',(5.99999999822618,6.44958311156655,8.422124980624));
#51569=CARTESIAN_POINT('Ctrl Pts',(5.99999999638109,6.56568781639286,8.52054626219558));
#51570=CARTESIAN_POINT('Ctrl Pts',(5.99999999247689,6.67934219993644,8.62146736838768));
#51571=CARTESIAN_POINT('Ctrl Pts',(5.99999999188347,6.79061972240305,8.72495313863626));
#51572=CARTESIAN_POINT('Ctrl Pts',(5.99999999151144,6.86038184500564,8.78983045466269));
#51573=CARTESIAN_POINT('Ctrl Pts',(5.99999999284036,6.92920911788454,8.8557165489303));
#51574=CARTESIAN_POINT('Ctrl Pts',(5.99999999533528,6.99711214007891,8.92263466848373));
#51575=CARTESIAN_POINT('Ctrl Pts',(5.99999999728228,7.05010275404376,8.97485667754776));
#51576=CARTESIAN_POINT('Ctrl Pts',(5.99999999999971,7.10253038140868,9.02770730633247));
#51577=CARTESIAN_POINT('Ctrl Pts',(5.99999999999971,7.15440146857915,9.08120097285816));
#51578=CARTESIAN_POINT('Ctrl Pts',(5.99999999999971,7.28007178588764,9.21080238306546));
#51579=CARTESIAN_POINT('Ctrl Pts',(5.999999984904,7.40251839100925,9.34411442180928));
#51580=CARTESIAN_POINT('Ctrl Pts',(5.99999998011157,7.5213665288948,9.48080996079188));
#51581=CARTESIAN_POINT('Ctrl Pts',(5.99999997532264,7.64012751541815,9.61740526090964));
#51582=CARTESIAN_POINT('Ctrl Pts',(5.99999998034514,7.75529499347647,9.75737878109644));
#51583=CARTESIAN_POINT('Ctrl Pts',(5.99999998874861,7.86653171168378,9.90036730327227));
#51584=CARTESIAN_POINT('Ctrl Pts',(5.99999999244904,7.915514355194,9.96333172653706));
#51585=CARTESIAN_POINT('Ctrl Pts',(5.99999999643384,7.96373531284376,10.0268803217595));
#51586=CARTESIAN_POINT('Ctrl Pts',(5.99999999855295,8.01116828547801,10.0909800599343));
#51587=CARTESIAN_POINT('Ctrl Pts',(5.99999999944824,8.03120793721771,10.118061146324));
#51588=CARTESIAN_POINT('Ctrl Pts',(5.9999999999997,8.05110695913799,10.1452405932687));
#51589=CARTESIAN_POINT('Ctrl Pts',(5.9999999999997,8.07086366361946,10.1725155424444));
#51590=CARTESIAN_POINT('Ctrl Pts',(5.9999999999997,8.19463793080481,10.3433910470058));
#51591=CARTESIAN_POINT('Ctrl Pts',(5.99999998499452,8.31277452188091,10.5180623042338));
#51592=CARTESIAN_POINT('Ctrl Pts',(5.99999998425411,8.42519108889713,10.6962951891408));
#51593=CARTESIAN_POINT('Ctrl Pts',(5.9999999835127,8.53775753234144,10.8747656983488));
#51594=CARTESIAN_POINT('Ctrl Pts',(5.99999999342451,8.64458901980545,11.0568078073897));
#51595=CARTESIAN_POINT('Ctrl Pts',(5.99999999807136,8.74556121729957,11.2422176425727));
#51596=CARTESIAN_POINT('Ctrl Pts',(5.99999999924405,8.77104273958086,11.2890079963893));
#51597=CARTESIAN_POINT('Ctrl Pts',(5.99999999999971,8.79615088361354,11.3360129638309));
#51598=CARTESIAN_POINT('Ctrl Pts',(5.99999999999971,8.82088319339553,11.3832295268562));
#51599=CARTESIAN_POINT('Ctrl Pts',(5.9999999999997,8.82409824626035,11.3893673986344));
#51600=CARTESIAN_POINT('Ctrl Pts',(5.99999999998697,8.82730698839302,11.395508823316));
#51601=CARTESIAN_POINT('Ctrl Pts',(5.99999999996269,8.83050940751732,11.4016537827019));
#51602=CARTESIAN_POINT('Ctrl Pts',(5.99999999919991,8.93112302668215,11.5947161456975));
#51603=CARTESIAN_POINT('Ctrl Pts',(5.99999999014648,9.02549152491428,11.7912698092488));
#51604=CARTESIAN_POINT('Ctrl Pts',(5.99999998974637,9.11332588235521,11.9907230388185));
#51605=CARTESIAN_POINT('Ctrl Pts',(5.99999998934601,9.20121618416255,12.1903033061998));
#51606=CARTESIAN_POINT('Ctrl Pts',(5.99999999678082,9.28256378678173,12.3927863257178));
#51607=CARTESIAN_POINT('Ctrl Pts',(5.99999999936896,9.3571261646783,12.5975570160648));
#51608=CARTESIAN_POINT('Ctrl Pts',(5.99999999976094,9.36841888658775,12.6285702230806));
#51609=CARTESIAN_POINT('Ctrl Pts',(5.9999999999997,9.37955605981923,12.6596358719235));
#51610=CARTESIAN_POINT('Ctrl Pts',(5.9999999999997,9.39053694094342,12.690751792812));
#51611=CARTESIAN_POINT('Ctrl Pts',(5.9999999999997,9.40603018940343,12.7346541616597));
#51612=CARTESIAN_POINT('Ctrl Pts',(5.99999999951884,9.42121086917364,12.7786568707967));
#51613=CARTESIAN_POINT('Ctrl Pts',(5.99999999869869,9.43607805733177,12.8227576339477));
#51614=CARTESIAN_POINT('Ctrl Pts',(5.99999999492022,9.50457105013169,13.0259294254691));
#51615=CARTESIAN_POINT('Ctrl Pts',(5.99999998426479,9.56641442502825,13.2311813385896));
#51616=CARTESIAN_POINT('Ctrl Pts',(5.99999998403914,9.62153670788177,13.4382622973276));
#51617=CARTESIAN_POINT('Ctrl Pts',(5.99999998381348,9.6766589907353,13.6453432560655));
#51618=CARTESIAN_POINT('Ctrl Pts',(5.99999999999971,9.72506028807675,13.8542538365966));
#51619=CARTESIAN_POINT('Ctrl Pts',(5.99999999999971,9.76661736553527,14.0647507043716));
#51620=CARTESIAN_POINT('Ctrl Pts',(5.99999999999971,9.78347351328543,14.1501312585673));
#51621=CARTESIAN_POINT('Ctrl Pts',(5.99999999594492,9.79921712968305,14.235772411136));
#51622=CARTESIAN_POINT('Ctrl Pts',(5.99999999152506,9.81383325134206,14.3216199403523));
#51623=CARTESIAN_POINT('Ctrl Pts',(5.99999998224973,9.84450604590268,14.5017760507502));
#51624=CARTESIAN_POINT('Ctrl Pts',(5.9999999734632,9.87021006131464,14.682841403213));
#51625=CARTESIAN_POINT('Ctrl Pts',(5.99999997653297,9.89090683235236,14.8643171280013));
#51626=CARTESIAN_POINT('Ctrl Pts',(5.99999997960657,9.91162946133668,15.0460195833067));
#51627=CARTESIAN_POINT('Ctrl Pts',(5.99999999486873,9.92733230893222,15.2281329800598));
#51628=CARTESIAN_POINT('Ctrl Pts',(5.9999999991423,9.93802883787374,15.4101537132592));
#51629=CARTESIAN_POINT('Ctrl Pts',(5.99999999968371,9.93938395859166,15.433213536497));
#51630=CARTESIAN_POINT('Ctrl Pts',(5.9999999999997,9.94065879737618,15.4562718740799));
#51631=CARTESIAN_POINT('Ctrl Pts',(5.9999999999997,9.94185344127986,15.479327704528));
#51632=CARTESIAN_POINT('Ctrl Pts',(5.9999999999997,9.94848717375989,15.6073543163301));
#51633=CARTESIAN_POINT('Ctrl Pts',(5.99999999304439,9.95260845370109,15.7352949668062));
#51634=CARTESIAN_POINT('Ctrl Pts',(5.99999999143195,9.95424492247683,15.8632214076251));
#51635=CARTESIAN_POINT('Ctrl Pts',(5.99999998950812,9.95619741266735,16.0158519524361));
#51636=CARTESIAN_POINT('Ctrl Pts',(5.99999999273625,9.95461404479101,16.1684624668109));
#51637=CARTESIAN_POINT('Ctrl Pts',(5.99999999547189,9.94950734202748,16.3211471683246));
#51638=CARTESIAN_POINT('Ctrl Pts',(5.99999999819524,9.94442356206008,16.4731465038703));
#51639=CARTESIAN_POINT('Ctrl Pts',(5.99999999961476,9.93584800483817,16.6252198213967));
#51640=CARTESIAN_POINT('Ctrl Pts',(5.99999999985072,9.92374152693551,16.7774586800326));
#51641=CARTESIAN_POINT('Ctrl Pts',(5.99999999991369,9.92051092369794,16.8180834887958));
#51642=CARTESIAN_POINT('Ctrl Pts',(5.99999999993325,9.91702860387934,16.8587200565166));
#51643=CARTESIAN_POINT('Ctrl Pts',(5.99999999993294,9.9132931986081,16.8993700414499));
#51644=CARTESIAN_POINT('Origin',(7.4,0.,0.));
#51645=CARTESIAN_POINT('',(7.4,5.99999999991914,-10.3923048454599));
#51646=CARTESIAN_POINT('Origin',(7.4,6.74999999990903,-11.6913429511424));
#51647=CARTESIAN_POINT('Origin',(7.4,6.74999999990903,-11.6913429511424));
#51648=CARTESIAN_POINT('',(6.,5.99999999991914,-10.3923048454599));
#51649=CARTESIAN_POINT('',(7.4,5.99999999991914,-10.3923048454599));
#51650=CARTESIAN_POINT('Origin',(6.,6.74999999990903,-11.6913429511424));
#51651=CARTESIAN_POINT('Origin',(7.4,-6.62945397692566E-15,1.14825511146811E-14));
#51652=CARTESIAN_POINT('',(7.4,6.00000000008095,10.3923048453666));
#51653=CARTESIAN_POINT('Origin',(7.4,6.75000000009103,11.6913429510374));
#51654=CARTESIAN_POINT('Origin',(7.4,6.75000000009103,11.6913429510374));
#51655=CARTESIAN_POINT('',(6.,6.00000000008095,10.3923048453666));
#51656=CARTESIAN_POINT('',(7.4,6.00000000008095,10.3923048453666));
#51657=CARTESIAN_POINT('Origin',(6.,6.75000000009103,11.6913429510374));
#51658=CARTESIAN_POINT('Origin',(6.,0.,0.));
#51659=CARTESIAN_POINT('',(0.,0.,0.));
#51660=CARTESIAN_POINT('Origin',(23.,0.,19.3));
#51661=CARTESIAN_POINT('',(25.5,-3.06161699786838E-16,19.3));
#51662=CARTESIAN_POINT('Origin',(23.,0.,19.3));
#51663=CARTESIAN_POINT('',(23.,-1.3856406461,19.3));
#51664=CARTESIAN_POINT('',(21.8,-0.692820323,19.3));
#51665=CARTESIAN_POINT('',(22.3999999999746,-1.03923048453533,19.3));
#51666=CARTESIAN_POINT('',(21.8,0.692820323,19.3));
#51667=CARTESIAN_POINT('',(21.8,0.17320508075,19.3));
#51668=CARTESIAN_POINT('',(23.,1.3856406461,19.3));
#51669=CARTESIAN_POINT('',(22.3999999999746,1.03923048453533,19.3));
#51670=CARTESIAN_POINT('',(24.2,0.692820323,19.3));
#51671=CARTESIAN_POINT('',(23.6000000000254,1.03923048453533,19.3));
#51672=CARTESIAN_POINT('',(24.2,-0.692820323,19.3));
#51673=CARTESIAN_POINT('',(24.2,0.,19.3));
#51674=CARTESIAN_POINT('',(23.6000000000254,-1.03923048453533,19.3));
#51675=CARTESIAN_POINT('Origin',(23.,0.,9.3));
#51676=CARTESIAN_POINT('',(25.5,-3.06161699786838E-16,9.3));
#51677=CARTESIAN_POINT('Origin',(23.,0.,9.3));
#51678=CARTESIAN_POINT('Origin',(23.,0.,14.3));
#51679=CARTESIAN_POINT('',(25.5,3.06161699786838E-16,14.3));
#51680=CARTESIAN_POINT('Origin',(23.,3.11198878113149E-17,16.8));
#51681=CARTESIAN_POINT('',(24.2,-0.692820323,16.8));
#51682=CARTESIAN_POINT('',(23.,-1.3856406461,16.8));
#51683=CARTESIAN_POINT('',(24.2,-0.692820323,16.8));
#51684=CARTESIAN_POINT('',(24.2,0.692820323,16.8));
#51685=CARTESIAN_POINT('',(24.2,0.692820323,16.8));
#51686=CARTESIAN_POINT('',(23.,1.3856406461,16.8));
#51687=CARTESIAN_POINT('',(23.,1.3856406461,16.8));
#51688=CARTESIAN_POINT('',(21.8,0.692820323,16.8));
#51689=CARTESIAN_POINT('',(21.8,0.692820323,16.8));
#51690=CARTESIAN_POINT('',(21.8,-0.692820323,16.8));
#51691=CARTESIAN_POINT('',(21.8,-0.692820323,16.8));
#51692=CARTESIAN_POINT('',(23.,-1.3856406461,16.8));
#51693=CARTESIAN_POINT('Origin',(23.6,-1.03923048455,16.8));
#51694=CARTESIAN_POINT('',(24.2,-0.692820323,16.8));
#51695=CARTESIAN_POINT('',(23.,-1.3856406461,16.8));
#51696=CARTESIAN_POINT('Origin',(24.2,0.,16.8));
#51697=CARTESIAN_POINT('',(24.2,0.692820323,16.8));
#51698=CARTESIAN_POINT('Origin',(23.6,1.03923048455,16.8));
#51699=CARTESIAN_POINT('',(23.,1.3856406461,16.8));
#51700=CARTESIAN_POINT('Origin',(22.4,1.03923048455,16.8));
#51701=CARTESIAN_POINT('',(21.8,0.692820323,16.8));
#51702=CARTESIAN_POINT('Origin',(21.8,0.3464101615,16.8));
#51703=CARTESIAN_POINT('',(21.8,-0.692820323,16.8));
#51704=CARTESIAN_POINT('Origin',(22.4,-1.03923048455,16.8));
#51705=CARTESIAN_POINT('',(0.,0.,0.));
#51706=CARTESIAN_POINT('Origin',(-6.,0.,-10.));
#51707=CARTESIAN_POINT('',(-6.,-11.5470739757602,3.26574380475891));
#51708=CARTESIAN_POINT('',(-6.,-19.921468401738,1.77062043322529));
#51709=CARTESIAN_POINT('Origin',(-6.,-13.8564064606,-8.));
#51710=CARTESIAN_POINT('',(-6.,-11.4941364764755,16.3671875));
#51711=CARTESIAN_POINT('Origin',(-6.,0.,0.));
#51712=CARTESIAN_POINT('',(-6.,-8.60175408505985,8.3671875));
#51713=CARTESIAN_POINT('Origin',(-6.,0.,16.));
#51714=CARTESIAN_POINT('Origin',(-6.,0.,0.));
#51715=CARTESIAN_POINT('Origin',(33.,0.,-9.5));
#51716=CARTESIAN_POINT('',(33.,2.32682891837997E-15,19.));
#51717=CARTESIAN_POINT('Origin',(33.,0.,0.));
#51718=CARTESIAN_POINT('',(33.,2.5,9.3));
#51719=CARTESIAN_POINT('',(33.,2.5,6.53834841531101));
#51720=CARTESIAN_POINT('',(33.,2.5,-2.425));
#51721=CARTESIAN_POINT('',(33.,-2.5,6.53834841531101));
#51722=CARTESIAN_POINT('Origin',(33.,0.,0.));
#51723=CARTESIAN_POINT('',(33.,-2.5,9.3));
#51724=CARTESIAN_POINT('',(33.,-2.5,-2.425));
#51725=CARTESIAN_POINT('',(33.,0.,9.3));
#51726=CARTESIAN_POINT('Origin',(32.5,0.,0.));
#51727=CARTESIAN_POINT('',(32.,2.44929359829471E-15,20.));
#51728=CARTESIAN_POINT('Origin',(32.,0.,0.));
#51729=CARTESIAN_POINT('',(32.5,2.38806125833734E-15,19.5));
#51730=CARTESIAN_POINT('Origin',(13.,0.,0.));
#51731=CARTESIAN_POINT('',(3.7202200813,-0.2994444445,-19.9977581999748));
#51732=CARTESIAN_POINT('',(4.3435534146,-0.2994444445,-19.9977581999748));
#51733=CARTESIAN_POINT('',(4.03188674795,-0.2994444445,-19.9977581999748));
#51734=CARTESIAN_POINT('',(4.3435534146,-1.1061111111,-19.969389530226));
#51735=CARTESIAN_POINT('Ctrl Pts',(4.3435534146,-0.2994444445,-19.9977581999748));
#51736=CARTESIAN_POINT('Ctrl Pts',(4.39419529583398,-0.2994444445,-19.9977581999748));
#51737=CARTESIAN_POINT('Ctrl Pts',(4.44821240138141,-0.309565031449933,
-19.9976146851541));
#51738=CARTESIAN_POINT('Ctrl Pts',(4.54758041279513,-0.350722737591021,
-19.9969351943239));
#51739=CARTESIAN_POINT('Ctrl Pts',(4.59293124895252,-0.381759842781414,
-19.9963882206146));
#51740=CARTESIAN_POINT('Ctrl Pts',(4.66456114163788,-0.453382333903515,
-19.994892548385));
#51741=CARTESIAN_POINT('Ctrl Pts',(4.69560697302298,-0.498746314496724,
-19.993842130762));
#51742=CARTESIAN_POINT('Ctrl Pts',(4.73676959169473,-0.5981279615852,-19.9911158762495));
#51743=CARTESIAN_POINT('Ctrl Pts',(4.7468867479,-0.652145173345914,-19.9894290439444));
#51744=CARTESIAN_POINT('Ctrl Pts',(4.7468867479,-0.753438288963382,-19.9858675169476));
#51745=CARTESIAN_POINT('Ctrl Pts',(4.73675961734101,-0.80746838265751,-19.9837551246746));
#51746=CARTESIAN_POINT('Ctrl Pts',(4.69558023913546,-0.906857064706403,
-19.9794915935354));
#51747=CARTESIAN_POINT('Ctrl Pts',(4.66452814741898,-0.952216188266304,
-19.9773514320566));
#51748=CARTESIAN_POINT('Ctrl Pts',(4.59290252845076,-1.02381445280548,-19.9738100392531));
#51749=CARTESIAN_POINT('Ctrl Pts',(4.54756443095206,-1.05484068319396,-19.9721740344373));
#51750=CARTESIAN_POINT('Ctrl Pts',(4.44821243395584,-1.09598926486806,-19.9699582388217));
#51751=CARTESIAN_POINT('Ctrl Pts',(4.39419807843,-1.1061111111,-19.969389530226));
#51752=CARTESIAN_POINT('Ctrl Pts',(4.3435534146,-1.1061111111,-19.969389530226));
#51753=CARTESIAN_POINT('',(3.7202200813,-1.1061111111,-19.969389530226));
#51754=CARTESIAN_POINT('',(4.03188674795,-1.1061111111,-19.969389530226));
#51755=CARTESIAN_POINT('Origin',(3.7202200813,0.,0.));
#51756=CARTESIAN_POINT('Origin',(-6.,0.,-10.));
#51757=CARTESIAN_POINT('',(-6.,8.60175408505985,8.3671875));
#51758=CARTESIAN_POINT('',(-6.,11.4941364764755,16.3671875));
#51759=CARTESIAN_POINT('Origin',(-6.,0.,16.));
#51760=CARTESIAN_POINT('',(-6.,19.921468401738,1.77062043322529));
#51761=CARTESIAN_POINT('Origin',(-6.,0.,0.));
#51762=CARTESIAN_POINT('',(-6.,11.5470739757602,3.26574380475891));
#51763=CARTESIAN_POINT('Origin',(-6.,13.8564064606,-8.));
#51764=CARTESIAN_POINT('Origin',(-6.,0.,0.));
#51765=CARTESIAN_POINT('Origin',(-6.,0.,-10.));
#51766=CARTESIAN_POINT('',(-6.,-8.42733192529161,-18.1378079331809));
#51767=CARTESIAN_POINT('',(-6.,-2.94531989074286,-11.632931304757));
#51768=CARTESIAN_POINT('Origin',(-6.,-13.8564064606,-8.));
#51769=CARTESIAN_POINT('',(-6.,2.94531989074286,-11.632931304757));
#51770=CARTESIAN_POINT('Origin',(-6.,0.,0.));
#51771=CARTESIAN_POINT('',(-6.,8.42733192529161,-18.1378079331809));
#51772=CARTESIAN_POINT('Origin',(-6.,13.8564064606,-8.));
#51773=CARTESIAN_POINT('Origin',(-6.,0.,0.));
#51774=CARTESIAN_POINT('Origin',(1.,-13.8564064606,-8.));
#51775=CARTESIAN_POINT('',(8.,-11.5470739757602,3.26574380475891));
#51776=CARTESIAN_POINT('',(8.,-19.921468401738,1.77062043322529));
#51777=CARTESIAN_POINT('Origin',(8.,-13.8564064606,-8.));
#51778=CARTESIAN_POINT('',(1.,-19.921468401738,1.77062043322529));
#51779=CARTESIAN_POINT('',(1.,-11.5470739757602,3.26574380475891));
#51780=CARTESIAN_POINT('Origin',(1.,0.,0.));
#51781=CARTESIAN_POINT('',(8.,-2.94531989074286,-11.632931304757));
#51782=CARTESIAN_POINT('',(1.,-2.94531989074286,-11.632931304757));
#51783=CARTESIAN_POINT('',(8.,2.94531989074286,-11.632931304757));
#51784=CARTESIAN_POINT('Origin',(8.,0.,0.));
#51785=CARTESIAN_POINT('',(1.,2.94531989074286,-11.632931304757));
#51786=CARTESIAN_POINT('Origin',(1.,0.,0.));
#51787=CARTESIAN_POINT('',(8.,11.5470739757602,3.26574380475891));
#51788=CARTESIAN_POINT('',(1.,11.5470739757602,3.26574380475891));
#51789=CARTESIAN_POINT('',(8.,8.60175408505985,8.3671875));
#51790=CARTESIAN_POINT('Origin',(8.,0.,0.));
#51791=CARTESIAN_POINT('',(1.,8.60175408505985,8.3671875));
#51792=CARTESIAN_POINT('Origin',(1.,0.,0.));
#51793=CARTESIAN_POINT('',(8.,-8.60175408505985,8.3671875));
#51794=CARTESIAN_POINT('',(1.,-8.60175408505985,8.3671875));
#51795=CARTESIAN_POINT('Origin',(8.,0.,0.));
#51796=CARTESIAN_POINT('Origin',(1.,13.8564064606,-8.));
#51797=CARTESIAN_POINT('',(8.,19.921468401738,1.77062043322529));
#51798=CARTESIAN_POINT('',(1.,19.921468401738,1.77062043322529));
#51799=CARTESIAN_POINT('Origin',(8.,13.8564064606,-8.));
#51800=CARTESIAN_POINT('Origin',(1.,13.8564064606,-8.));
#51801=CARTESIAN_POINT('',(8.,8.42733192529161,-18.1378079331809));
#51802=CARTESIAN_POINT('Origin',(8.,13.8564064606,-8.));
#51803=CARTESIAN_POINT('',(1.,8.42733192529161,-18.1378079331809));
#51804=CARTESIAN_POINT('Origin',(8.,13.8564064606,-8.));
#51805=CARTESIAN_POINT('',(8.,-8.42733192529161,-18.1378079331809));
#51806=CARTESIAN_POINT('Origin',(8.,0.,0.));
#51807=CARTESIAN_POINT('',(8.,-11.4941364764755,16.3671875));
#51808=CARTESIAN_POINT('Origin',(8.,0.,16.));
#51809=CARTESIAN_POINT('',(8.,-2.44929359829471E-15,20.));
#51810=CARTESIAN_POINT('Origin',(8.,0.,0.));
#51811=CARTESIAN_POINT('',(8.,11.4941364764755,16.3671875));
#51812=CARTESIAN_POINT('Origin',(8.,0.,0.));
#51813=CARTESIAN_POINT('Origin',(8.,0.,16.));
#51814=CARTESIAN_POINT('Origin',(8.,0.,0.));
#51815=CARTESIAN_POINT('Origin',(8.,-13.8564064606,-8.));
#51816=CARTESIAN_POINT('',(8.,2.5,6.53834841531101));
#51817=CARTESIAN_POINT('',(8.,2.5,9.3));
#51818=CARTESIAN_POINT('',(8.,2.5,-1.675));
#51819=CARTESIAN_POINT('',(8.,-2.5,9.3));
#51820=CARTESIAN_POINT('',(8.,6.9282032303,9.3));
#51821=CARTESIAN_POINT('',(8.,-2.5,6.53834841531101));
#51822=CARTESIAN_POINT('',(8.,-2.5,-1.675));
#51823=CARTESIAN_POINT('Origin',(8.,0.,0.));
#51824=CARTESIAN_POINT('Origin',(1.,0.,16.));
#51825=CARTESIAN_POINT('',(1.,-11.4941364764755,16.3671875));
#51826=CARTESIAN_POINT('Origin',(1.,0.,16.));
#51827=CARTESIAN_POINT('',(1.,11.4941364764755,16.3671875));
#51828=CARTESIAN_POINT('Origin',(1.,-13.8564064606,-8.));
#51829=CARTESIAN_POINT('',(1.,-8.42733192529161,-18.1378079331809));
#51830=CARTESIAN_POINT('Origin',(20.5,0.,0.));
#51831=CARTESIAN_POINT('',(20.5,-2.5,6.53834841531101));
#51832=CARTESIAN_POINT('',(20.5,2.5,6.53834841531101));
#51833=CARTESIAN_POINT('Origin',(20.5,0.,9.3));
#51834=CARTESIAN_POINT('',(20.5,2.5,9.3));
#51835=CARTESIAN_POINT('',(20.5,-2.5,9.3));
#51836=CARTESIAN_POINT('',(25.1,-2.57175827820944E-16,9.3));
#51837=CARTESIAN_POINT('Origin',(23.,0.,9.3));
#51838=CARTESIAN_POINT('Origin',(20.5,2.5,4.65));
#51839=CARTESIAN_POINT('Origin',(20.5,-2.5,4.65));
#51840=CARTESIAN_POINT('Origin',(23.,0.,10.));
#51841=CARTESIAN_POINT('',(25.1,2.57175827820944E-16,20.));
#51842=CARTESIAN_POINT('',(25.1,2.57175827820944E-16,10.));
#51843=CARTESIAN_POINT('',(20.9,0.,20.));
#51844=CARTESIAN_POINT('Ctrl Pts',(20.9,4.16333634234434E-16,20.));
#51845=CARTESIAN_POINT('Ctrl Pts',(20.9,0.263888990751172,20.));
#51846=CARTESIAN_POINT('Ctrl Pts',(20.9527780741314,0.545235237847868,19.9942425936951));
#51847=CARTESIAN_POINT('Ctrl Pts',(21.1671514943451,1.06257490219278,19.97343117591));
#51848=CARTESIAN_POINT('Ctrl Pts',(21.3287361087815,1.29858458976497,19.9586721250997));
#51849=CARTESIAN_POINT('Ctrl Pts',(21.7014161819223,1.67126466290584,19.9309254589373));
#51850=CARTESIAN_POINT('Ctrl Pts',(21.9374255317885,1.83284867450471,19.9161307432363));
#51851=CARTESIAN_POINT('Ctrl Pts',(22.4547640622183,2.04722164681422,19.8952376620524));
#51852=CARTESIAN_POINT('Ctrl Pts',(22.7361099164069,2.1,19.8894444366855));
#51853=CARTESIAN_POINT('Ctrl Pts',(23.2638900835931,2.1,19.8894444366855));
#51854=CARTESIAN_POINT('Ctrl Pts',(23.5452359377817,2.04722164681422,19.8952376620524));
#51855=CARTESIAN_POINT('Ctrl Pts',(24.0625744682115,1.83284867450471,19.9161307432363));
#51856=CARTESIAN_POINT('Ctrl Pts',(24.2985838180777,1.67126466290584,19.9309254589373));
#51857=CARTESIAN_POINT('Ctrl Pts',(24.6712638912185,1.29858458976497,19.9586721250997));
#51858=CARTESIAN_POINT('Ctrl Pts',(24.8328485056549,1.06257490219277,19.97343117591));
#51859=CARTESIAN_POINT('Ctrl Pts',(25.0472219258686,0.545235237847867,19.9942425936951));
#51860=CARTESIAN_POINT('Ctrl Pts',(25.1,0.263888990751172,20.));
#51861=CARTESIAN_POINT('Ctrl Pts',(25.1,-6.93889390390723E-17,20.));
#51862=CARTESIAN_POINT('',(23.,-2.1,19.8894444366855));
#51863=CARTESIAN_POINT('Ctrl Pts',(23.,-2.1,19.8894444366855));
#51864=CARTESIAN_POINT('Ctrl Pts',(22.7361099164069,-2.1,19.8894444366855));
#51865=CARTESIAN_POINT('Ctrl Pts',(22.4547640622183,-2.04722164681422,19.8952376620524));
#51866=CARTESIAN_POINT('Ctrl Pts',(21.9374255317885,-1.83284867450471,19.9161307432363));
#51867=CARTESIAN_POINT('Ctrl Pts',(21.7014161819223,-1.67126466290584,19.9309254589373));
#51868=CARTESIAN_POINT('Ctrl Pts',(21.3287361087815,-1.29858458976497,19.9586721250997));
#51869=CARTESIAN_POINT('Ctrl Pts',(21.1671514943451,-1.06257490219277,19.97343117591));
#51870=CARTESIAN_POINT('Ctrl Pts',(20.9527780741314,-0.545235237847867,
19.9942425936951));
#51871=CARTESIAN_POINT('Ctrl Pts',(20.9,-0.263888990751171,20.));
#51872=CARTESIAN_POINT('Ctrl Pts',(20.9,-5.20417042793042E-17,20.));
#51873=CARTESIAN_POINT('Ctrl Pts',(25.1,-3.46944695195361E-16,20.));
#51874=CARTESIAN_POINT('Ctrl Pts',(25.1,-0.263888990751172,20.));
#51875=CARTESIAN_POINT('Ctrl Pts',(25.0472219258686,-0.545235237847867,
19.9942425936951));
#51876=CARTESIAN_POINT('Ctrl Pts',(24.8328485056549,-1.06257490219277,19.97343117591));
#51877=CARTESIAN_POINT('Ctrl Pts',(24.6712638912185,-1.29858458976497,19.9586721250997));
#51878=CARTESIAN_POINT('Ctrl Pts',(24.2985838180777,-1.67126466290584,19.9309254589373));
#51879=CARTESIAN_POINT('Ctrl Pts',(24.0625744682115,-1.83284867450471,19.9161307432363));
#51880=CARTESIAN_POINT('Ctrl Pts',(23.5452359377817,-2.04722164681422,19.8952376620524));
#51881=CARTESIAN_POINT('Ctrl Pts',(23.2638900835931,-2.1,19.8894444366855));
#51882=CARTESIAN_POINT('Ctrl Pts',(23.,-2.1,19.8894444366855));
#51883=CARTESIAN_POINT('Origin',(13.,0.,0.));
#51884=CARTESIAN_POINT('',(13.,-2.44929359829471E-15,20.));
#51885=CARTESIAN_POINT('',(13.,-2.44929359829471E-15,20.));
#51886=CARTESIAN_POINT('',(4.3435534146,-2.1388888889,-19.8852999555184));
#51887=CARTESIAN_POINT('',(5.18767834635794,0.459060516890588,-19.9947308919583));
#51888=CARTESIAN_POINT('Ctrl Pts',(5.18767834635794,0.459060516890587,-19.9947308919583));
#51889=CARTESIAN_POINT('Ctrl Pts',(5.24968129137097,0.414012740477042,-19.9957651472147));
#51890=CARTESIAN_POINT('Ctrl Pts',(5.30716488138641,0.364591710747686,-19.9967442102515));
#51891=CARTESIAN_POINT('Ctrl Pts',(5.48665323742873,0.185057927007366,-19.9995504652193));
#51892=CARTESIAN_POINT('Ctrl Pts',(5.59715741138799,0.0235509943668747,
-20.0007685496482));
#51893=CARTESIAN_POINT('Ctrl Pts',(5.7436627884403,-0.330259044510279,-19.9980555602176));
#51894=CARTESIAN_POINT('Ctrl Pts',(5.7796645257,-0.522560848653025,-19.993985306904));
#51895=CARTESIAN_POINT('Ctrl Pts',(5.7796645257,-0.883349185014401,-19.9812997715422));
#51896=CARTESIAN_POINT('Ctrl Pts',(5.74353603624199,-1.07581469312434,-19.971831595325));
#51897=CARTESIAN_POINT('Ctrl Pts',(5.59681775573534,-1.4297140658822,-19.9496203526915));
#51898=CARTESIAN_POINT('Ctrl Pts',(5.48623409908571,-1.59115913013439,-19.9370154287515));
#51899=CARTESIAN_POINT('Ctrl Pts',(5.23128841814184,-1.84591622773468,-19.9150423979699));
#51900=CARTESIAN_POINT('Ctrl Pts',(5.06995436664432,-1.95632911293912,-19.9042256075891));
#51901=CARTESIAN_POINT('Ctrl Pts',(4.71629161866783,-2.10281902804406,-19.8892828626319));
#51902=CARTESIAN_POINT('Ctrl Pts',(4.52395392331701,-2.1388888889,-19.8852999555184));
#51903=CARTESIAN_POINT('Ctrl Pts',(4.3435534146,-2.1388888889,-19.8852999555184));
#51904=CARTESIAN_POINT('',(5.7631397208,2.1388888889,-19.8852999555184));
#51905=CARTESIAN_POINT('Origin',(5.03059422324816,0.0005165593435702,2.33120559308216));
#51906=CARTESIAN_POINT('',(4.7295794663,2.1388888889,-19.8852999555184));
#51907=CARTESIAN_POINT('',(5.24635959355,2.1388888889,-19.8852999555184));
#51908=CARTESIAN_POINT('',(4.2292347159,0.6783333333,-19.9884932871123));
#51909=CARTESIAN_POINT('Origin',(3.99709194624176,0.000685748014040422,
2.32885472330861));
#51910=CARTESIAN_POINT('',(3.7202200813,0.6783333333,-19.9884932871123));
#51911=CARTESIAN_POINT('',(3.9747273986,0.6783333333,-19.9884932871123));
#51912=CARTESIAN_POINT('',(3.7202200813,2.1388888889,-19.8852999555184));
#51913=CARTESIAN_POINT('Origin',(3.7202200813,0.,0.));
#51914=CARTESIAN_POINT('',(2.7424423035,2.1388888889,-19.8852999555184));
#51915=CARTESIAN_POINT('',(3.2313311924,2.1388888889,-19.8852999555184));
#51916=CARTESIAN_POINT('',(2.7424423035,-2.1388888889,-19.8852999555184));
#51917=CARTESIAN_POINT('Origin',(2.7424423035,0.,0.));
#51918=CARTESIAN_POINT('',(3.54299785905,-2.1388888889,-19.8852999555184));
#51919=CARTESIAN_POINT('',(1.4888888889,-1.1611111111,-19.9662670769395));
#51920=CARTESIAN_POINT('',(1.4888888889,2.1388888889,-19.8852999555184));
#51921=CARTESIAN_POINT('Origin',(1.4888888889,0.,0.));
#51922=CARTESIAN_POINT('',(0.5111111111,2.1388888889,-19.8852999555184));
#51923=CARTESIAN_POINT('',(1.,2.1388888889,-19.8852999555184));
#51924=CARTESIAN_POINT('',(0.5111111111,-1.1611111111,-19.9662670769395));
#51925=CARTESIAN_POINT('Origin',(0.5111111111,0.,0.));
#51926=CARTESIAN_POINT('',(-0.5277777778,-1.1611111111,-19.9662670769395));
#51927=CARTESIAN_POINT('',(-0.00833333335000042,-1.1611111111,-19.9662670769395));
#51928=CARTESIAN_POINT('',(-0.5277777778,-2.1388888889,-19.8852999555184));
#51929=CARTESIAN_POINT('Origin',(-0.527777777800001,0.,0.));
#51930=CARTESIAN_POINT('',(2.5277777778,-2.1388888889,-19.8852999555184));
#51931=CARTESIAN_POINT('',(1.,-2.1388888889,-19.8852999555184));
#51932=CARTESIAN_POINT('',(2.5277777778,-1.1611111111,-19.9662670769395));
#51933=CARTESIAN_POINT('Origin',(2.5277777778,0.,0.));
#51934=CARTESIAN_POINT('',(2.00833333335,-1.1611111111,-19.9662670769395));
#51935=CARTESIAN_POINT('',(-3.7631397208,2.75,-19.8100353356575));
#51936=CARTESIAN_POINT('',(-1.8075841652,2.75,-19.8100353356575));
#51937=CARTESIAN_POINT('',(-2.785361943,2.75,-19.8100353356575));
#51938=CARTESIAN_POINT('',(1.,4.3709594736,-19.5165241085637));
#51939=CARTESIAN_POINT('Origin',(-6.57072388981035,-2.27381335982102E-9,
1.34364674941878E-8));
#51940=CARTESIAN_POINT('',(3.8075841652,2.75,-19.8100353356575));
#51941=CARTESIAN_POINT('Origin',(8.5707238638722,1.26959015522843E-8,-6.91637080940666E-8));
#51942=CARTESIAN_POINT('',(5.7631397208,2.75,-19.8100353356575));
#51943=CARTESIAN_POINT('',(4.785361943,2.75,-19.8100353356575));
#51944=CARTESIAN_POINT('',(1.,5.5,-19.2288845230294));
#51945=CARTESIAN_POINT('Origin',(10.526279440744,4.94369545300799E-10,-2.25620633287349E-9));
#51946=CARTESIAN_POINT('Origin',(-8.52627944326717,-9.62673274429449E-10,
4.51972903547926E-9));
#51947=CARTESIAN_POINT('',(-1.9747474276,-0.2016666667,-19.9989832380434));
#51948=CARTESIAN_POINT('',(-0.5561396937,2.1388888889,-19.8852999555184));
#51949=CARTESIAN_POINT('Origin',(-1.85251751839491,0.,0.));
#51950=CARTESIAN_POINT('',(-1.6994942043,2.1388888889,-19.8852999555184));
#51951=CARTESIAN_POINT('',(-1.127816949,2.1388888889,-19.8852999555184));
#51952=CARTESIAN_POINT('',(-2.785361943,0.3473197978,-19.9969839965445));
#51953=CARTESIAN_POINT('Origin',(-2.99587202900023,0.,0.));
#51954=CARTESIAN_POINT('',(-2.785361943,2.1388888889,-19.8852999555184));
#51955=CARTESIAN_POINT('Origin',(-2.785361943,0.,0.));
#51956=CARTESIAN_POINT('',(-3.7631397208,2.1388888889,-19.8852999555184));
#51957=CARTESIAN_POINT('',(-3.2742508319,2.1388888889,-19.8852999555184));
#51958=CARTESIAN_POINT('',(-3.7631397208,-2.1388888889,-19.8852999555184));
#51959=CARTESIAN_POINT('Origin',(-3.7631397208,0.,0.));
#51960=CARTESIAN_POINT('',(-2.785361943,-2.1388888889,-19.8852999555184));
#51961=CARTESIAN_POINT('',(-3.2742508319,-2.1388888889,-19.8852999555184));
#51962=CARTESIAN_POINT('',(-2.785361943,-0.7484330612,-19.9859912927256));
#51963=CARTESIAN_POINT('Origin',(-2.785361943,0.,0.));
#51964=CARTESIAN_POINT('',(-1.8474876449,-2.1388888889,-19.8852999555184));
#51965=CARTESIAN_POINT('Origin',(-3.29018641707832,0.,0.));
#51966=CARTESIAN_POINT('',(-0.6680745397,-2.1388888889,-19.8852999555184));
#51967=CARTESIAN_POINT('',(-1.2577810923,-2.1388888889,-19.8852999555184));
#51968=CARTESIAN_POINT('Origin',(-2.11077331185338,0.,0.));
#51969=CARTESIAN_POINT('',(1.,-4.3709594736,-19.5165241085637));
#51970=CARTESIAN_POINT('',(-1.8075841652,-2.75,-19.8100353356575));
#51971=CARTESIAN_POINT('Origin',(-6.57072387874695,-4.11288225699025E-9,
-2.09971195985759E-8));
#51972=CARTESIAN_POINT('',(-3.7631397208,-2.75,-19.8100353356575));
#51973=CARTESIAN_POINT('',(-2.785361943,-2.75,-19.8100353356575));
#51974=CARTESIAN_POINT('',(1.,-5.5,-19.2288845230294));
#51975=CARTESIAN_POINT('Origin',(-8.52627944334428,1.00725594531781E-9,
4.7267834091258E-9));
#51976=CARTESIAN_POINT('',(5.7631397208,-2.75,-19.8100353356575));
#51977=CARTESIAN_POINT('Origin',(10.5262794407692,-4.79505324335605E-10,
-2.19413154312065E-9));
#51978=CARTESIAN_POINT('',(3.8075841652,-2.75,-19.8100353356575));
#51979=CARTESIAN_POINT('',(4.785361943,-2.75,-19.8100353356575));
#51980=CARTESIAN_POINT('Origin',(8.57072386754017,-1.05836966968198E-8,
-5.72841307722172E-8));
#51981=CARTESIAN_POINT('Origin',(1.,0.,0.));
#51982=CARTESIAN_POINT('',(1.4888888889,2.1388888889,-19.3823413013222));
#51983=CARTESIAN_POINT('',(1.4888888889,-1.1611111111,-19.4654006120521));
#51984=CARTESIAN_POINT('Origin',(1.4888888889,0.,0.));
#51985=CARTESIAN_POINT('',(2.5277777778,-1.1611111111,-19.4654006120521));
#51986=CARTESIAN_POINT('',(2.00833333335,-1.1611111111,-19.4654006120521));
#51987=CARTESIAN_POINT('',(2.5277777778,-2.1388888889,-19.3823413013222));
#51988=CARTESIAN_POINT('Origin',(2.5277777778,0.,0.));
#51989=CARTESIAN_POINT('',(-0.5277777778,-2.1388888889,-19.3823413013222));
#51990=CARTESIAN_POINT('',(1.,-2.1388888889,-19.3823413013222));
#51991=CARTESIAN_POINT('',(-0.5277777778,-1.1611111111,-19.4654006120521));
#51992=CARTESIAN_POINT('Origin',(-0.5277777778,0.,0.));
#51993=CARTESIAN_POINT('',(0.5111111111,-1.1611111111,-19.4654006120521));
#51994=CARTESIAN_POINT('',(-0.00833333334999997,-1.1611111111,-19.4654006120521));
#51995=CARTESIAN_POINT('',(0.5111111111,2.1388888889,-19.3823413013222));
#51996=CARTESIAN_POINT('Origin',(0.5111111111,0.,0.));
#51997=CARTESIAN_POINT('',(1.,2.1388888889,-19.3823413013222));
#51998=CARTESIAN_POINT('Origin',(0.5111111111,0.4888888889,0.));
#51999=CARTESIAN_POINT('',(0.5111111111,2.1388888889,0.));
#52000=CARTESIAN_POINT('',(0.5111111111,-1.1611111111,0.));
#52001=CARTESIAN_POINT('Origin',(1.,2.1388888889,0.));
#52002=CARTESIAN_POINT('',(1.4888888889,2.1388888889,0.));
#52003=CARTESIAN_POINT('Origin',(-0.00833333334999997,-1.1611111111,0.));
#52004=CARTESIAN_POINT('',(-0.5277777778,-1.1611111111,0.));
#52005=CARTESIAN_POINT('Origin',(-0.5277777778,-1.65,0.));
#52006=CARTESIAN_POINT('',(-0.5277777778,-2.1388888889,0.));
#52007=CARTESIAN_POINT('Origin',(1.,-2.1388888889,0.));
#52008=CARTESIAN_POINT('',(2.5277777778,-2.1388888889,0.));
#52009=CARTESIAN_POINT('Origin',(2.5277777778,-1.65,0.));
#52010=CARTESIAN_POINT('',(2.5277777778,-1.1611111111,0.));
#52011=CARTESIAN_POINT('Origin',(2.00833333335,-1.1611111111,0.));
#52012=CARTESIAN_POINT('',(1.4888888889,-1.1611111111,0.));
#52013=CARTESIAN_POINT('Origin',(1.4888888889,0.4888888889,0.));
#52014=CARTESIAN_POINT('Origin',(-2.24242807365,1.24310434335,0.));
#52015=CARTESIAN_POINT('',(-1.6994942043,2.1388888889,-19.3823413013222));
#52016=CARTESIAN_POINT('',(-1.6994942043,2.1388888889,0.));
#52017=CARTESIAN_POINT('',(-2.785361943,0.3473197978,-19.4969066510064));
#52018=CARTESIAN_POINT('Origin',(-2.99587202900024,0.,0.));
#52019=CARTESIAN_POINT('',(-2.785361943,0.3473197978,0.));
#52020=CARTESIAN_POINT('Origin',(-1.127816949,2.1388888889,0.));
#52021=CARTESIAN_POINT('',(-0.5561396937,2.1388888889,-19.3823413013222));
#52022=CARTESIAN_POINT('',(-0.5561396937,2.1388888889,0.));
#52023=CARTESIAN_POINT('',(-1.127816949,2.1388888889,-19.3823413013222));
#52024=CARTESIAN_POINT('Origin',(-1.26544356065,0.9686111111,0.));
#52025=CARTESIAN_POINT('',(-1.9747474276,-0.2016666667,-19.4989571658472));
#52026=CARTESIAN_POINT('',(-1.9747474276,-0.2016666667,0.));
#52027=CARTESIAN_POINT('Origin',(-1.85251751839491,0.,0.));
#52028=CARTESIAN_POINT('Origin',(-1.2577810923,-2.1388888889,0.));
#52029=CARTESIAN_POINT('',(-1.8474876449,-2.1388888889,-19.3823413013222));
#52030=CARTESIAN_POINT('',(-1.8474876449,-2.1388888889,0.));
#52031=CARTESIAN_POINT('',(-0.6680745397,-2.1388888889,-19.3823413013222));
#52032=CARTESIAN_POINT('',(-1.2577810923,-2.1388888889,-19.3823413013222));
#52033=CARTESIAN_POINT('',(-0.6680745397,-2.1388888889,0.));
#52034=CARTESIAN_POINT('Origin',(-2.31642479395,-1.44366097505,0.));
#52035=CARTESIAN_POINT('',(-2.785361943,-0.7484330612,-19.4856318335563));
#52036=CARTESIAN_POINT('',(-2.785361943,-0.7484330612,0.));
#52037=CARTESIAN_POINT('Origin',(-3.29018641707832,0.,0.));
#52038=CARTESIAN_POINT('Origin',(-2.785361943,-1.44366097505,0.));
#52039=CARTESIAN_POINT('',(-2.785361943,-2.1388888889,-19.3823413013222));
#52040=CARTESIAN_POINT('',(-2.785361943,-2.1388888889,0.));
#52041=CARTESIAN_POINT('Origin',(-2.785361943,0.,0.));
#52042=CARTESIAN_POINT('Origin',(-3.2742508319,-2.1388888889,0.));
#52043=CARTESIAN_POINT('',(-3.7631397208,-2.1388888889,-19.3823413013222));
#52044=CARTESIAN_POINT('',(-3.7631397208,-2.1388888889,0.));
#52045=CARTESIAN_POINT('',(-3.2742508319,-2.1388888889,-19.3823413013222));
#52046=CARTESIAN_POINT('Origin',(-3.7631397208,0.,0.));
#52047=CARTESIAN_POINT('',(-3.7631397208,2.1388888889,-19.3823413013222));
#52048=CARTESIAN_POINT('',(-3.7631397208,2.1388888889,0.));
#52049=CARTESIAN_POINT('Origin',(-3.7631397208,0.,0.));
#52050=CARTESIAN_POINT('Origin',(-3.2742508319,2.1388888889,0.));
#52051=CARTESIAN_POINT('',(-2.785361943,2.1388888889,-19.3823413013222));
#52052=CARTESIAN_POINT('',(-2.785361943,2.1388888889,0.));
#52053=CARTESIAN_POINT('',(-3.2742508319,2.1388888889,-19.3823413013222));
#52054=CARTESIAN_POINT('Origin',(-2.785361943,1.24310434335,0.));
#52055=CARTESIAN_POINT('Origin',(-2.785361943,0.,0.));
#52056=CARTESIAN_POINT('Origin',(-1.32141098365,-1.1702777778,0.));
#52057=CARTESIAN_POINT('Origin',(-2.11077331185338,0.,0.));
#52058=CARTESIAN_POINT('Origin',(1.,0.,0.));
#52059=CARTESIAN_POINT('Origin',(1.,0.,0.));
#52060=CARTESIAN_POINT('',(1.,5.5,-18.7082869338697));
#52061=CARTESIAN_POINT('',(5.7631397208,2.75,-19.305115902268));
#52062=CARTESIAN_POINT('Origin',(10.5262794424987,-5.18419751571741E-10,
2.36643593609642E-9));
#52063=CARTESIAN_POINT('',(3.8075841652,2.75,-19.305115902268));
#52064=CARTESIAN_POINT('',(4.785361943,2.75,-19.305115902268));
#52065=CARTESIAN_POINT('',(1.,4.3709594736,-19.0038078626402));
#52066=CARTESIAN_POINT('Origin',(8.570723907158,-1.22962007242933E-8,6.41915343102539E-8));
#52067=CARTESIAN_POINT('',(-1.8075841652,2.75,-19.305115902268));
#52068=CARTESIAN_POINT('Origin',(-6.57072388594774,-4.93771690202038E-11,
4.65181226871891E-10));
#52069=CARTESIAN_POINT('',(-3.7631397208,2.75,-19.305115902268));
#52070=CARTESIAN_POINT('',(-2.785361943,2.75,-19.305115902268));
#52071=CARTESIAN_POINT('Origin',(-8.5262794404497,6.64190369370488E-10,
-3.11044967560292E-9));
#52072=CARTESIAN_POINT('Origin',(2.4037920826,3.5604797368,0.));
#52073=CARTESIAN_POINT('',(1.,4.3709594736,0.));
#52074=CARTESIAN_POINT('',(3.8075841652,2.75,0.));
#52075=CARTESIAN_POINT('Origin',(-0.4037920826,3.5604797368,0.));
#52076=CARTESIAN_POINT('',(-1.8075841652,2.75,0.));
#52077=CARTESIAN_POINT('Origin',(4.785361943,2.75,0.));
#52078=CARTESIAN_POINT('',(5.7631397208,2.75,0.));
#52079=CARTESIAN_POINT('Origin',(3.3815698604,4.125,0.));
#52080=CARTESIAN_POINT('',(1.,5.5,0.));
#52081=CARTESIAN_POINT('Origin',(-1.3815698604,4.125,0.));
#52082=CARTESIAN_POINT('',(-3.7631397208,2.75,0.));
#52083=CARTESIAN_POINT('Origin',(-2.785361943,2.75,0.));
#52084=CARTESIAN_POINT('Origin',(4.785361943,-2.75,0.));
#52085=CARTESIAN_POINT('',(5.7631397208,-2.75,-19.305115902268));
#52086=CARTESIAN_POINT('',(5.7631397208,-2.75,0.));
#52087=CARTESIAN_POINT('',(3.8075841652,-2.75,-19.305115902268));
#52088=CARTESIAN_POINT('',(4.785361943,-2.75,-19.305115902268));
#52089=CARTESIAN_POINT('',(3.8075841652,-2.75,0.));
#52090=CARTESIAN_POINT('Origin',(3.3815698604,-4.125,0.));
#52091=CARTESIAN_POINT('',(1.,-5.5,-18.7082869338697));
#52092=CARTESIAN_POINT('',(1.,-5.5,0.));
#52093=CARTESIAN_POINT('Origin',(10.5262794400813,-8.77110606367637E-10,
-4.09533296164E-9));
#52094=CARTESIAN_POINT('Origin',(-1.3815698604,-4.125,0.));
#52095=CARTESIAN_POINT('',(-3.7631397208,-2.75,-19.305115902268));
#52096=CARTESIAN_POINT('',(-3.7631397208,-2.75,0.));
#52097=CARTESIAN_POINT('Origin',(-8.52627944078166,-4.73031613879016E-10,
-2.23582041769532E-9));
#52098=CARTESIAN_POINT('Origin',(-2.785361943,-2.75,0.));
#52099=CARTESIAN_POINT('',(-1.8075841652,-2.75,-19.305115902268));
#52100=CARTESIAN_POINT('',(-1.8075841652,-2.75,0.));
#52101=CARTESIAN_POINT('',(-2.785361943,-2.75,-19.305115902268));
#52102=CARTESIAN_POINT('Origin',(2.4037920826,-3.5604797368,0.));
#52103=CARTESIAN_POINT('',(1.,-4.3709594736,-19.0038078626402));
#52104=CARTESIAN_POINT('Origin',(8.57072389406941,4.73950212409591E-9,2.49748000058503E-8));
#52105=CARTESIAN_POINT('',(1.,-4.3709594736,0.));
#52106=CARTESIAN_POINT('Origin',(-0.4037920826,-3.5604797368,0.));
#52107=CARTESIAN_POINT('Origin',(-6.57072389929174,7.75191022484023E-9,
4.058589020417E-8));
#52108=CARTESIAN_POINT('Origin',(1.,0.,0.));
#52109=CARTESIAN_POINT('Origin',(4.4794070911,1.4086111111,0.));
#52110=CARTESIAN_POINT('',(4.7295794663,2.1388888889,-19.3823413013222));
#52111=CARTESIAN_POINT('',(4.7295794663,2.1388888889,0.));
#52112=CARTESIAN_POINT('',(4.2292347159,0.6783333333,-19.4881980667514));
#52113=CARTESIAN_POINT('Origin',(3.99710417002144,0.000721430429313635,
2.2697089266716));
#52114=CARTESIAN_POINT('',(4.2292347159,0.6783333333,0.));
#52115=CARTESIAN_POINT('Origin',(5.24635959355,2.1388888889,0.));
#52116=CARTESIAN_POINT('',(5.7631397208,2.1388888889,-19.3823413013222));
#52117=CARTESIAN_POINT('',(5.7631397208,2.1388888889,0.));
#52118=CARTESIAN_POINT('',(5.24635959355,2.1388888889,-19.3823413013222));
#52119=CARTESIAN_POINT('Origin',(5.47540903359635,1.29897470288934,0.));
#52120=CARTESIAN_POINT('',(5.18767834635794,0.459060516890588,-19.4945957496387));
#52121=CARTESIAN_POINT('',(5.18767834635794,0.459060516890588,0.));
#52122=CARTESIAN_POINT('Origin',(5.03060343765304,0.000543454432446466,
2.27211957514992));
#52123=CARTESIAN_POINT('Origin',(4.3435534146,-0.7027777778,0.));
#52124=CARTESIAN_POINT('',(4.3435534146,-2.1388888889,-19.3823413013222));
#52125=CARTESIAN_POINT('',(4.3435534146,-2.1388888889,0.));
#52126=CARTESIAN_POINT('Ctrl Pts',(4.3435534146,-2.1388888889,-19.3823413013222));
#52127=CARTESIAN_POINT('Ctrl Pts',(4.52395809426988,-2.1388888889,-19.3823413013222));
#52128=CARTESIAN_POINT('Ctrl Pts',(4.71629563622818,-2.10281731621556,-19.3864277949426));
#52129=CARTESIAN_POINT('Ctrl Pts',(5.06994974058055,-1.95633107681449,-19.4017574464858));
#52130=CARTESIAN_POINT('Ctrl Pts',(5.23127577915034,-1.84592395078976,-19.4128536921776));
#52131=CARTESIAN_POINT('Ctrl Pts',(5.48621793448543,-1.59118019669263,-19.4353935671731));
#52132=CARTESIAN_POINT('Ctrl Pts',(5.59680474635876,-1.42973736216137,-19.4483236475342));
#52133=CARTESIAN_POINT('Ctrl Pts',(5.74353126970954,-1.07583427316188,-19.4711073706637));
#52134=CARTESIAN_POINT('Ctrl Pts',(5.7796645257,-0.883362239425408,-19.4808193953452));
#52135=CARTESIAN_POINT('Ctrl Pts',(5.7796645257,-0.522566272387348,-19.4938308937715));
#52136=CARTESIAN_POINT('Ctrl Pts',(5.74366463353765,-0.330266483099083,
-19.4980055699564));
#52137=CARTESIAN_POINT('Ctrl Pts',(5.59716211486846,0.0235426180269262,
-19.500788263579));
#52138=CARTESIAN_POINT('Ctrl Pts',(5.48665892619763,0.185050560069143,-19.4995390181328));
#52139=CARTESIAN_POINT('Ctrl Pts',(5.30716969365494,0.364587581151339,-19.4966607992451));
#52140=CARTESIAN_POINT('Ctrl Pts',(5.24968384954062,0.414010881858001,-19.495656582549));
#52141=CARTESIAN_POINT('Ctrl Pts',(5.18767834635794,0.459060516890588,-19.4945957496387));
#52142=CARTESIAN_POINT('Origin',(3.54299785905,-2.1388888889,0.));
#52143=CARTESIAN_POINT('',(2.7424423035,-2.1388888889,-19.3823413013222));
#52144=CARTESIAN_POINT('',(2.7424423035,-2.1388888889,0.));
#52145=CARTESIAN_POINT('',(3.54299785905,-2.1388888889,-19.3823413013222));
#52146=CARTESIAN_POINT('Origin',(3.7202200813,-0.7027777778,0.));
#52147=CARTESIAN_POINT('',(3.7202200813,-1.1061111111,-19.468603396492));
#52148=CARTESIAN_POINT('',(3.7202200813,-1.1061111111,0.));
#52149=CARTESIAN_POINT('',(3.7202200813,-0.2994444445,-19.497700711229));
#52150=CARTESIAN_POINT('Origin',(3.7202200813,0.,0.));
#52151=CARTESIAN_POINT('',(3.7202200813,-0.2994444445,0.));
#52152=CARTESIAN_POINT('Origin',(4.03188674795,-1.1061111111,0.));
#52153=CARTESIAN_POINT('',(4.3435534146,-1.1061111111,-19.468603396492));
#52154=CARTESIAN_POINT('',(4.3435534146,-1.1061111111,0.));
#52155=CARTESIAN_POINT('',(4.03188674795,-1.1061111111,-19.468603396492));
#52156=CARTESIAN_POINT('Origin',(2.7424423035,0.,0.));
#52157=CARTESIAN_POINT('',(2.7424423035,2.1388888889,-19.3823413013222));
#52158=CARTESIAN_POINT('',(2.7424423035,2.1388888889,0.));
#52159=CARTESIAN_POINT('Origin',(2.7424423035,0.,0.));
#52160=CARTESIAN_POINT('Origin',(3.2313311924,2.1388888889,0.));
#52161=CARTESIAN_POINT('',(3.7202200813,2.1388888889,-19.3823413013222));
#52162=CARTESIAN_POINT('',(3.7202200813,2.1388888889,0.));
#52163=CARTESIAN_POINT('',(3.2313311924,2.1388888889,-19.3823413013222));
#52164=CARTESIAN_POINT('Origin',(3.7202200813,1.4086111111,0.));
#52165=CARTESIAN_POINT('',(3.7202200813,0.6783333333,-19.4881980667514));
#52166=CARTESIAN_POINT('',(3.7202200813,0.6783333333,0.));
#52167=CARTESIAN_POINT('Origin',(3.7202200813,0.,0.));
#52168=CARTESIAN_POINT('Origin',(3.9747273986,0.6783333333,0.));
#52169=CARTESIAN_POINT('',(3.9747273986,0.6783333333,-19.4881980667514));
#52170=CARTESIAN_POINT('Origin',(4.3435534146,-0.7027777778,0.));
#52171=CARTESIAN_POINT('',(4.3435534146,-0.2994444445,-19.497700711229));
#52172=CARTESIAN_POINT('',(4.3435534146,-0.2994444445,0.));
#52173=CARTESIAN_POINT('Ctrl Pts',(4.3435534146,-1.1061111111,-19.468603396492));
#52174=CARTESIAN_POINT('Ctrl Pts',(4.39419814308983,-1.1061111111,-19.468603396492));
#52175=CARTESIAN_POINT('Ctrl Pts',(4.44821225425436,-1.0959892259289,-19.4691867368818));
#52176=CARTESIAN_POINT('Ctrl Pts',(4.54756315899303,-1.0548413233652,-19.4714594820528));
#52177=CARTESIAN_POINT('Ctrl Pts',(4.59290043242865,-1.02381583731486,-19.4731375157807));
#52178=CARTESIAN_POINT('Ctrl Pts',(4.66452631029908,-0.952218736036693,
-19.4767698957415));
#52179=CARTESIAN_POINT('Ctrl Pts',(4.69557900256288,-0.906859343552727,
-19.4789650772337));
#52180=CARTESIAN_POINT('Ctrl Pts',(4.73675930343402,-0.807469845951887,
-19.4833381841241));
#52181=CARTESIAN_POINT('Ctrl Pts',(4.7468867479,-0.75343917779947,-19.4855048515763));
#52182=CARTESIAN_POINT('Ctrl Pts',(4.7468867479,-0.652145736281435,-19.4891578288136));
#52183=CARTESIAN_POINT('Ctrl Pts',(4.73676979677675,-0.598128620436881,
-19.4908879558739));
#52184=CARTESIAN_POINT('Ctrl Pts',(4.69560712746241,-0.498746523663012,
-19.4936841838618));
#52185=CARTESIAN_POINT('Ctrl Pts',(4.66456102115108,-0.453382021110974,
-19.4947615621894));
#52186=CARTESIAN_POINT('Ctrl Pts',(4.59293064696051,-0.381759433086016,
-19.4962956016238));
#52187=CARTESIAN_POINT('Ctrl Pts',(4.54757997199792,-0.350722506379112,
-19.4968566012566));
#52188=CARTESIAN_POINT('Ctrl Pts',(4.44821221942384,-0.309565004720403,
-19.4975535161267));
#52189=CARTESIAN_POINT('Ctrl Pts',(4.39419521514208,-0.2994444445,-19.497700711229));
#52190=CARTESIAN_POINT('Ctrl Pts',(4.3435534146,-0.2994444445,-19.497700711229));
#52191=CARTESIAN_POINT('Origin',(4.03188674795,-0.2994444445,0.));
#52192=CARTESIAN_POINT('',(4.03188674795,-0.2994444445,-19.497700711229));
#52193=CARTESIAN_POINT('Origin',(1.,0.,0.));
#52194=CARTESIAN_POINT('',(0.,0.,0.));
#52195=CARTESIAN_POINT('Origin',(-23.,0.,-18.4));
#52196=CARTESIAN_POINT('',(-25.5,-3.06161699786838E-16,-18.4));
#52197=CARTESIAN_POINT('Origin',(-23.,0.,-18.4));
#52198=CARTESIAN_POINT('',(-23.,-1.3856406461,-18.4));
#52199=CARTESIAN_POINT('',(-21.8,-0.692820323,-18.4));
#52200=CARTESIAN_POINT('',(-22.3999999999746,-1.03923048453533,-18.4));
#52201=CARTESIAN_POINT('',(-21.8,0.692820323,-18.4));
#52202=CARTESIAN_POINT('',(-21.8,0.17320508075,-18.4));
#52203=CARTESIAN_POINT('',(-23.,1.3856406461,-18.4));
#52204=CARTESIAN_POINT('',(-22.3999999999746,1.03923048453533,-18.4));
#52205=CARTESIAN_POINT('',(-24.2,0.692820323,-18.4));
#52206=CARTESIAN_POINT('',(-23.6000000000254,1.03923048453533,-18.4));
#52207=CARTESIAN_POINT('',(-24.2,-0.692820323,-18.4));
#52208=CARTESIAN_POINT('',(-24.2,0.,-18.4));
#52209=CARTESIAN_POINT('',(-23.6000000000254,-1.03923048453533,-18.4));
#52210=CARTESIAN_POINT('Origin',(-23.,0.,-6.4));
#52211=CARTESIAN_POINT('',(-25.5,-3.06161699786838E-16,-6.4));
#52212=CARTESIAN_POINT('Origin',(-23.,0.,-6.4));
#52213=CARTESIAN_POINT('Origin',(-23.,0.,-12.4));
#52214=CARTESIAN_POINT('',(-25.5,3.06161699786838E-16,-12.4));
#52215=CARTESIAN_POINT('Origin',(-23.,3.11198878113149E-17,-15.9));
#52216=CARTESIAN_POINT('',(-24.2,-0.692820323,-15.9));
#52217=CARTESIAN_POINT('',(-23.,-1.3856406461,-15.9));
#52218=CARTESIAN_POINT('',(-24.2,-0.692820323,-15.9));
#52219=CARTESIAN_POINT('',(-24.2,0.692820323,-15.9));
#52220=CARTESIAN_POINT('',(-24.2,0.692820323,-15.9));
#52221=CARTESIAN_POINT('',(-23.,1.3856406461,-15.9));
#52222=CARTESIAN_POINT('',(-23.,1.3856406461,-15.9));
#52223=CARTESIAN_POINT('',(-21.8,0.692820323,-15.9));
#52224=CARTESIAN_POINT('',(-21.8,0.692820323,-15.9));
#52225=CARTESIAN_POINT('',(-21.8,-0.692820323,-15.9));
#52226=CARTESIAN_POINT('',(-21.8,-0.692820323,-15.9));
#52227=CARTESIAN_POINT('',(-23.,-1.3856406461,-15.9));
#52228=CARTESIAN_POINT('Origin',(-23.6,-1.03923048455,-15.9));
#52229=CARTESIAN_POINT('',(-24.2,-0.692820323,-15.9));
#52230=CARTESIAN_POINT('',(-23.,-1.3856406461,-15.9));
#52231=CARTESIAN_POINT('Origin',(-24.2,0.,-15.9));
#52232=CARTESIAN_POINT('',(-24.2,0.692820323,-15.9));
#52233=CARTESIAN_POINT('Origin',(-23.6,1.03923048455,-15.9));
#52234=CARTESIAN_POINT('',(-23.,1.3856406461,-15.9));
#52235=CARTESIAN_POINT('Origin',(-22.4,1.03923048455,-15.9));
#52236=CARTESIAN_POINT('',(-21.8,0.692820323,-15.9));
#52237=CARTESIAN_POINT('Origin',(-21.8,0.3464101615,-15.9));
#52238=CARTESIAN_POINT('',(-21.8,-0.692820323,-15.9));
#52239=CARTESIAN_POINT('Origin',(-22.4,-1.03923048455,-15.9));
#52240=CARTESIAN_POINT('',(0.,0.,0.));
#52241=CARTESIAN_POINT('Origin',(6.,0.,10.));
#52242=CARTESIAN_POINT('',(6.,-11.5470739757602,-3.26574380475891));
#52243=CARTESIAN_POINT('',(6.,-19.921468401738,-1.77062043322529));
#52244=CARTESIAN_POINT('Origin',(6.,-13.8564064606,8.));
#52245=CARTESIAN_POINT('',(6.,-11.4941364764755,-16.3671875));
#52246=CARTESIAN_POINT('Origin',(6.,0.,0.));
#52247=CARTESIAN_POINT('',(6.,-8.60175408505985,-8.3671875));
#52248=CARTESIAN_POINT('Origin',(6.,0.,-16.));
#52249=CARTESIAN_POINT('Origin',(6.,0.,0.));
#52250=CARTESIAN_POINT('Origin',(-33.,0.,9.5));
#52251=CARTESIAN_POINT('',(-33.,2.32682891837997E-15,-19.));
#52252=CARTESIAN_POINT('Origin',(-33.,0.,0.));
#52253=CARTESIAN_POINT('',(-33.,-1.5,-4.76969600708473));
#52254=CARTESIAN_POINT('',(-33.,-1.5,-6.4));
#52255=CARTESIAN_POINT('',(-33.,-1.5,3.15));
#52256=CARTESIAN_POINT('',(-33.,1.5,-6.4));
#52257=CARTESIAN_POINT('',(-33.,0.,-6.4));
#52258=CARTESIAN_POINT('',(-33.,1.5,-4.76969600708473));
#52259=CARTESIAN_POINT('',(-33.,1.5,3.15));
#52260=CARTESIAN_POINT('Origin',(-33.,0.,0.));
#52261=CARTESIAN_POINT('Origin',(-32.5,0.,0.));
#52262=CARTESIAN_POINT('',(-32.,2.44929359829471E-15,-20.));
#52263=CARTESIAN_POINT('Origin',(-32.,0.,0.));
#52264=CARTESIAN_POINT('',(-32.5,2.38806125833734E-15,-19.5));
#52265=CARTESIAN_POINT('Origin',(-13.,0.,0.));
#52266=CARTESIAN_POINT('',(-3.7202200813,-0.2994444445,19.9977581999748));
#52267=CARTESIAN_POINT('',(-4.3435534146,-0.2994444445,19.9977581999748));
#52268=CARTESIAN_POINT('',(-4.03188674795,-0.2994444445,19.9977581999748));
#52269=CARTESIAN_POINT('',(-4.3435534146,-1.1061111111,19.969389530226));
#52270=CARTESIAN_POINT('Ctrl Pts',(-4.3435534146,-0.2994444445,19.9977581999748));
#52271=CARTESIAN_POINT('Ctrl Pts',(-4.39419529583398,-0.2994444445,19.9977581999748));
#52272=CARTESIAN_POINT('Ctrl Pts',(-4.44821240138141,-0.309565031449933,
19.9976146851541));
#52273=CARTESIAN_POINT('Ctrl Pts',(-4.54758041279513,-0.350722737591021,
19.9969351943239));
#52274=CARTESIAN_POINT('Ctrl Pts',(-4.59293124895252,-0.381759842781414,
19.9963882206146));
#52275=CARTESIAN_POINT('Ctrl Pts',(-4.66456114163788,-0.453382333903515,
19.994892548385));
#52276=CARTESIAN_POINT('Ctrl Pts',(-4.69560697302298,-0.498746314496724,
19.993842130762));
#52277=CARTESIAN_POINT('Ctrl Pts',(-4.73676959169473,-0.5981279615852,19.9911158762495));
#52278=CARTESIAN_POINT('Ctrl Pts',(-4.7468867479,-0.652145173345914,19.9894290439444));
#52279=CARTESIAN_POINT('Ctrl Pts',(-4.7468867479,-0.753438288963382,19.9858675169476));
#52280=CARTESIAN_POINT('Ctrl Pts',(-4.73675961734101,-0.80746838265751,
19.9837551246746));
#52281=CARTESIAN_POINT('Ctrl Pts',(-4.69558023913546,-0.906857064706403,
19.9794915935354));
#52282=CARTESIAN_POINT('Ctrl Pts',(-4.66452814741898,-0.952216188266304,
19.9773514320566));
#52283=CARTESIAN_POINT('Ctrl Pts',(-4.59290252845076,-1.02381445280548,
19.9738100392531));
#52284=CARTESIAN_POINT('Ctrl Pts',(-4.54756443095206,-1.05484068319396,
19.9721740344373));
#52285=CARTESIAN_POINT('Ctrl Pts',(-4.44821243395584,-1.09598926486806,
19.9699582388217));
#52286=CARTESIAN_POINT('Ctrl Pts',(-4.39419807843,-1.1061111111,19.969389530226));
#52287=CARTESIAN_POINT('Ctrl Pts',(-4.3435534146,-1.1061111111,19.969389530226));
#52288=CARTESIAN_POINT('',(-3.7202200813,-1.1061111111,19.969389530226));
#52289=CARTESIAN_POINT('',(-4.03188674795,-1.1061111111,19.969389530226));
#52290=CARTESIAN_POINT('Origin',(-3.7202200813,0.,0.));
#52291=CARTESIAN_POINT('Origin',(6.,0.,10.));
#52292=CARTESIAN_POINT('',(6.,8.60175408505985,-8.3671875));
#52293=CARTESIAN_POINT('',(6.,11.4941364764755,-16.3671875));
#52294=CARTESIAN_POINT('Origin',(6.,0.,-16.));
#52295=CARTESIAN_POINT('',(6.,19.921468401738,-1.77062043322529));
#52296=CARTESIAN_POINT('Origin',(6.,0.,0.));
#52297=CARTESIAN_POINT('',(6.,11.5470739757602,-3.26574380475891));
#52298=CARTESIAN_POINT('Origin',(6.,13.8564064606,8.));
#52299=CARTESIAN_POINT('Origin',(6.,0.,0.));
#52300=CARTESIAN_POINT('Origin',(6.,0.,10.));
#52301=CARTESIAN_POINT('',(6.,-8.42733192529161,18.1378079331809));
#52302=CARTESIAN_POINT('',(6.,-2.94531989074286,11.632931304757));
#52303=CARTESIAN_POINT('Origin',(6.,-13.8564064606,8.));
#52304=CARTESIAN_POINT('',(6.,2.94531989074286,11.632931304757));
#52305=CARTESIAN_POINT('Origin',(6.,0.,0.));
#52306=CARTESIAN_POINT('',(6.,8.42733192529161,18.1378079331809));
#52307=CARTESIAN_POINT('Origin',(6.,13.8564064606,8.));
#52308=CARTESIAN_POINT('Origin',(6.,0.,0.));
#52309=CARTESIAN_POINT('Origin',(-1.,-13.8564064606,8.));
#52310=CARTESIAN_POINT('',(-8.,-11.5470739757602,-3.26574380475891));
#52311=CARTESIAN_POINT('',(-8.,-19.921468401738,-1.77062043322529));
#52312=CARTESIAN_POINT('Origin',(-8.,-13.8564064606,8.));
#52313=CARTESIAN_POINT('',(-1.,-19.921468401738,-1.77062043322529));
#52314=CARTESIAN_POINT('',(-1.,-11.5470739757602,-3.26574380475891));
#52315=CARTESIAN_POINT('Origin',(-1.,0.,0.));
#52316=CARTESIAN_POINT('',(-8.,-2.94531989074286,11.632931304757));
#52317=CARTESIAN_POINT('',(-1.,-2.94531989074286,11.632931304757));
#52318=CARTESIAN_POINT('',(-8.,2.94531989074286,11.632931304757));
#52319=CARTESIAN_POINT('Origin',(-8.,0.,0.));
#52320=CARTESIAN_POINT('',(-1.,2.94531989074286,11.632931304757));
#52321=CARTESIAN_POINT('Origin',(-1.,0.,0.));
#52322=CARTESIAN_POINT('',(-8.,11.5470739757602,-3.26574380475891));
#52323=CARTESIAN_POINT('',(-1.,11.5470739757602,-3.26574380475891));
#52324=CARTESIAN_POINT('',(-8.,8.60175408505985,-8.3671875));
#52325=CARTESIAN_POINT('Origin',(-8.,0.,0.));
#52326=CARTESIAN_POINT('',(-1.,8.60175408505985,-8.3671875));
#52327=CARTESIAN_POINT('Origin',(-1.,0.,0.));
#52328=CARTESIAN_POINT('',(-8.,-8.60175408505985,-8.3671875));
#52329=CARTESIAN_POINT('',(-1.,-8.60175408505985,-8.3671875));
#52330=CARTESIAN_POINT('Origin',(-8.,0.,0.));
#52331=CARTESIAN_POINT('Origin',(-1.,13.8564064606,8.));
#52332=CARTESIAN_POINT('',(-8.,19.921468401738,-1.77062043322529));
#52333=CARTESIAN_POINT('',(-1.,19.921468401738,-1.77062043322529));
#52334=CARTESIAN_POINT('Origin',(-8.,13.8564064606,8.));
#52335=CARTESIAN_POINT('Origin',(-1.,13.8564064606,8.));
#52336=CARTESIAN_POINT('',(-8.,8.42733192529161,18.1378079331809));
#52337=CARTESIAN_POINT('Origin',(-8.,13.8564064606,8.));
#52338=CARTESIAN_POINT('',(-1.,8.42733192529161,18.1378079331809));
#52339=CARTESIAN_POINT('Origin',(-8.,13.8564064606,8.));
#52340=CARTESIAN_POINT('',(-8.,-8.42733192529161,18.1378079331809));
#52341=CARTESIAN_POINT('Origin',(-8.,0.,0.));
#52342=CARTESIAN_POINT('',(-8.,-11.4941364764755,-16.3671875));
#52343=CARTESIAN_POINT('Origin',(-8.,0.,-16.));
#52344=CARTESIAN_POINT('',(-8.,-2.44929359829471E-15,-20.));
#52345=CARTESIAN_POINT('Origin',(-8.,0.,0.));
#52346=CARTESIAN_POINT('',(-8.,11.4941364764755,-16.3671875));
#52347=CARTESIAN_POINT('Origin',(-8.,0.,0.));
#52348=CARTESIAN_POINT('Origin',(-8.,0.,-16.));
#52349=CARTESIAN_POINT('Origin',(-8.,0.,0.));
#52350=CARTESIAN_POINT('Origin',(-8.,-13.8564064606,8.));
#52351=CARTESIAN_POINT('',(-8.,-1.5,-6.4));
#52352=CARTESIAN_POINT('',(-8.,-1.5,-4.76969600708473));
#52353=CARTESIAN_POINT('',(-8.,-1.5,2.4));
#52354=CARTESIAN_POINT('',(-8.,1.5,-4.76969600708473));
#52355=CARTESIAN_POINT('Origin',(-8.,0.,0.));
#52356=CARTESIAN_POINT('',(-8.,1.5,-6.4));
#52357=CARTESIAN_POINT('',(-8.,1.5,2.4));
#52358=CARTESIAN_POINT('',(-8.,6.9282032303,-6.4));
#52359=CARTESIAN_POINT('Origin',(-1.,0.,-16.));
#52360=CARTESIAN_POINT('',(-1.,-11.4941364764755,-16.3671875));
#52361=CARTESIAN_POINT('Origin',(-1.,0.,-16.));
#52362=CARTESIAN_POINT('',(-1.,11.4941364764755,-16.3671875));
#52363=CARTESIAN_POINT('Origin',(-1.,-13.8564064606,8.));
#52364=CARTESIAN_POINT('',(-1.,-8.42733192529161,18.1378079331809));
#52365=CARTESIAN_POINT('Origin',(-20.5,0.,0.));
#52366=CARTESIAN_POINT('',(-21.5303061543301,-1.5,-4.76969600708473));
#52367=CARTESIAN_POINT('',(-20.5,-1.5,-4.76969600708473));
#52368=CARTESIAN_POINT('',(-24.4696938456699,-1.5,-4.76969600708473));
#52369=CARTESIAN_POINT('Ctrl Pts',(-24.4696938456699,-1.5,-4.76969600708473));
#52370=CARTESIAN_POINT('Ctrl Pts',(-24.2875078566679,-1.67850508453567,
-4.71355875506578));
#52371=CARTESIAN_POINT('Ctrl Pts',(-24.0592673499683,-1.83355795563958,
-4.65305931877349));
#52372=CARTESIAN_POINT('Ctrl Pts',(-23.5501354824849,-2.04585962054866,
-4.56378013142765));
#52373=CARTESIAN_POINT('Ctrl Pts',(-23.2674916717861,-2.1,-4.53762052181537));
#52374=CARTESIAN_POINT('Ctrl Pts',(-23.,-2.1,-4.53762052181537));
#52375=CARTESIAN_POINT('Ctrl Pts',(-22.7325083282139,-2.1,-4.53762052181537));
#52376=CARTESIAN_POINT('Ctrl Pts',(-22.4498645175151,-2.04585962054866,
-4.56378013142765));
#52377=CARTESIAN_POINT('Ctrl Pts',(-21.9407326500317,-1.83355795563958,
-4.65305931877349));
#52378=CARTESIAN_POINT('Ctrl Pts',(-21.7124921433321,-1.67850508453567,
-4.71355875506578));
#52379=CARTESIAN_POINT('Ctrl Pts',(-21.5303061543301,-1.5,-4.76969600708473));
#52380=CARTESIAN_POINT('',(-20.5,-1.5,-4.76969600708473));
#52381=CARTESIAN_POINT('',(-24.4696938456699,1.5,-4.76969600708473));
#52382=CARTESIAN_POINT('',(-20.5,1.5,-4.76969600708473));
#52383=CARTESIAN_POINT('',(-21.5303061543301,1.5,-4.76969600708473));
#52384=CARTESIAN_POINT('Ctrl Pts',(-21.5303061543301,1.5,-4.76969600708473));
#52385=CARTESIAN_POINT('Ctrl Pts',(-21.7124921433321,1.67850508453567,-4.71355875506578));
#52386=CARTESIAN_POINT('Ctrl Pts',(-21.9407326500317,1.83355795563958,-4.65305931877349));
#52387=CARTESIAN_POINT('Ctrl Pts',(-22.4498645175151,2.04585962054866,-4.56378013142765));
#52388=CARTESIAN_POINT('Ctrl Pts',(-22.7325083282139,2.1,-4.53762052181537));
#52389=CARTESIAN_POINT('Ctrl Pts',(-23.2674916717861,2.1,-4.53762052181537));
#52390=CARTESIAN_POINT('Ctrl Pts',(-23.5501354824849,2.04585962054866,-4.56378013142765));
#52391=CARTESIAN_POINT('Ctrl Pts',(-24.0592673499683,1.83355795563958,-4.65305931877349));
#52392=CARTESIAN_POINT('Ctrl Pts',(-24.2875078566679,1.67850508453567,-4.71355875506578));
#52393=CARTESIAN_POINT('Ctrl Pts',(-24.4696938456699,1.5,-4.76969600708473));
#52394=CARTESIAN_POINT('',(-20.5,1.5,-4.76969600708473));
#52395=CARTESIAN_POINT('Origin',(-20.5,1.5,-3.2));
#52396=CARTESIAN_POINT('',(-21.5303061543301,1.5,-6.4));
#52397=CARTESIAN_POINT('',(-21.5303061543301,1.5,-5.58484800354236));
#52398=CARTESIAN_POINT('',(-20.5,1.5,-6.4));
#52399=CARTESIAN_POINT('Origin',(-20.5,1.5,-3.2));
#52400=CARTESIAN_POINT('',(-24.4696938456699,1.5,-6.4));
#52401=CARTESIAN_POINT('',(-24.4696938456699,1.5,-5.58484800354236));
#52402=CARTESIAN_POINT('',(-20.5,1.5,-6.4));
#52403=CARTESIAN_POINT('Origin',(-20.5,0.,-6.4));
#52404=CARTESIAN_POINT('',(-21.5303061543301,-1.5,-6.4));
#52405=CARTESIAN_POINT('Origin',(-23.,0.,-6.4));
#52406=CARTESIAN_POINT('',(-20.5,-1.5,-6.4));
#52407=CARTESIAN_POINT('Origin',(-20.5,0.,-6.4));
#52408=CARTESIAN_POINT('',(-25.1,2.57175827820944E-16,-6.4));
#52409=CARTESIAN_POINT('Origin',(-23.,0.,-6.4));
#52410=CARTESIAN_POINT('',(-24.4696938456699,-1.5,-6.4));
#52411=CARTESIAN_POINT('',(-20.5,-1.5,-6.4));
#52412=CARTESIAN_POINT('Origin',(-23.,0.,-6.4));
#52413=CARTESIAN_POINT('Origin',(-20.5,-1.5,-3.2));
#52414=CARTESIAN_POINT('',(-21.5303061543301,-1.5,-5.58484800354236));
#52415=CARTESIAN_POINT('Origin',(-20.5,-1.5,-3.2));
#52416=CARTESIAN_POINT('',(-24.4696938456699,-1.5,-5.58484800354236));
#52417=CARTESIAN_POINT('Origin',(-23.,0.,-10.));
#52418=CARTESIAN_POINT('',(-25.1,2.57175827820944E-16,-20.));
#52419=CARTESIAN_POINT('',(-25.1,2.57175827820944E-16,-10.));
#52420=CARTESIAN_POINT('',(-20.9,0.,-20.));
#52421=CARTESIAN_POINT('Ctrl Pts',(-20.9,4.16333634234434E-16,-20.));
#52422=CARTESIAN_POINT('Ctrl Pts',(-20.9,0.263888990751172,-20.));
#52423=CARTESIAN_POINT('Ctrl Pts',(-20.9527780741314,0.545235237847868,
-19.9942425936951));
#52424=CARTESIAN_POINT('Ctrl Pts',(-21.1671514943451,1.06257490219278,-19.97343117591));
#52425=CARTESIAN_POINT('Ctrl Pts',(-21.3287361087815,1.29858458976497,-19.9586721250997));
#52426=CARTESIAN_POINT('Ctrl Pts',(-21.7014161819223,1.67126466290584,-19.9309254589373));
#52427=CARTESIAN_POINT('Ctrl Pts',(-21.9374255317885,1.83284867450471,-19.9161307432363));
#52428=CARTESIAN_POINT('Ctrl Pts',(-22.4547640622183,2.04722164681422,-19.8952376620524));
#52429=CARTESIAN_POINT('Ctrl Pts',(-22.7361099164069,2.1,-19.8894444366855));
#52430=CARTESIAN_POINT('Ctrl Pts',(-23.2638900835931,2.1,-19.8894444366855));
#52431=CARTESIAN_POINT('Ctrl Pts',(-23.5452359377817,2.04722164681422,-19.8952376620524));
#52432=CARTESIAN_POINT('Ctrl Pts',(-24.0625744682115,1.83284867450471,-19.9161307432363));
#52433=CARTESIAN_POINT('Ctrl Pts',(-24.2985838180777,1.67126466290584,-19.9309254589373));
#52434=CARTESIAN_POINT('Ctrl Pts',(-24.6712638912185,1.29858458976497,-19.9586721250997));
#52435=CARTESIAN_POINT('Ctrl Pts',(-24.8328485056549,1.06257490219277,-19.97343117591));
#52436=CARTESIAN_POINT('Ctrl Pts',(-25.0472219258686,0.545235237847867,
-19.9942425936951));
#52437=CARTESIAN_POINT('Ctrl Pts',(-25.1,0.263888990751172,-20.));
#52438=CARTESIAN_POINT('Ctrl Pts',(-25.1,-6.93889390390723E-17,-20.));
#52439=CARTESIAN_POINT('',(-23.,-2.1,-19.8894444366855));
#52440=CARTESIAN_POINT('Ctrl Pts',(-23.,-2.1,-19.8894444366855));
#52441=CARTESIAN_POINT('Ctrl Pts',(-22.7361099164069,-2.1,-19.8894444366855));
#52442=CARTESIAN_POINT('Ctrl Pts',(-22.4547640622183,-2.04722164681422,
-19.8952376620524));
#52443=CARTESIAN_POINT('Ctrl Pts',(-21.9374255317885,-1.83284867450471,
-19.9161307432363));
#52444=CARTESIAN_POINT('Ctrl Pts',(-21.7014161819223,-1.67126466290584,
-19.9309254589373));
#52445=CARTESIAN_POINT('Ctrl Pts',(-21.3287361087815,-1.29858458976497,
-19.9586721250997));
#52446=CARTESIAN_POINT('Ctrl Pts',(-21.1671514943451,-1.06257490219277,
-19.97343117591));
#52447=CARTESIAN_POINT('Ctrl Pts',(-20.9527780741314,-0.545235237847867,
-19.9942425936951));
#52448=CARTESIAN_POINT('Ctrl Pts',(-20.9,-0.263888990751171,-20.));
#52449=CARTESIAN_POINT('Ctrl Pts',(-20.9,-5.20417042793042E-17,-20.));
#52450=CARTESIAN_POINT('Ctrl Pts',(-25.1,-3.46944695195361E-16,-20.));
#52451=CARTESIAN_POINT('Ctrl Pts',(-25.1,-0.263888990751172,-20.));
#52452=CARTESIAN_POINT('Ctrl Pts',(-25.0472219258686,-0.545235237847867,
-19.9942425936951));
#52453=CARTESIAN_POINT('Ctrl Pts',(-24.8328485056549,-1.06257490219277,
-19.97343117591));
#52454=CARTESIAN_POINT('Ctrl Pts',(-24.6712638912185,-1.29858458976497,
-19.9586721250997));
#52455=CARTESIAN_POINT('Ctrl Pts',(-24.2985838180777,-1.67126466290584,
-19.9309254589373));
#52456=CARTESIAN_POINT('Ctrl Pts',(-24.0625744682115,-1.83284867450471,
-19.9161307432363));
#52457=CARTESIAN_POINT('Ctrl Pts',(-23.5452359377817,-2.04722164681422,
-19.8952376620524));
#52458=CARTESIAN_POINT('Ctrl Pts',(-23.2638900835931,-2.1,-19.8894444366855));
#52459=CARTESIAN_POINT('Ctrl Pts',(-23.,-2.1,-19.8894444366855));
#52460=CARTESIAN_POINT('Origin',(-13.,0.,0.));
#52461=CARTESIAN_POINT('',(-13.,-2.44929359829471E-15,-20.));
#52462=CARTESIAN_POINT('',(-13.,-2.44929359829471E-15,-20.));
#52463=CARTESIAN_POINT('',(-4.3435534146,-2.1388888889,19.8852999555184));
#52464=CARTESIAN_POINT('',(-5.18767834635794,0.459060516890588,19.9947308919583));
#52465=CARTESIAN_POINT('Ctrl Pts',(-5.18767834635794,0.459060516890587,
19.9947308919583));
#52466=CARTESIAN_POINT('Ctrl Pts',(-5.24968129137097,0.414012740477042,
19.9957651472147));
#52467=CARTESIAN_POINT('Ctrl Pts',(-5.30716488138641,0.364591710747686,
19.9967442102515));
#52468=CARTESIAN_POINT('Ctrl Pts',(-5.48665323742873,0.185057927007366,
19.9995504652193));
#52469=CARTESIAN_POINT('Ctrl Pts',(-5.59715741138799,0.0235509943668747,
20.0007685496482));
#52470=CARTESIAN_POINT('Ctrl Pts',(-5.7436627884403,-0.330259044510279,
19.9980555602176));
#52471=CARTESIAN_POINT('Ctrl Pts',(-5.7796645257,-0.522560848653025,19.993985306904));
#52472=CARTESIAN_POINT('Ctrl Pts',(-5.7796645257,-0.883349185014401,19.9812997715422));
#52473=CARTESIAN_POINT('Ctrl Pts',(-5.74353603624199,-1.07581469312434,
19.971831595325));
#52474=CARTESIAN_POINT('Ctrl Pts',(-5.59681775573534,-1.4297140658822,19.9496203526915));
#52475=CARTESIAN_POINT('Ctrl Pts',(-5.48623409908571,-1.59115913013439,
19.9370154287515));
#52476=CARTESIAN_POINT('Ctrl Pts',(-5.23128841814184,-1.84591622773468,
19.9150423979699));
#52477=CARTESIAN_POINT('Ctrl Pts',(-5.06995436664432,-1.95632911293912,
19.9042256075891));
#52478=CARTESIAN_POINT('Ctrl Pts',(-4.71629161866783,-2.10281902804406,
19.8892828626319));
#52479=CARTESIAN_POINT('Ctrl Pts',(-4.52395392331701,-2.1388888889,19.8852999555184));
#52480=CARTESIAN_POINT('Ctrl Pts',(-4.3435534146,-2.1388888889,19.8852999555184));
#52481=CARTESIAN_POINT('',(-5.7631397208,2.1388888889,19.8852999555184));
#52482=CARTESIAN_POINT('Origin',(-5.03059422324816,0.0005165593435702,-2.33120559308216));
#52483=CARTESIAN_POINT('',(-4.7295794663,2.1388888889,19.8852999555184));
#52484=CARTESIAN_POINT('',(-5.24635959355,2.1388888889,19.8852999555184));
#52485=CARTESIAN_POINT('',(-4.2292347159,0.6783333333,19.9884932871123));
#52486=CARTESIAN_POINT('Origin',(-3.99709194624176,0.000685748014040422,
-2.32885472330861));
#52487=CARTESIAN_POINT('',(-3.7202200813,0.6783333333,19.9884932871123));
#52488=CARTESIAN_POINT('',(-3.9747273986,0.6783333333,19.9884932871123));
#52489=CARTESIAN_POINT('',(-3.7202200813,2.1388888889,19.8852999555184));
#52490=CARTESIAN_POINT('Origin',(-3.7202200813,0.,0.));
#52491=CARTESIAN_POINT('',(-2.7424423035,2.1388888889,19.8852999555184));
#52492=CARTESIAN_POINT('',(-3.2313311924,2.1388888889,19.8852999555184));
#52493=CARTESIAN_POINT('',(-2.7424423035,-2.1388888889,19.8852999555184));
#52494=CARTESIAN_POINT('Origin',(-2.7424423035,0.,0.));
#52495=CARTESIAN_POINT('',(-3.54299785905,-2.1388888889,19.8852999555184));
#52496=CARTESIAN_POINT('',(-1.4888888889,-1.1611111111,19.9662670769395));
#52497=CARTESIAN_POINT('',(-1.4888888889,2.1388888889,19.8852999555184));
#52498=CARTESIAN_POINT('Origin',(-1.4888888889,0.,0.));
#52499=CARTESIAN_POINT('',(-0.5111111111,2.1388888889,19.8852999555184));
#52500=CARTESIAN_POINT('',(-1.,2.1388888889,19.8852999555184));
#52501=CARTESIAN_POINT('',(-0.5111111111,-1.1611111111,19.9662670769395));
#52502=CARTESIAN_POINT('Origin',(-0.5111111111,0.,0.));
#52503=CARTESIAN_POINT('',(0.5277777778,-1.1611111111,19.9662670769395));
#52504=CARTESIAN_POINT('',(0.00833333335000042,-1.1611111111,19.9662670769395));
#52505=CARTESIAN_POINT('',(0.5277777778,-2.1388888889,19.8852999555184));
#52506=CARTESIAN_POINT('Origin',(0.527777777800001,0.,0.));
#52507=CARTESIAN_POINT('',(-2.5277777778,-2.1388888889,19.8852999555184));
#52508=CARTESIAN_POINT('',(-1.,-2.1388888889,19.8852999555184));
#52509=CARTESIAN_POINT('',(-2.5277777778,-1.1611111111,19.9662670769395));
#52510=CARTESIAN_POINT('Origin',(-2.5277777778,0.,0.));
#52511=CARTESIAN_POINT('',(-2.00833333335,-1.1611111111,19.9662670769395));
#52512=CARTESIAN_POINT('',(3.7631397208,2.75,19.8100353356575));
#52513=CARTESIAN_POINT('',(1.8075841652,2.75,19.8100353356575));
#52514=CARTESIAN_POINT('',(2.785361943,2.75,19.8100353356575));
#52515=CARTESIAN_POINT('',(-1.,4.3709594736,19.5165241085637));
#52516=CARTESIAN_POINT('Origin',(6.57072388981035,-2.27381335982102E-9,
-1.34364674941878E-8));
#52517=CARTESIAN_POINT('',(-3.8075841652,2.75,19.8100353356575));
#52518=CARTESIAN_POINT('Origin',(-8.5707238638722,1.26959015522843E-8,6.91637080940666E-8));
#52519=CARTESIAN_POINT('',(-5.7631397208,2.75,19.8100353356575));
#52520=CARTESIAN_POINT('',(-4.785361943,2.75,19.8100353356575));
#52521=CARTESIAN_POINT('',(-1.,5.5,19.2288845230294));
#52522=CARTESIAN_POINT('Origin',(-10.526279440744,4.94369545300799E-10,
2.25620633287349E-9));
#52523=CARTESIAN_POINT('Origin',(8.52627944326717,-9.62673274429449E-10,
-4.51972903547926E-9));
#52524=CARTESIAN_POINT('',(1.9747474276,-0.2016666667,19.9989832380434));
#52525=CARTESIAN_POINT('',(0.5561396937,2.1388888889,19.8852999555184));
#52526=CARTESIAN_POINT('Origin',(1.85251751839491,0.,0.));
#52527=CARTESIAN_POINT('',(1.6994942043,2.1388888889,19.8852999555184));
#52528=CARTESIAN_POINT('',(1.127816949,2.1388888889,19.8852999555184));
#52529=CARTESIAN_POINT('',(2.785361943,0.3473197978,19.9969839965445));
#52530=CARTESIAN_POINT('Origin',(2.99587202900023,0.,0.));
#52531=CARTESIAN_POINT('',(2.785361943,2.1388888889,19.8852999555184));
#52532=CARTESIAN_POINT('Origin',(2.785361943,0.,0.));
#52533=CARTESIAN_POINT('',(3.7631397208,2.1388888889,19.8852999555184));
#52534=CARTESIAN_POINT('',(3.2742508319,2.1388888889,19.8852999555184));
#52535=CARTESIAN_POINT('',(3.7631397208,-2.1388888889,19.8852999555184));
#52536=CARTESIAN_POINT('Origin',(3.7631397208,0.,0.));
#52537=CARTESIAN_POINT('',(2.785361943,-2.1388888889,19.8852999555184));
#52538=CARTESIAN_POINT('',(3.2742508319,-2.1388888889,19.8852999555184));
#52539=CARTESIAN_POINT('',(2.785361943,-0.7484330612,19.9859912927256));
#52540=CARTESIAN_POINT('Origin',(2.785361943,0.,0.));
#52541=CARTESIAN_POINT('',(1.8474876449,-2.1388888889,19.8852999555184));
#52542=CARTESIAN_POINT('Origin',(3.29018641707832,0.,0.));
#52543=CARTESIAN_POINT('',(0.6680745397,-2.1388888889,19.8852999555184));
#52544=CARTESIAN_POINT('',(1.2577810923,-2.1388888889,19.8852999555184));
#52545=CARTESIAN_POINT('Origin',(2.11077331185338,0.,0.));
#52546=CARTESIAN_POINT('',(-1.,-4.3709594736,19.5165241085637));
#52547=CARTESIAN_POINT('',(1.8075841652,-2.75,19.8100353356575));
#52548=CARTESIAN_POINT('Origin',(6.57072387874695,-4.11288225699025E-9,
2.09971195985759E-8));
#52549=CARTESIAN_POINT('',(3.7631397208,-2.75,19.8100353356575));
#52550=CARTESIAN_POINT('',(2.785361943,-2.75,19.8100353356575));
#52551=CARTESIAN_POINT('',(-1.,-5.5,19.2288845230294));
#52552=CARTESIAN_POINT('Origin',(8.52627944334428,1.00725594531781E-9,-4.7267834091258E-9));
#52553=CARTESIAN_POINT('',(-5.7631397208,-2.75,19.8100353356575));
#52554=CARTESIAN_POINT('Origin',(-10.5262794407692,-4.79505324335605E-10,
2.19413154312065E-9));
#52555=CARTESIAN_POINT('',(-3.8075841652,-2.75,19.8100353356575));
#52556=CARTESIAN_POINT('',(-4.785361943,-2.75,19.8100353356575));
#52557=CARTESIAN_POINT('Origin',(-8.57072386754017,-1.05836966968198E-8,
5.72841307722172E-8));
#52558=CARTESIAN_POINT('Origin',(-1.,0.,0.));
#52559=CARTESIAN_POINT('',(-1.4888888889,2.1388888889,19.3823413013222));
#52560=CARTESIAN_POINT('',(-1.4888888889,-1.1611111111,19.4654006120521));
#52561=CARTESIAN_POINT('Origin',(-1.4888888889,0.,0.));
#52562=CARTESIAN_POINT('',(-2.5277777778,-1.1611111111,19.4654006120521));
#52563=CARTESIAN_POINT('',(-2.00833333335,-1.1611111111,19.4654006120521));
#52564=CARTESIAN_POINT('',(-2.5277777778,-2.1388888889,19.3823413013222));
#52565=CARTESIAN_POINT('Origin',(-2.5277777778,0.,0.));
#52566=CARTESIAN_POINT('',(0.5277777778,-2.1388888889,19.3823413013222));
#52567=CARTESIAN_POINT('',(-1.,-2.1388888889,19.3823413013222));
#52568=CARTESIAN_POINT('',(0.5277777778,-1.1611111111,19.4654006120521));
#52569=CARTESIAN_POINT('Origin',(0.5277777778,0.,0.));
#52570=CARTESIAN_POINT('',(-0.5111111111,-1.1611111111,19.4654006120521));
#52571=CARTESIAN_POINT('',(0.00833333334999997,-1.1611111111,19.4654006120521));
#52572=CARTESIAN_POINT('',(-0.5111111111,2.1388888889,19.3823413013222));
#52573=CARTESIAN_POINT('Origin',(-0.5111111111,0.,0.));
#52574=CARTESIAN_POINT('',(-1.,2.1388888889,19.3823413013222));
#52575=CARTESIAN_POINT('Origin',(-0.5111111111,0.4888888889,0.));
#52576=CARTESIAN_POINT('',(-0.5111111111,2.1388888889,0.));
#52577=CARTESIAN_POINT('',(-0.5111111111,-1.1611111111,0.));
#52578=CARTESIAN_POINT('Origin',(-1.,2.1388888889,0.));
#52579=CARTESIAN_POINT('',(-1.4888888889,2.1388888889,0.));
#52580=CARTESIAN_POINT('Origin',(0.00833333334999997,-1.1611111111,0.));
#52581=CARTESIAN_POINT('',(0.5277777778,-1.1611111111,0.));
#52582=CARTESIAN_POINT('Origin',(0.5277777778,-1.65,0.));
#52583=CARTESIAN_POINT('',(0.5277777778,-2.1388888889,0.));
#52584=CARTESIAN_POINT('Origin',(-1.,-2.1388888889,0.));
#52585=CARTESIAN_POINT('',(-2.5277777778,-2.1388888889,0.));
#52586=CARTESIAN_POINT('Origin',(-2.5277777778,-1.65,0.));
#52587=CARTESIAN_POINT('',(-2.5277777778,-1.1611111111,0.));
#52588=CARTESIAN_POINT('Origin',(-2.00833333335,-1.1611111111,0.));
#52589=CARTESIAN_POINT('',(-1.4888888889,-1.1611111111,0.));
#52590=CARTESIAN_POINT('Origin',(-1.4888888889,0.4888888889,0.));
#52591=CARTESIAN_POINT('Origin',(2.24242807365,1.24310434335,0.));
#52592=CARTESIAN_POINT('',(1.6994942043,2.1388888889,19.3823413013222));
#52593=CARTESIAN_POINT('',(1.6994942043,2.1388888889,0.));
#52594=CARTESIAN_POINT('',(2.785361943,0.3473197978,19.4969066510064));
#52595=CARTESIAN_POINT('Origin',(2.99587202900024,0.,0.));
#52596=CARTESIAN_POINT('',(2.785361943,0.3473197978,0.));
#52597=CARTESIAN_POINT('Origin',(1.127816949,2.1388888889,0.));
#52598=CARTESIAN_POINT('',(0.5561396937,2.1388888889,19.3823413013222));
#52599=CARTESIAN_POINT('',(0.5561396937,2.1388888889,0.));
#52600=CARTESIAN_POINT('',(1.127816949,2.1388888889,19.3823413013222));
#52601=CARTESIAN_POINT('Origin',(1.26544356065,0.9686111111,0.));
#52602=CARTESIAN_POINT('',(1.9747474276,-0.2016666667,19.4989571658472));
#52603=CARTESIAN_POINT('',(1.9747474276,-0.2016666667,0.));
#52604=CARTESIAN_POINT('Origin',(1.85251751839491,0.,0.));
#52605=CARTESIAN_POINT('Origin',(1.2577810923,-2.1388888889,0.));
#52606=CARTESIAN_POINT('',(1.8474876449,-2.1388888889,19.3823413013222));
#52607=CARTESIAN_POINT('',(1.8474876449,-2.1388888889,0.));
#52608=CARTESIAN_POINT('',(0.6680745397,-2.1388888889,19.3823413013222));
#52609=CARTESIAN_POINT('',(1.2577810923,-2.1388888889,19.3823413013222));
#52610=CARTESIAN_POINT('',(0.6680745397,-2.1388888889,0.));
#52611=CARTESIAN_POINT('Origin',(2.31642479395,-1.44366097505,0.));
#52612=CARTESIAN_POINT('',(2.785361943,-0.7484330612,19.4856318335563));
#52613=CARTESIAN_POINT('',(2.785361943,-0.7484330612,0.));
#52614=CARTESIAN_POINT('Origin',(3.29018641707832,0.,0.));
#52615=CARTESIAN_POINT('Origin',(2.785361943,-1.44366097505,0.));
#52616=CARTESIAN_POINT('',(2.785361943,-2.1388888889,19.3823413013222));
#52617=CARTESIAN_POINT('',(2.785361943,-2.1388888889,0.));
#52618=CARTESIAN_POINT('Origin',(2.785361943,0.,0.));
#52619=CARTESIAN_POINT('Origin',(3.2742508319,-2.1388888889,0.));
#52620=CARTESIAN_POINT('',(3.7631397208,-2.1388888889,19.3823413013222));
#52621=CARTESIAN_POINT('',(3.7631397208,-2.1388888889,0.));
#52622=CARTESIAN_POINT('',(3.2742508319,-2.1388888889,19.3823413013222));
#52623=CARTESIAN_POINT('Origin',(3.7631397208,0.,0.));
#52624=CARTESIAN_POINT('',(3.7631397208,2.1388888889,19.3823413013222));
#52625=CARTESIAN_POINT('',(3.7631397208,2.1388888889,0.));
#52626=CARTESIAN_POINT('Origin',(3.7631397208,0.,0.));
#52627=CARTESIAN_POINT('Origin',(3.2742508319,2.1388888889,0.));
#52628=CARTESIAN_POINT('',(2.785361943,2.1388888889,19.3823413013222));
#52629=CARTESIAN_POINT('',(2.785361943,2.1388888889,0.));
#52630=CARTESIAN_POINT('',(3.2742508319,2.1388888889,19.3823413013222));
#52631=CARTESIAN_POINT('Origin',(2.785361943,1.24310434335,0.));
#52632=CARTESIAN_POINT('Origin',(2.785361943,0.,0.));
#52633=CARTESIAN_POINT('Origin',(1.32141098365,-1.1702777778,0.));
#52634=CARTESIAN_POINT('Origin',(2.11077331185338,0.,0.));
#52635=CARTESIAN_POINT('Origin',(-1.,0.,0.));
#52636=CARTESIAN_POINT('Origin',(-1.,0.,0.));
#52637=CARTESIAN_POINT('',(-1.,5.5,18.7082869338697));
#52638=CARTESIAN_POINT('',(-5.7631397208,2.75,19.305115902268));
#52639=CARTESIAN_POINT('Origin',(-10.5262794424987,-5.18419751571741E-10,
-2.36643593609642E-9));
#52640=CARTESIAN_POINT('',(-3.8075841652,2.75,19.305115902268));
#52641=CARTESIAN_POINT('',(-4.785361943,2.75,19.305115902268));
#52642=CARTESIAN_POINT('',(-1.,4.3709594736,19.0038078626402));
#52643=CARTESIAN_POINT('Origin',(-8.570723907158,-1.22962007242933E-8,-6.41915343102539E-8));
#52644=CARTESIAN_POINT('',(1.8075841652,2.75,19.305115902268));
#52645=CARTESIAN_POINT('Origin',(6.57072388594774,-4.93771690202038E-11,
-4.65181226871891E-10));
#52646=CARTESIAN_POINT('',(3.7631397208,2.75,19.305115902268));
#52647=CARTESIAN_POINT('',(2.785361943,2.75,19.305115902268));
#52648=CARTESIAN_POINT('Origin',(8.5262794404497,6.64190369370488E-10,3.11044967560292E-9));
#52649=CARTESIAN_POINT('Origin',(-2.4037920826,3.5604797368,0.));
#52650=CARTESIAN_POINT('',(-1.,4.3709594736,0.));
#52651=CARTESIAN_POINT('',(-3.8075841652,2.75,0.));
#52652=CARTESIAN_POINT('Origin',(0.4037920826,3.5604797368,0.));
#52653=CARTESIAN_POINT('',(1.8075841652,2.75,0.));
#52654=CARTESIAN_POINT('Origin',(-4.785361943,2.75,0.));
#52655=CARTESIAN_POINT('',(-5.7631397208,2.75,0.));
#52656=CARTESIAN_POINT('Origin',(-3.3815698604,4.125,0.));
#52657=CARTESIAN_POINT('',(-1.,5.5,0.));
#52658=CARTESIAN_POINT('Origin',(1.3815698604,4.125,0.));
#52659=CARTESIAN_POINT('',(3.7631397208,2.75,0.));
#52660=CARTESIAN_POINT('Origin',(2.785361943,2.75,0.));
#52661=CARTESIAN_POINT('Origin',(-4.785361943,-2.75,0.));
#52662=CARTESIAN_POINT('',(-5.7631397208,-2.75,19.305115902268));
#52663=CARTESIAN_POINT('',(-5.7631397208,-2.75,0.));
#52664=CARTESIAN_POINT('',(-3.8075841652,-2.75,19.305115902268));
#52665=CARTESIAN_POINT('',(-4.785361943,-2.75,19.305115902268));
#52666=CARTESIAN_POINT('',(-3.8075841652,-2.75,0.));
#52667=CARTESIAN_POINT('Origin',(-3.3815698604,-4.125,0.));
#52668=CARTESIAN_POINT('',(-1.,-5.5,18.7082869338697));
#52669=CARTESIAN_POINT('',(-1.,-5.5,0.));
#52670=CARTESIAN_POINT('Origin',(-10.5262794400813,-8.77110606367637E-10,
4.09533296164E-9));
#52671=CARTESIAN_POINT('Origin',(1.3815698604,-4.125,0.));
#52672=CARTESIAN_POINT('',(3.7631397208,-2.75,19.305115902268));
#52673=CARTESIAN_POINT('',(3.7631397208,-2.75,0.));
#52674=CARTESIAN_POINT('Origin',(8.52627944078166,-4.73031613879016E-10,
2.23582041769532E-9));
#52675=CARTESIAN_POINT('Origin',(2.785361943,-2.75,0.));
#52676=CARTESIAN_POINT('',(1.8075841652,-2.75,19.305115902268));
#52677=CARTESIAN_POINT('',(1.8075841652,-2.75,0.));
#52678=CARTESIAN_POINT('',(2.785361943,-2.75,19.305115902268));
#52679=CARTESIAN_POINT('Origin',(-2.4037920826,-3.5604797368,0.));
#52680=CARTESIAN_POINT('',(-1.,-4.3709594736,19.0038078626402));
#52681=CARTESIAN_POINT('Origin',(-8.57072389406941,4.73950212409591E-9,
-2.49748000058503E-8));
#52682=CARTESIAN_POINT('',(-1.,-4.3709594736,0.));
#52683=CARTESIAN_POINT('Origin',(0.4037920826,-3.5604797368,0.));
#52684=CARTESIAN_POINT('Origin',(6.57072389929174,7.75191022484023E-9,-4.058589020417E-8));
#52685=CARTESIAN_POINT('Origin',(-1.,0.,0.));
#52686=CARTESIAN_POINT('Origin',(-4.4794070911,1.4086111111,0.));
#52687=CARTESIAN_POINT('',(-4.7295794663,2.1388888889,19.3823413013222));
#52688=CARTESIAN_POINT('',(-4.7295794663,2.1388888889,0.));
#52689=CARTESIAN_POINT('',(-4.2292347159,0.6783333333,19.4881980667514));
#52690=CARTESIAN_POINT('Origin',(-3.99710417002144,0.000721430429313635,
-2.2697089266716));
#52691=CARTESIAN_POINT('',(-4.2292347159,0.6783333333,0.));
#52692=CARTESIAN_POINT('Origin',(-5.24635959355,2.1388888889,0.));
#52693=CARTESIAN_POINT('',(-5.7631397208,2.1388888889,19.3823413013222));
#52694=CARTESIAN_POINT('',(-5.7631397208,2.1388888889,0.));
#52695=CARTESIAN_POINT('',(-5.24635959355,2.1388888889,19.3823413013222));
#52696=CARTESIAN_POINT('Origin',(-5.47540903359635,1.29897470288934,0.));
#52697=CARTESIAN_POINT('',(-5.18767834635794,0.459060516890588,19.4945957496387));
#52698=CARTESIAN_POINT('',(-5.18767834635794,0.459060516890588,0.));
#52699=CARTESIAN_POINT('Origin',(-5.03060343765304,0.000543454432446466,
-2.27211957514992));
#52700=CARTESIAN_POINT('Origin',(-4.3435534146,-0.7027777778,0.));
#52701=CARTESIAN_POINT('',(-4.3435534146,-2.1388888889,19.3823413013222));
#52702=CARTESIAN_POINT('',(-4.3435534146,-2.1388888889,0.));
#52703=CARTESIAN_POINT('Ctrl Pts',(-4.3435534146,-2.1388888889,19.3823413013222));
#52704=CARTESIAN_POINT('Ctrl Pts',(-4.52395809426988,-2.1388888889,19.3823413013222));
#52705=CARTESIAN_POINT('Ctrl Pts',(-4.71629563622818,-2.10281731621556,
19.3864277949426));
#52706=CARTESIAN_POINT('Ctrl Pts',(-5.06994974058055,-1.95633107681449,
19.4017574464858));
#52707=CARTESIAN_POINT('Ctrl Pts',(-5.23127577915034,-1.84592395078976,
19.4128536921776));
#52708=CARTESIAN_POINT('Ctrl Pts',(-5.48621793448543,-1.59118019669263,
19.4353935671731));
#52709=CARTESIAN_POINT('Ctrl Pts',(-5.59680474635876,-1.42973736216137,
19.4483236475342));
#52710=CARTESIAN_POINT('Ctrl Pts',(-5.74353126970954,-1.07583427316188,
19.4711073706637));
#52711=CARTESIAN_POINT('Ctrl Pts',(-5.7796645257,-0.883362239425408,19.4808193953452));
#52712=CARTESIAN_POINT('Ctrl Pts',(-5.7796645257,-0.522566272387348,19.4938308937715));
#52713=CARTESIAN_POINT('Ctrl Pts',(-5.74366463353765,-0.330266483099083,
19.4980055699564));
#52714=CARTESIAN_POINT('Ctrl Pts',(-5.59716211486846,0.0235426180269262,
19.500788263579));
#52715=CARTESIAN_POINT('Ctrl Pts',(-5.48665892619763,0.185050560069143,
19.4995390181328));
#52716=CARTESIAN_POINT('Ctrl Pts',(-5.30716969365494,0.364587581151339,
19.4966607992451));
#52717=CARTESIAN_POINT('Ctrl Pts',(-5.24968384954062,0.414010881858001,
19.495656582549));
#52718=CARTESIAN_POINT('Ctrl Pts',(-5.18767834635794,0.459060516890588,
19.4945957496387));
#52719=CARTESIAN_POINT('Origin',(-3.54299785905,-2.1388888889,0.));
#52720=CARTESIAN_POINT('',(-2.7424423035,-2.1388888889,19.3823413013222));
#52721=CARTESIAN_POINT('',(-2.7424423035,-2.1388888889,0.));
#52722=CARTESIAN_POINT('',(-3.54299785905,-2.1388888889,19.3823413013222));
#52723=CARTESIAN_POINT('Origin',(-3.7202200813,-0.7027777778,0.));
#52724=CARTESIAN_POINT('',(-3.7202200813,-1.1061111111,19.468603396492));
#52725=CARTESIAN_POINT('',(-3.7202200813,-1.1061111111,0.));
#52726=CARTESIAN_POINT('',(-3.7202200813,-0.2994444445,19.497700711229));
#52727=CARTESIAN_POINT('Origin',(-3.7202200813,0.,0.));
#52728=CARTESIAN_POINT('',(-3.7202200813,-0.2994444445,0.));
#52729=CARTESIAN_POINT('Origin',(-4.03188674795,-1.1061111111,0.));
#52730=CARTESIAN_POINT('',(-4.3435534146,-1.1061111111,19.468603396492));
#52731=CARTESIAN_POINT('',(-4.3435534146,-1.1061111111,0.));
#52732=CARTESIAN_POINT('',(-4.03188674795,-1.1061111111,19.468603396492));
#52733=CARTESIAN_POINT('Origin',(-2.7424423035,0.,0.));
#52734=CARTESIAN_POINT('',(-2.7424423035,2.1388888889,19.3823413013222));
#52735=CARTESIAN_POINT('',(-2.7424423035,2.1388888889,0.));
#52736=CARTESIAN_POINT('Origin',(-2.7424423035,0.,0.));
#52737=CARTESIAN_POINT('Origin',(-3.2313311924,2.1388888889,0.));
#52738=CARTESIAN_POINT('',(-3.7202200813,2.1388888889,19.3823413013222));
#52739=CARTESIAN_POINT('',(-3.7202200813,2.1388888889,0.));
#52740=CARTESIAN_POINT('',(-3.2313311924,2.1388888889,19.3823413013222));
#52741=CARTESIAN_POINT('Origin',(-3.7202200813,1.4086111111,0.));
#52742=CARTESIAN_POINT('',(-3.7202200813,0.6783333333,19.4881980667514));
#52743=CARTESIAN_POINT('',(-3.7202200813,0.6783333333,0.));
#52744=CARTESIAN_POINT('Origin',(-3.7202200813,0.,0.));
#52745=CARTESIAN_POINT('Origin',(-3.9747273986,0.6783333333,0.));
#52746=CARTESIAN_POINT('',(-3.9747273986,0.6783333333,19.4881980667514));
#52747=CARTESIAN_POINT('Origin',(-4.3435534146,-0.7027777778,0.));
#52748=CARTESIAN_POINT('',(-4.3435534146,-0.2994444445,19.497700711229));
#52749=CARTESIAN_POINT('',(-4.3435534146,-0.2994444445,0.));
#52750=CARTESIAN_POINT('Ctrl Pts',(-4.3435534146,-1.1061111111,19.468603396492));
#52751=CARTESIAN_POINT('Ctrl Pts',(-4.39419814308983,-1.1061111111,19.468603396492));
#52752=CARTESIAN_POINT('Ctrl Pts',(-4.44821225425436,-1.0959892259289,19.4691867368818));
#52753=CARTESIAN_POINT('Ctrl Pts',(-4.54756315899303,-1.0548413233652,19.4714594820528));
#52754=CARTESIAN_POINT('Ctrl Pts',(-4.59290043242865,-1.02381583731486,
19.4731375157807));
#52755=CARTESIAN_POINT('Ctrl Pts',(-4.66452631029908,-0.952218736036693,
19.4767698957415));
#52756=CARTESIAN_POINT('Ctrl Pts',(-4.69557900256288,-0.906859343552727,
19.4789650772337));
#52757=CARTESIAN_POINT('Ctrl Pts',(-4.73675930343402,-0.807469845951887,
19.4833381841241));
#52758=CARTESIAN_POINT('Ctrl Pts',(-4.7468867479,-0.75343917779947,19.4855048515763));
#52759=CARTESIAN_POINT('Ctrl Pts',(-4.7468867479,-0.652145736281435,19.4891578288136));
#52760=CARTESIAN_POINT('Ctrl Pts',(-4.73676979677675,-0.598128620436881,
19.4908879558739));
#52761=CARTESIAN_POINT('Ctrl Pts',(-4.69560712746241,-0.498746523663012,
19.4936841838618));
#52762=CARTESIAN_POINT('Ctrl Pts',(-4.66456102115108,-0.453382021110974,
19.4947615621894));
#52763=CARTESIAN_POINT('Ctrl Pts',(-4.59293064696051,-0.381759433086016,
19.4962956016238));
#52764=CARTESIAN_POINT('Ctrl Pts',(-4.54757997199792,-0.350722506379112,
19.4968566012566));
#52765=CARTESIAN_POINT('Ctrl Pts',(-4.44821221942384,-0.309565004720403,
19.4975535161267));
#52766=CARTESIAN_POINT('Ctrl Pts',(-4.39419521514208,-0.2994444445,19.497700711229));
#52767=CARTESIAN_POINT('Ctrl Pts',(-4.3435534146,-0.2994444445,19.497700711229));
#52768=CARTESIAN_POINT('Origin',(-4.03188674795,-0.2994444445,0.));
#52769=CARTESIAN_POINT('',(-4.03188674795,-0.2994444445,19.497700711229));
#52770=CARTESIAN_POINT('Origin',(-1.,0.,0.));
#52771=CARTESIAN_POINT('',(0.,0.,0.));
#52772=CARTESIAN_POINT('',(0.,0.,0.));
#52773=CARTESIAN_POINT('',(0.,0.,0.));
#52774=CARTESIAN_POINT('',(0.,0.,0.));
#52775=CARTESIAN_POINT('',(0.,0.,0.));
#52776=CARTESIAN_POINT('',(0.,0.,0.));
#52777=CARTESIAN_POINT('',(0.,0.,0.));
#52778=CARTESIAN_POINT('',(0.,0.,0.));
#52779=CARTESIAN_POINT('Origin',(-3.43502884254442,-7.,13.4350288425444));
#52780=CARTESIAN_POINT('',(-3.43502884254442,7.,15.5350288425444));
#52781=CARTESIAN_POINT('Origin',(-3.43502884254442,7.,13.4350288425444));
#52782=CARTESIAN_POINT('',(-3.43502884254442,-7.,15.5350288425444));
#52783=CARTESIAN_POINT('',(-3.43502884254442,-7.,15.5350288425444));
#52784=CARTESIAN_POINT('Origin',(-3.43502884254442,-7.,13.4350288425444));
#52785=CARTESIAN_POINT('Origin',(10.,-7.,19.));
#52786=CARTESIAN_POINT('',(10.,7.,21.1));
#52787=CARTESIAN_POINT('Origin',(10.,7.,19.));
#52788=CARTESIAN_POINT('',(10.,-7.,21.1));
#52789=CARTESIAN_POINT('',(10.,-7.,21.1));
#52790=CARTESIAN_POINT('Origin',(10.,-7.,19.));
#52791=CARTESIAN_POINT('Origin',(23.4350288425443,-7.,13.4350288425445));
#52792=CARTESIAN_POINT('',(23.4350288425443,7.,15.5350288425445));
#52793=CARTESIAN_POINT('Origin',(23.4350288425443,7.,13.4350288425445));
#52794=CARTESIAN_POINT('',(23.4350288425443,-7.,15.5350288425445));
#52795=CARTESIAN_POINT('',(23.4350288425443,-7.,15.5350288425445));
#52796=CARTESIAN_POINT('Origin',(23.4350288425443,-7.,13.4350288425445));
#52797=CARTESIAN_POINT('Origin',(-3.43502884254442,-7.,-13.4350288425444));
#52798=CARTESIAN_POINT('',(-3.43502884254442,7.,-11.3350288425444));
#52799=CARTESIAN_POINT('Origin',(-3.43502884254442,7.,-13.4350288425444));
#52800=CARTESIAN_POINT('',(-3.43502884254442,-7.,-11.3350288425444));
#52801=CARTESIAN_POINT('',(-3.43502884254442,-7.,-11.3350288425444));
#52802=CARTESIAN_POINT('Origin',(-3.43502884254442,-7.,-13.4350288425444));
#52803=CARTESIAN_POINT('Origin',(10.,-7.,-19.));
#52804=CARTESIAN_POINT('',(10.,7.,-16.9));
#52805=CARTESIAN_POINT('Origin',(10.,7.,-19.));
#52806=CARTESIAN_POINT('',(10.,-7.,-16.9));
#52807=CARTESIAN_POINT('',(10.,-7.,-16.9));
#52808=CARTESIAN_POINT('Origin',(10.,-7.,-19.));
#52809=CARTESIAN_POINT('Origin',(23.4350288425443,-7.,-13.4350288425445));
#52810=CARTESIAN_POINT('',(23.4350288425443,7.,-11.3350288425445));
#52811=CARTESIAN_POINT('Origin',(23.4350288425443,7.,-13.4350288425445));
#52812=CARTESIAN_POINT('',(23.4350288425443,-7.,-11.3350288425445));
#52813=CARTESIAN_POINT('',(23.4350288425443,-7.,-11.3350288425445));
#52814=CARTESIAN_POINT('Origin',(23.4350288425443,-7.,-13.4350288425445));
#52815=CARTESIAN_POINT('Origin',(10.,7.,0.));
#52816=CARTESIAN_POINT('',(10.,7.,14.));
#52817=CARTESIAN_POINT('Origin',(10.,7.,0.));
#52818=CARTESIAN_POINT('',(10.,-7.,14.));
#52819=CARTESIAN_POINT('',(10.,7.,14.));
#52820=CARTESIAN_POINT('Origin',(10.,-7.,0.));
#52821=CARTESIAN_POINT('Origin',(-32.,-7.,35.));
#52822=CARTESIAN_POINT('',(32.,-7.,25.));
#52823=CARTESIAN_POINT('',(32.,-7.,-25.));
#52824=CARTESIAN_POINT('',(32.,-7.,35.));
#52825=CARTESIAN_POINT('',(22.,-7.,35.));
#52826=CARTESIAN_POINT('Origin',(22.,-7.,25.));
#52827=CARTESIAN_POINT('',(-32.,-7.,35.));
#52828=CARTESIAN_POINT('',(-32.,-7.,35.));
#52829=CARTESIAN_POINT('',(-32.,-7.,-35.));
#52830=CARTESIAN_POINT('',(-32.,-7.,35.));
#52831=CARTESIAN_POINT('',(22.,-7.,-35.));
#52832=CARTESIAN_POINT('',(-32.,-7.,-35.));
#52833=CARTESIAN_POINT('Origin',(22.,-7.,-25.));
#52834=CARTESIAN_POINT('Origin',(32.,-7.,35.));
#52835=CARTESIAN_POINT('',(32.,7.,25.));
#52836=CARTESIAN_POINT('',(32.,7.,-25.));
#52837=CARTESIAN_POINT('',(32.,7.,35.));
#52838=CARTESIAN_POINT('',(32.,-7.,25.));
#52839=CARTESIAN_POINT('',(32.,7.,-25.));
#52840=CARTESIAN_POINT('Origin',(-32.,7.,35.));
#52841=CARTESIAN_POINT('',(22.,7.,35.));
#52842=CARTESIAN_POINT('',(-32.,7.,35.));
#52843=CARTESIAN_POINT('',(-32.,7.,35.));
#52844=CARTESIAN_POINT('Origin',(22.,7.,25.));
#52845=CARTESIAN_POINT('',(22.,7.,-35.));
#52846=CARTESIAN_POINT('Origin',(22.,7.,-25.));
#52847=CARTESIAN_POINT('',(-32.,7.,-35.));
#52848=CARTESIAN_POINT('',(-32.,7.,-35.));
#52849=CARTESIAN_POINT('',(-32.,7.,35.));
#52850=CARTESIAN_POINT('Origin',(-32.,-7.,35.));
#52851=CARTESIAN_POINT('',(-32.,-7.,-35.));
#52852=CARTESIAN_POINT('',(-32.,-7.,35.));
#52853=CARTESIAN_POINT('Origin',(0.,0.,35.));
#52854=CARTESIAN_POINT('',(22.,0.,35.));
#52855=CARTESIAN_POINT('Origin',(0.,0.,-35.));
#52856=CARTESIAN_POINT('',(22.,-7.,-35.));
#52857=CARTESIAN_POINT('Origin',(22.,0.,25.));
#52858=CARTESIAN_POINT('Origin',(22.,-7.,-25.));
#52859=CARTESIAN_POINT('',(0.,0.,0.));
#52860=CARTESIAN_POINT('Origin',(-14.,25.,5.));
#52861=CARTESIAN_POINT('',(-17.,25.,-5.));
#52862=CARTESIAN_POINT('Origin',(-14.,25.,-5.));
#52863=CARTESIAN_POINT('',(-17.,25.,5.));
#52864=CARTESIAN_POINT('',(-17.,25.,5.));
#52865=CARTESIAN_POINT('Origin',(-14.,25.,5.));
#52866=CARTESIAN_POINT('Origin',(14.,-25.,5.));
#52867=CARTESIAN_POINT('',(11.,-25.,-5.));
#52868=CARTESIAN_POINT('Origin',(14.,-25.,-5.));
#52869=CARTESIAN_POINT('',(11.,-25.,5.));
#52870=CARTESIAN_POINT('',(11.,-25.,5.));
#52871=CARTESIAN_POINT('Origin',(14.,-25.,5.));
#52872=CARTESIAN_POINT('Origin',(34.,25.,5.));
#52873=CARTESIAN_POINT('',(30.7,25.,-5.));
#52874=CARTESIAN_POINT('Origin',(34.,25.,-5.));
#52875=CARTESIAN_POINT('',(30.7,25.,5.));
#52876=CARTESIAN_POINT('',(30.7,25.,5.));
#52877=CARTESIAN_POINT('Origin',(34.,25.,5.));
#52878=CARTESIAN_POINT('Origin',(-34.,25.,5.));
#52879=CARTESIAN_POINT('',(-37.3,25.,-5.));
#52880=CARTESIAN_POINT('Origin',(-34.,25.,-5.));
#52881=CARTESIAN_POINT('',(-37.3,25.,5.));
#52882=CARTESIAN_POINT('',(-37.3,25.,5.));
#52883=CARTESIAN_POINT('Origin',(-34.,25.,5.));
#52884=CARTESIAN_POINT('Origin',(-34.,-25.,5.));
#52885=CARTESIAN_POINT('',(-37.3,-25.,-5.));
#52886=CARTESIAN_POINT('Origin',(-34.,-25.,-5.));
#52887=CARTESIAN_POINT('',(-37.3,-25.,5.));
#52888=CARTESIAN_POINT('',(-37.3,-25.,5.));
#52889=CARTESIAN_POINT('Origin',(-34.,-25.,5.));
#52890=CARTESIAN_POINT('Origin',(34.,-25.,5.));
#52891=CARTESIAN_POINT('',(30.7,-25.,-5.));
#52892=CARTESIAN_POINT('Origin',(34.,-25.,-5.));
#52893=CARTESIAN_POINT('',(30.7,-25.,5.));
#52894=CARTESIAN_POINT('',(30.7,-25.,5.));
#52895=CARTESIAN_POINT('Origin',(34.,-25.,5.));
#52896=CARTESIAN_POINT('Origin',(47.5,37.5,5.));
#52897=CARTESIAN_POINT('',(47.5,-37.5,-5.));
#52898=CARTESIAN_POINT('',(47.5,37.5,-5.));
#52899=CARTESIAN_POINT('',(47.5,37.5,-5.));
#52900=CARTESIAN_POINT('',(47.5,37.5,5.));
#52901=CARTESIAN_POINT('',(47.5,37.5,5.));
#52902=CARTESIAN_POINT('',(47.5,-37.5,5.));
#52903=CARTESIAN_POINT('',(47.5,37.5,5.));
#52904=CARTESIAN_POINT('',(47.5,-37.5,5.));
#52905=CARTESIAN_POINT('Origin',(-47.5,37.5,5.));
#52906=CARTESIAN_POINT('',(-47.5,37.5,-5.));
#52907=CARTESIAN_POINT('',(-47.5,37.5,-5.));
#52908=CARTESIAN_POINT('',(-47.5,37.5,5.));
#52909=CARTESIAN_POINT('',(-47.5,37.5,5.));
#52910=CARTESIAN_POINT('',(-47.5,37.5,5.));
#52911=CARTESIAN_POINT('Origin',(-47.5,37.5,5.));
#52912=CARTESIAN_POINT('',(-47.5,-37.5,-5.));
#52913=CARTESIAN_POINT('',(-47.5,37.5,-5.));
#52914=CARTESIAN_POINT('',(-47.5,-37.5,5.));
#52915=CARTESIAN_POINT('',(-47.5,-37.5,5.));
#52916=CARTESIAN_POINT('',(-47.5,37.5,5.));
#52917=CARTESIAN_POINT('Origin',(-47.5,-37.5,5.));
#52918=CARTESIAN_POINT('',(-47.5,-37.5,-5.));
#52919=CARTESIAN_POINT('',(-47.5,-37.5,5.));
#52920=CARTESIAN_POINT('Origin',(0.,0.,5.));
#52921=CARTESIAN_POINT('Origin',(0.,0.,-5.));
#52922=CARTESIAN_POINT('',(0.,0.,0.));
#52923=CARTESIAN_POINT('',(-37.,1.38777878078145E-14,4.73545521495571E-16));
#52924=CARTESIAN_POINT('',(0.,0.,0.));
#52925=CARTESIAN_POINT('Origin',(34.,25.,2.5));
#52926=CARTESIAN_POINT('',(30.7,25.,-2.5));
#52927=CARTESIAN_POINT('Origin',(34.,25.,-2.5));
#52928=CARTESIAN_POINT('',(30.7,25.,2.5));
#52929=CARTESIAN_POINT('',(30.7,25.,2.5));
#52930=CARTESIAN_POINT('Origin',(34.,25.,2.5));
#52931=CARTESIAN_POINT('Origin',(-34.,25.,2.5));
#52932=CARTESIAN_POINT('',(-37.3,25.,-2.5));
#52933=CARTESIAN_POINT('Origin',(-34.,25.,-2.5));
#52934=CARTESIAN_POINT('',(-37.3,25.,2.5));
#52935=CARTESIAN_POINT('',(-37.3,25.,2.5));
#52936=CARTESIAN_POINT('Origin',(-34.,25.,2.5));
#52937=CARTESIAN_POINT('Origin',(-34.,-25.,2.5));
#52938=CARTESIAN_POINT('',(-37.3,-25.,-2.5));
#52939=CARTESIAN_POINT('Origin',(-34.,-25.,-2.5));
#52940=CARTESIAN_POINT('',(-37.3,-25.,2.5));
#52941=CARTESIAN_POINT('',(-37.3,-25.,2.5));
#52942=CARTESIAN_POINT('Origin',(-34.,-25.,2.5));
#52943=CARTESIAN_POINT('Origin',(34.,-25.,2.5));
#52944=CARTESIAN_POINT('',(30.7,-25.,-2.5));
#52945=CARTESIAN_POINT('Origin',(34.,-25.,-2.5));
#52946=CARTESIAN_POINT('',(30.7,-25.,2.5));
#52947=CARTESIAN_POINT('',(30.7,-25.,2.5));
#52948=CARTESIAN_POINT('Origin',(34.,-25.,2.5));
#52949=CARTESIAN_POINT('Origin',(-14.,25.,2.5));
#52950=CARTESIAN_POINT('',(-17.3,25.,-2.5));
#52951=CARTESIAN_POINT('Origin',(-14.,25.,-2.5));
#52952=CARTESIAN_POINT('',(-17.3,25.,2.5));
#52953=CARTESIAN_POINT('',(-17.3,25.,2.5));
#52954=CARTESIAN_POINT('Origin',(-14.,25.,2.5));
#52955=CARTESIAN_POINT('Origin',(14.,-25.,2.5));
#52956=CARTESIAN_POINT('',(10.7,-25.,-2.5));
#52957=CARTESIAN_POINT('Origin',(14.,-25.,-2.5));
#52958=CARTESIAN_POINT('',(10.7,-25.,2.5));
#52959=CARTESIAN_POINT('',(10.7,-25.,2.5));
#52960=CARTESIAN_POINT('Origin',(14.,-25.,2.5));
#52961=CARTESIAN_POINT('Origin',(47.5,37.5,2.5));
#52962=CARTESIAN_POINT('',(47.5,-37.5,-2.5));
#52963=CARTESIAN_POINT('',(47.5,37.5,-2.5));
#52964=CARTESIAN_POINT('',(47.5,37.5,-2.5));
#52965=CARTESIAN_POINT('',(47.5,37.5,2.5));
#52966=CARTESIAN_POINT('',(47.5,37.5,2.5));
#52967=CARTESIAN_POINT('',(47.5,-37.5,2.5));
#52968=CARTESIAN_POINT('',(47.5,37.5,2.5));
#52969=CARTESIAN_POINT('',(47.5,-37.5,2.5));
#52970=CARTESIAN_POINT('Origin',(-47.5,37.5,2.5));
#52971=CARTESIAN_POINT('',(-47.5,37.5,-2.5));
#52972=CARTESIAN_POINT('',(-47.5,37.5,-2.5));
#52973=CARTESIAN_POINT('',(-47.5,37.5,2.5));
#52974=CARTESIAN_POINT('',(-47.5,37.5,2.5));
#52975=CARTESIAN_POINT('',(-47.5,37.5,2.5));
#52976=CARTESIAN_POINT('Origin',(-47.5,37.5,2.5));
#52977=CARTESIAN_POINT('',(-47.5,-37.5,-2.5));
#52978=CARTESIAN_POINT('',(-47.5,37.5,-2.5));
#52979=CARTESIAN_POINT('',(-47.5,-37.5,2.5));
#52980=CARTESIAN_POINT('',(-47.5,-37.5,2.5));
#52981=CARTESIAN_POINT('',(-47.5,37.5,2.5));
#52982=CARTESIAN_POINT('Origin',(-47.5,-37.5,2.5));
#52983=CARTESIAN_POINT('',(-47.5,-37.5,-2.5));
#52984=CARTESIAN_POINT('',(-47.5,-37.5,2.5));
#52985=CARTESIAN_POINT('Origin',(0.,0.,2.5));
#52986=CARTESIAN_POINT('Origin',(0.,0.,-2.5));
#52987=CARTESIAN_POINT('',(0.,0.,0.));
#52988=CARTESIAN_POINT('Origin',(-113.,125.,4.48054292080867E-14));
#52989=CARTESIAN_POINT('',(-113.,115.,-41.));
#52990=CARTESIAN_POINT('',(-113.,115.,-6.));
#52991=CARTESIAN_POINT('',(-113.,115.,4.48054292080867E-14));
#52992=CARTESIAN_POINT('',(-113.,125.,-41.));
#52993=CARTESIAN_POINT('',(-113.,125.,-41.));
#52994=CARTESIAN_POINT('',(-113.,125.,-6.));
#52995=CARTESIAN_POINT('',(-113.,125.,4.48054292080867E-14));
#52996=CARTESIAN_POINT('',(-113.,125.,-6.));
#52997=CARTESIAN_POINT('Origin',(2.4027149321267,125.,-8.54298642533938));
#52998=CARTESIAN_POINT('',(-273.,115.,-86.));
#52999=CARTESIAN_POINT('',(2.4027149321267,115.,-8.54298642533938));
#53000=CARTESIAN_POINT('',(-273.,125.,-86.));
#53001=CARTESIAN_POINT('',(-273.,125.,-86.));
#53002=CARTESIAN_POINT('',(2.4027149321267,125.,-8.54298642533938));
#53003=CARTESIAN_POINT('Origin',(0.,125.,-86.));
#53004=CARTESIAN_POINT('',(-308.,115.,-86.));
#53005=CARTESIAN_POINT('',(0.,115.,-86.));
#53006=CARTESIAN_POINT('',(-308.,125.,-86.));
#53007=CARTESIAN_POINT('',(-308.,125.,-86.));
#53008=CARTESIAN_POINT('',(0.,125.,-86.));
#53009=CARTESIAN_POINT('Origin',(-308.,125.,0.));
#53010=CARTESIAN_POINT('',(-308.,115.,-6.));
#53011=CARTESIAN_POINT('',(-308.,115.,0.));
#53012=CARTESIAN_POINT('',(-308.,125.,-6.));
#53013=CARTESIAN_POINT('',(-308.,125.,-6.));
#53014=CARTESIAN_POINT('',(-308.,125.,0.));
#53015=CARTESIAN_POINT('Origin',(0.,125.,-6.));
#53016=CARTESIAN_POINT('',(0.,115.,-6.));
#53017=CARTESIAN_POINT('',(0.,125.,-6.));
#53018=CARTESIAN_POINT('Origin',(0.,125.,0.));
#53019=CARTESIAN_POINT('Origin',(0.,115.,0.));
#53020=CARTESIAN_POINT('Origin',(-113.,-125.,4.48054292080867E-14));
#53021=CARTESIAN_POINT('',(-113.,-115.,-41.));
#53022=CARTESIAN_POINT('',(-113.,-115.,-6.));
#53023=CARTESIAN_POINT('',(-113.,-115.,4.48054292080867E-14));
#53024=CARTESIAN_POINT('',(-113.,-125.,-6.));
#53025=CARTESIAN_POINT('',(-113.,-125.,-6.));
#53026=CARTESIAN_POINT('',(-113.,-125.,-41.));
#53027=CARTESIAN_POINT('',(-113.,-125.,4.48054292080867E-14));
#53028=CARTESIAN_POINT('',(-113.,-125.,-41.));
#53029=CARTESIAN_POINT('Origin',(2.4027149321267,-125.,-8.54298642533938));
#53030=CARTESIAN_POINT('',(-273.,-115.,-86.));
#53031=CARTESIAN_POINT('',(2.4027149321267,-115.,-8.54298642533938));
#53032=CARTESIAN_POINT('',(-273.,-125.,-86.));
#53033=CARTESIAN_POINT('',(2.4027149321267,-125.,-8.54298642533938));
#53034=CARTESIAN_POINT('',(-273.,-125.,-86.));
#53035=CARTESIAN_POINT('Origin',(0.,-125.,-86.));
#53036=CARTESIAN_POINT('',(-308.,-115.,-86.));
#53037=CARTESIAN_POINT('',(0.,-115.,-86.));
#53038=CARTESIAN_POINT('',(-308.,-125.,-86.));
#53039=CARTESIAN_POINT('',(0.,-125.,-86.));
#53040=CARTESIAN_POINT('',(-308.,-125.,-86.));
#53041=CARTESIAN_POINT('Origin',(-308.,-125.,0.));
#53042=CARTESIAN_POINT('',(-308.,-115.,-6.));
#53043=CARTESIAN_POINT('',(-308.,-115.,0.));
#53044=CARTESIAN_POINT('',(-308.,-125.,-6.));
#53045=CARTESIAN_POINT('',(-308.,-125.,0.));
#53046=CARTESIAN_POINT('',(-308.,-125.,-6.));
#53047=CARTESIAN_POINT('Origin',(0.,-125.,-6.));
#53048=CARTESIAN_POINT('',(0.,-115.,-6.));
#53049=CARTESIAN_POINT('',(0.,-125.,-6.));
#53050=CARTESIAN_POINT('Origin',(0.,-125.,0.));
#53051=CARTESIAN_POINT('Origin',(0.,-115.,0.));
#53052=CARTESIAN_POINT('Origin',(2.5,2.75545529808155E-15,110.001));
#53053=CARTESIAN_POINT('',(2.50000000000002,55.,6.00000000000001));
#53054=CARTESIAN_POINT('',(2.50000000000001,-55.,6.00000000000001));
#53055=CARTESIAN_POINT('Origin',(2.5,2.75545529808155E-15,6.00000000000001));
#53056=CARTESIAN_POINT('',(2.50000000000001,-55.,-6.));
#53057=CARTESIAN_POINT('',(2.50000000000001,-55.,110.001));
#53058=CARTESIAN_POINT('',(2.50000000000002,55.,-6.));
#53059=CARTESIAN_POINT('Origin',(2.5,2.75545529808155E-15,-6.));
#53060=CARTESIAN_POINT('',(2.50000000000002,55.,110.001));
#53061=CARTESIAN_POINT('Origin',(-50.,47.5,6.));
#53062=CARTESIAN_POINT('',(-53.4,47.5,-6.));
#53063=CARTESIAN_POINT('Origin',(-50.,47.5,-6.));
#53064=CARTESIAN_POINT('',(-53.4,47.5,6.));
#53065=CARTESIAN_POINT('',(-53.4,47.5,6.));
#53066=CARTESIAN_POINT('Origin',(-50.,47.5,6.));
#53067=CARTESIAN_POINT('Origin',(70.,47.5,6.));
#53068=CARTESIAN_POINT('',(66.6,47.5,-6.));
#53069=CARTESIAN_POINT('Origin',(70.,47.5,-6.));
#53070=CARTESIAN_POINT('',(66.6,47.5,6.));
#53071=CARTESIAN_POINT('',(66.6,47.5,6.));
#53072=CARTESIAN_POINT('Origin',(70.,47.5,6.));
#53073=CARTESIAN_POINT('Origin',(70.,-47.5,6.));
#53074=CARTESIAN_POINT('',(66.6,-47.5,-6.));
#53075=CARTESIAN_POINT('Origin',(70.,-47.5,-6.));
#53076=CARTESIAN_POINT('',(66.6,-47.5,6.));
#53077=CARTESIAN_POINT('',(66.6,-47.5,6.));
#53078=CARTESIAN_POINT('Origin',(70.,-47.5,6.));
#53079=CARTESIAN_POINT('Origin',(-50.,-47.5,6.));
#53080=CARTESIAN_POINT('',(-53.4,-47.5,-6.));
#53081=CARTESIAN_POINT('Origin',(-50.,-47.5,-6.));
#53082=CARTESIAN_POINT('',(-53.4,-47.5,6.));
#53083=CARTESIAN_POINT('',(-53.4,-47.5,6.));
#53084=CARTESIAN_POINT('Origin',(-50.,-47.5,6.));
#53085=CARTESIAN_POINT('Origin',(-248.336309447889,58.3363094478911,6.));
#53086=CARTESIAN_POINT('',(-252.586309447889,58.3363094478911,-6.));
#53087=CARTESIAN_POINT('Origin',(-248.336309447889,58.3363094478911,-6.));
#53088=CARTESIAN_POINT('',(-252.586309447889,58.3363094478911,6.));
#53089=CARTESIAN_POINT('',(-252.586309447889,58.3363094478911,6.));
#53090=CARTESIAN_POINT('Origin',(-248.336309447889,58.3363094478911,6.));
#53091=CARTESIAN_POINT('Origin',(-248.33630944789,-58.3363094478899,6.));
#53092=CARTESIAN_POINT('',(-252.58630944789,-58.3363094478899,-6.));
#53093=CARTESIAN_POINT('Origin',(-248.33630944789,-58.3363094478899,-6.));
#53094=CARTESIAN_POINT('',(-252.58630944789,-58.3363094478899,6.));
#53095=CARTESIAN_POINT('',(-252.58630944789,-58.3363094478899,6.));
#53096=CARTESIAN_POINT('Origin',(-248.33630944789,-58.3363094478899,6.));
#53097=CARTESIAN_POINT('Origin',(-131.66369055211,-58.3363094478907,6.));
#53098=CARTESIAN_POINT('',(-135.91369055211,-58.3363094478907,-6.));
#53099=CARTESIAN_POINT('Origin',(-131.66369055211,-58.3363094478907,-6.));
#53100=CARTESIAN_POINT('',(-135.91369055211,-58.3363094478907,6.));
#53101=CARTESIAN_POINT('',(-135.91369055211,-58.3363094478907,6.));
#53102=CARTESIAN_POINT('Origin',(-131.66369055211,-58.3363094478907,6.));
#53103=CARTESIAN_POINT('Origin',(-131.66369055211,58.3363094478899,6.));
#53104=CARTESIAN_POINT('',(-135.91369055211,58.3363094478899,-6.));
#53105=CARTESIAN_POINT('Origin',(-131.66369055211,58.3363094478899,-6.));
#53106=CARTESIAN_POINT('',(-135.91369055211,58.3363094478899,6.));
#53107=CARTESIAN_POINT('',(-135.91369055211,58.3363094478899,6.));
#53108=CARTESIAN_POINT('Origin',(-131.66369055211,58.3363094478899,6.));
#53109=CARTESIAN_POINT('Origin',(-190.,0.,-110.));
#53110=CARTESIAN_POINT('',(-235.,-5.51091059616309E-15,-6.));
#53111=CARTESIAN_POINT('Origin',(-190.,0.,-6.00000000000001));
#53112=CARTESIAN_POINT('',(-235.,-5.51091059616309E-15,0.999999999999996));
#53113=CARTESIAN_POINT('',(-235.,-5.51091059616309E-15,-110.));
#53114=CARTESIAN_POINT('Origin',(-190.,0.,1.));
#53115=CARTESIAN_POINT('Origin',(-190.,0.,1.));
#53116=CARTESIAN_POINT('',(-255.,-7.9602041944578E-15,1.));
#53117=CARTESIAN_POINT('Origin',(-190.,0.,1.));
#53118=CARTESIAN_POINT('',(-255.,-7.9602041944578E-15,6.));
#53119=CARTESIAN_POINT('',(-255.,-7.9602041944578E-15,1.));
#53120=CARTESIAN_POINT('Origin',(-190.,0.,6.));
#53121=CARTESIAN_POINT('Origin',(-320.,13.9999999999999,-25.));
#53122=CARTESIAN_POINT('',(-308.,13.9999999999999,-28.));
#53123=CARTESIAN_POINT('Origin',(-308.,13.9999999999999,-25.));
#53124=CARTESIAN_POINT('',(-320.,13.9999999999999,-28.));
#53125=CARTESIAN_POINT('',(-320.,13.9999999999999,-28.));
#53126=CARTESIAN_POINT('Origin',(-320.,13.9999999999999,-25.));
#53127=CARTESIAN_POINT('Origin',(-320.,-14.0000000000001,25.));
#53128=CARTESIAN_POINT('',(-308.,-14.0000000000001,22.));
#53129=CARTESIAN_POINT('Origin',(-308.,-14.0000000000001,25.));
#53130=CARTESIAN_POINT('',(-320.,-14.0000000000001,22.));
#53131=CARTESIAN_POINT('',(-320.,-14.0000000000001,22.));
#53132=CARTESIAN_POINT('Origin',(-320.,-14.0000000000001,25.));
#53133=CARTESIAN_POINT('Origin',(-320.,33.9999999999999,-25.));
#53134=CARTESIAN_POINT('',(-308.,33.9999999999999,-27.5));
#53135=CARTESIAN_POINT('Origin',(-308.,33.9999999999999,-25.));
#53136=CARTESIAN_POINT('',(-320.,33.9999999999999,-27.5));
#53137=CARTESIAN_POINT('',(-320.,33.9999999999999,-27.5));
#53138=CARTESIAN_POINT('Origin',(-320.,33.9999999999999,-25.));
#53139=CARTESIAN_POINT('Origin',(-320.,33.9999999999999,25.));
#53140=CARTESIAN_POINT('',(-308.,33.9999999999999,22.5));
#53141=CARTESIAN_POINT('Origin',(-308.,33.9999999999999,25.));
#53142=CARTESIAN_POINT('',(-320.,33.9999999999999,22.5));
#53143=CARTESIAN_POINT('',(-320.,33.9999999999999,22.5));
#53144=CARTESIAN_POINT('Origin',(-320.,33.9999999999999,25.));
#53145=CARTESIAN_POINT('Origin',(-320.,-34.0000000000001,25.));
#53146=CARTESIAN_POINT('',(-308.,-34.0000000000001,22.5));
#53147=CARTESIAN_POINT('Origin',(-308.,-34.0000000000001,25.));
#53148=CARTESIAN_POINT('',(-320.,-34.0000000000001,22.5));
#53149=CARTESIAN_POINT('',(-320.,-34.0000000000001,22.5));
#53150=CARTESIAN_POINT('Origin',(-320.,-34.0000000000001,25.));
#53151=CARTESIAN_POINT('Origin',(-320.,-34.0000000000001,-25.));
#53152=CARTESIAN_POINT('',(-308.,-34.0000000000001,-27.5));
#53153=CARTESIAN_POINT('Origin',(-308.,-34.0000000000001,-25.));
#53154=CARTESIAN_POINT('',(-320.,-34.0000000000001,-27.5));
#53155=CARTESIAN_POINT('',(-320.,-34.0000000000001,-27.5));
#53156=CARTESIAN_POINT('Origin',(-320.,-34.0000000000001,-25.));
#53157=CARTESIAN_POINT('Origin',(-308.,-94.,40.));
#53158=CARTESIAN_POINT('',(-314.4,-94.,45.5));
#53159=CARTESIAN_POINT('Origin',(-314.4,-94.,40.));
#53160=CARTESIAN_POINT('',(-308.,-94.,45.5));
#53161=CARTESIAN_POINT('',(-308.,-94.,45.5));
#53162=CARTESIAN_POINT('Origin',(-308.,-94.,40.));
#53163=CARTESIAN_POINT('Origin',(-308.,-94.,40.));
#53164=CARTESIAN_POINT('',(-320.,-94.,43.3));
#53165=CARTESIAN_POINT('Origin',(-320.,-94.,40.));
#53166=CARTESIAN_POINT('',(-314.4,-94.,43.3));
#53167=CARTESIAN_POINT('',(-308.,-94.,43.3));
#53168=CARTESIAN_POINT('Origin',(-314.4,-94.,40.));
#53169=CARTESIAN_POINT('Origin',(-308.,-93.9999999999999,84.9999999999999));
#53170=CARTESIAN_POINT('',(-314.4,-93.9999999999999,90.5));
#53171=CARTESIAN_POINT('Origin',(-314.4,-93.9999999999999,84.9999999999999));
#53172=CARTESIAN_POINT('',(-308.,-93.9999999999999,90.5));
#53173=CARTESIAN_POINT('',(-308.,-93.9999999999999,90.5));
#53174=CARTESIAN_POINT('Origin',(-308.,-93.9999999999999,84.9999999999999));
#53175=CARTESIAN_POINT('Origin',(-308.,-93.9999999999999,84.9999999999999));
#53176=CARTESIAN_POINT('',(-320.,-93.9999999999999,88.3));
#53177=CARTESIAN_POINT('Origin',(-320.,-93.9999999999999,84.9999999999999));
#53178=CARTESIAN_POINT('',(-314.4,-93.9999999999999,88.3));
#53179=CARTESIAN_POINT('',(-308.,-93.9999999999999,88.3));
#53180=CARTESIAN_POINT('Origin',(-314.4,-93.9999999999999,84.9999999999999));
#53181=CARTESIAN_POINT('Origin',(-308.,-151.,85.));
#53182=CARTESIAN_POINT('',(-314.4,-151.,90.5));
#53183=CARTESIAN_POINT('Origin',(-314.4,-151.,85.));
#53184=CARTESIAN_POINT('',(-308.,-151.,90.5));
#53185=CARTESIAN_POINT('',(-308.,-151.,90.5));
#53186=CARTESIAN_POINT('Origin',(-308.,-151.,85.));
#53187=CARTESIAN_POINT('Origin',(-308.,-151.,85.));
#53188=CARTESIAN_POINT('',(-320.,-151.,88.3));
#53189=CARTESIAN_POINT('Origin',(-320.,-151.,85.));
#53190=CARTESIAN_POINT('',(-314.4,-151.,88.3));
#53191=CARTESIAN_POINT('',(-308.,-151.,88.3));
#53192=CARTESIAN_POINT('Origin',(-314.4,-151.,85.));
#53193=CARTESIAN_POINT('Origin',(-308.,-151.,40.));
#53194=CARTESIAN_POINT('',(-314.4,-151.,45.5));
#53195=CARTESIAN_POINT('Origin',(-314.4,-151.,40.));
#53196=CARTESIAN_POINT('',(-308.,-151.,45.5));
#53197=CARTESIAN_POINT('',(-308.,-151.,45.5));
#53198=CARTESIAN_POINT('Origin',(-308.,-151.,40.));
#53199=CARTESIAN_POINT('Origin',(-308.,-151.,40.));
#53200=CARTESIAN_POINT('',(-320.,-151.,43.3));
#53201=CARTESIAN_POINT('Origin',(-320.,-151.,40.));
#53202=CARTESIAN_POINT('',(-314.4,-151.,43.3));
#53203=CARTESIAN_POINT('',(-308.,-151.,43.3));
#53204=CARTESIAN_POINT('Origin',(-314.4,-151.,40.));
#53205=CARTESIAN_POINT('Origin',(-308.,151.,40.));
#53206=CARTESIAN_POINT('',(-314.4,151.,45.5));
#53207=CARTESIAN_POINT('Origin',(-314.4,151.,40.));
#53208=CARTESIAN_POINT('',(-308.,151.,45.5));
#53209=CARTESIAN_POINT('',(-308.,151.,45.5));
#53210=CARTESIAN_POINT('Origin',(-308.,151.,40.));
#53211=CARTESIAN_POINT('Origin',(-308.,151.,40.));
#53212=CARTESIAN_POINT('',(-320.,151.,43.3));
#53213=CARTESIAN_POINT('Origin',(-320.,151.,40.));
#53214=CARTESIAN_POINT('',(-314.4,151.,43.3));
#53215=CARTESIAN_POINT('',(-308.,151.,43.3));
#53216=CARTESIAN_POINT('Origin',(-314.4,151.,40.));
#53217=CARTESIAN_POINT('Origin',(-308.,151.,85.));
#53218=CARTESIAN_POINT('',(-314.4,151.,90.5));
#53219=CARTESIAN_POINT('Origin',(-314.4,151.,85.));
#53220=CARTESIAN_POINT('',(-308.,151.,90.5));
#53221=CARTESIAN_POINT('',(-308.,151.,90.5));
#53222=CARTESIAN_POINT('Origin',(-308.,151.,85.));
#53223=CARTESIAN_POINT('Origin',(-308.,151.,85.));
#53224=CARTESIAN_POINT('',(-320.,151.,88.3));
#53225=CARTESIAN_POINT('Origin',(-320.,151.,85.));
#53226=CARTESIAN_POINT('',(-314.4,151.,88.3));
#53227=CARTESIAN_POINT('',(-308.,151.,88.3));
#53228=CARTESIAN_POINT('Origin',(-314.4,151.,85.));
#53229=CARTESIAN_POINT('Origin',(-308.,94.,85.));
#53230=CARTESIAN_POINT('',(-314.4,94.,90.5));
#53231=CARTESIAN_POINT('Origin',(-314.4,94.,85.));
#53232=CARTESIAN_POINT('',(-308.,94.,90.5));
#53233=CARTESIAN_POINT('',(-308.,94.,90.5));
#53234=CARTESIAN_POINT('Origin',(-308.,94.,85.));
#53235=CARTESIAN_POINT('Origin',(-308.,94.,85.));
#53236=CARTESIAN_POINT('',(-320.,94.,88.3));
#53237=CARTESIAN_POINT('Origin',(-320.,94.,85.));
#53238=CARTESIAN_POINT('',(-314.4,94.,88.3));
#53239=CARTESIAN_POINT('',(-308.,94.,88.3));
#53240=CARTESIAN_POINT('Origin',(-314.4,94.,85.));
#53241=CARTESIAN_POINT('Origin',(-308.,94.,40.));
#53242=CARTESIAN_POINT('',(-314.4,94.,45.5));
#53243=CARTESIAN_POINT('Origin',(-314.4,94.,40.));
#53244=CARTESIAN_POINT('',(-308.,94.,45.5));
#53245=CARTESIAN_POINT('',(-308.,94.,45.5));
#53246=CARTESIAN_POINT('Origin',(-308.,94.,40.));
#53247=CARTESIAN_POINT('Origin',(-308.,94.,40.));
#53248=CARTESIAN_POINT('',(-320.,94.,43.3));
#53249=CARTESIAN_POINT('Origin',(-320.,94.,40.));
#53250=CARTESIAN_POINT('',(-314.4,94.,43.3));
#53251=CARTESIAN_POINT('',(-308.,94.,43.3));
#53252=CARTESIAN_POINT('Origin',(-314.4,94.,40.));
#53253=CARTESIAN_POINT('Origin',(-308.,-94.,-85.0000000000001));
#53254=CARTESIAN_POINT('',(-314.4,-94.,-79.5));
#53255=CARTESIAN_POINT('Origin',(-314.4,-94.,-85.0000000000001));
#53256=CARTESIAN_POINT('',(-308.,-94.,-79.5));
#53257=CARTESIAN_POINT('',(-308.,-94.,-79.5));
#53258=CARTESIAN_POINT('Origin',(-308.,-94.,-85.0000000000001));
#53259=CARTESIAN_POINT('Origin',(-308.,-94.,-85.0000000000001));
#53260=CARTESIAN_POINT('',(-320.,-94.,-81.7));
#53261=CARTESIAN_POINT('Origin',(-320.,-94.,-85.0000000000001));
#53262=CARTESIAN_POINT('',(-314.4,-94.,-81.7));
#53263=CARTESIAN_POINT('',(-308.,-94.,-81.7));
#53264=CARTESIAN_POINT('Origin',(-314.4,-94.,-85.0000000000001));
#53265=CARTESIAN_POINT('Origin',(-308.,-93.9999999999999,-40.0000000000001));
#53266=CARTESIAN_POINT('',(-314.4,-93.9999999999999,-34.5000000000001));
#53267=CARTESIAN_POINT('Origin',(-314.4,-93.9999999999999,-40.0000000000001));
#53268=CARTESIAN_POINT('',(-308.,-93.9999999999999,-34.5000000000001));
#53269=CARTESIAN_POINT('',(-308.,-93.9999999999999,-34.5000000000001));
#53270=CARTESIAN_POINT('Origin',(-308.,-93.9999999999999,-40.0000000000001));
#53271=CARTESIAN_POINT('Origin',(-308.,-93.9999999999999,-40.0000000000001));
#53272=CARTESIAN_POINT('',(-320.,-93.9999999999999,-36.7));
#53273=CARTESIAN_POINT('Origin',(-320.,-93.9999999999999,-40.0000000000001));
#53274=CARTESIAN_POINT('',(-314.4,-93.9999999999999,-36.7));
#53275=CARTESIAN_POINT('',(-308.,-93.9999999999999,-36.7));
#53276=CARTESIAN_POINT('Origin',(-314.4,-93.9999999999999,-40.0000000000001));
#53277=CARTESIAN_POINT('Origin',(-308.,-151.,-40.));
#53278=CARTESIAN_POINT('',(-314.4,-151.,-34.5));
#53279=CARTESIAN_POINT('Origin',(-314.4,-151.,-40.));
#53280=CARTESIAN_POINT('',(-308.,-151.,-34.5));
#53281=CARTESIAN_POINT('',(-308.,-151.,-34.5));
#53282=CARTESIAN_POINT('Origin',(-308.,-151.,-40.));
#53283=CARTESIAN_POINT('Origin',(-308.,-151.,-40.));
#53284=CARTESIAN_POINT('',(-320.,-151.,-36.7));
#53285=CARTESIAN_POINT('Origin',(-320.,-151.,-40.));
#53286=CARTESIAN_POINT('',(-314.4,-151.,-36.7));
#53287=CARTESIAN_POINT('',(-308.,-151.,-36.7));
#53288=CARTESIAN_POINT('Origin',(-314.4,-151.,-40.));
#53289=CARTESIAN_POINT('Origin',(-308.,-151.,-85.));
#53290=CARTESIAN_POINT('',(-314.4,-151.,-79.5));
#53291=CARTESIAN_POINT('Origin',(-314.4,-151.,-85.));
#53292=CARTESIAN_POINT('',(-308.,-151.,-79.5));
#53293=CARTESIAN_POINT('',(-308.,-151.,-79.5));
#53294=CARTESIAN_POINT('Origin',(-308.,-151.,-85.));
#53295=CARTESIAN_POINT('Origin',(-308.,-151.,-85.));
#53296=CARTESIAN_POINT('',(-320.,-151.,-81.7));
#53297=CARTESIAN_POINT('Origin',(-320.,-151.,-85.));
#53298=CARTESIAN_POINT('',(-314.4,-151.,-81.7));
#53299=CARTESIAN_POINT('',(-308.,-151.,-81.7));
#53300=CARTESIAN_POINT('Origin',(-314.4,-151.,-85.));
#53301=CARTESIAN_POINT('Origin',(-308.,151.,-85.));
#53302=CARTESIAN_POINT('',(-314.4,151.,-79.5));
#53303=CARTESIAN_POINT('Origin',(-314.4,151.,-85.));
#53304=CARTESIAN_POINT('',(-308.,151.,-79.5));
#53305=CARTESIAN_POINT('',(-308.,151.,-79.5));
#53306=CARTESIAN_POINT('Origin',(-308.,151.,-85.));
#53307=CARTESIAN_POINT('Origin',(-308.,151.,-85.));
#53308=CARTESIAN_POINT('',(-320.,151.,-81.7));
#53309=CARTESIAN_POINT('Origin',(-320.,151.,-85.));
#53310=CARTESIAN_POINT('',(-314.4,151.,-81.7));
#53311=CARTESIAN_POINT('',(-308.,151.,-81.7));
#53312=CARTESIAN_POINT('Origin',(-314.4,151.,-85.));
#53313=CARTESIAN_POINT('Origin',(-308.,151.,-40.));
#53314=CARTESIAN_POINT('',(-314.4,151.,-34.5));
#53315=CARTESIAN_POINT('Origin',(-314.4,151.,-40.));
#53316=CARTESIAN_POINT('',(-308.,151.,-34.5));
#53317=CARTESIAN_POINT('',(-308.,151.,-34.5));
#53318=CARTESIAN_POINT('Origin',(-308.,151.,-40.));
#53319=CARTESIAN_POINT('Origin',(-308.,151.,-40.));
#53320=CARTESIAN_POINT('',(-320.,151.,-36.7));
#53321=CARTESIAN_POINT('Origin',(-320.,151.,-40.));
#53322=CARTESIAN_POINT('',(-314.4,151.,-36.7));
#53323=CARTESIAN_POINT('',(-308.,151.,-36.7));
#53324=CARTESIAN_POINT('Origin',(-314.4,151.,-40.));
#53325=CARTESIAN_POINT('Origin',(-308.,94.,-40.));
#53326=CARTESIAN_POINT('',(-314.4,94.,-34.5));
#53327=CARTESIAN_POINT('Origin',(-314.4,94.,-40.));
#53328=CARTESIAN_POINT('',(-308.,94.,-34.5));
#53329=CARTESIAN_POINT('',(-308.,94.,-34.5));
#53330=CARTESIAN_POINT('Origin',(-308.,94.,-40.));
#53331=CARTESIAN_POINT('Origin',(-308.,94.,-40.));
#53332=CARTESIAN_POINT('',(-320.,94.,-36.7));
#53333=CARTESIAN_POINT('Origin',(-320.,94.,-40.));
#53334=CARTESIAN_POINT('',(-314.4,94.,-36.7));
#53335=CARTESIAN_POINT('',(-308.,94.,-36.7));
#53336=CARTESIAN_POINT('Origin',(-314.4,94.,-40.));
#53337=CARTESIAN_POINT('Origin',(-308.,94.,-85.));
#53338=CARTESIAN_POINT('',(-314.4,94.,-79.5));
#53339=CARTESIAN_POINT('Origin',(-314.4,94.,-85.));
#53340=CARTESIAN_POINT('',(-308.,94.,-79.5));
#53341=CARTESIAN_POINT('',(-308.,94.,-79.5));
#53342=CARTESIAN_POINT('Origin',(-308.,94.,-85.));
#53343=CARTESIAN_POINT('Origin',(-308.,94.,-85.));
#53344=CARTESIAN_POINT('',(-320.,94.,-81.7));
#53345=CARTESIAN_POINT('Origin',(-320.,94.,-85.));
#53346=CARTESIAN_POINT('',(-314.4,94.,-81.7));
#53347=CARTESIAN_POINT('',(-308.,94.,-81.7));
#53348=CARTESIAN_POINT('Origin',(-314.4,94.,-85.));
#53349=CARTESIAN_POINT('Origin',(-320.,-160.,6.));
#53350=CARTESIAN_POINT('',(-320.,-155.,-110.));
#53351=CARTESIAN_POINT('',(-320.,155.,-110.));
#53352=CARTESIAN_POINT('',(-320.,175.,-110.));
#53353=CARTESIAN_POINT('',(-320.,-175.,-89.9999999999999));
#53354=CARTESIAN_POINT('',(-320.,-215.5,-49.4999999999997));
#53355=CARTESIAN_POINT('',(-320.,-175.,90.));
#53356=CARTESIAN_POINT('',(-320.,-175.,110.));
#53357=CARTESIAN_POINT('',(-320.,-155.,110.));
#53358=CARTESIAN_POINT('',(-320.,-209.5,55.5000000000003));
#53359=CARTESIAN_POINT('',(-320.,155.,110.));
#53360=CARTESIAN_POINT('',(-320.,175.,110.));
#53361=CARTESIAN_POINT('',(-320.,175.,89.9999999999999));
#53362=CARTESIAN_POINT('',(-320.,49.5000000000005,215.5));
#53363=CARTESIAN_POINT('',(-320.,175.,-90.));
#53364=CARTESIAN_POINT('',(-320.,175.,110.));
#53365=CARTESIAN_POINT('',(-320.,55.499999999999,-209.5));
#53366=CARTESIAN_POINT('Origin',(-320.,-160.,6.));
#53367=CARTESIAN_POINT('',(-308.,-160.,-6.));
#53368=CARTESIAN_POINT('',(64.9999999999998,-160.,-6.));
#53369=CARTESIAN_POINT('',(-320.,-160.,-6.));
#53370=CARTESIAN_POINT('',(64.9999999999998,-160.,6.));
#53371=CARTESIAN_POINT('',(64.9999999999999,-160.,6.));
#53372=CARTESIAN_POINT('',(-308.,-160.,6.));
#53373=CARTESIAN_POINT('',(-320.,-160.,6.));
#53374=CARTESIAN_POINT('',(-308.,-160.,6.));
#53375=CARTESIAN_POINT('Origin',(115.,-160.,6.));
#53376=CARTESIAN_POINT('',(115.,-110.,6.));
#53377=CARTESIAN_POINT('',(115.,110.,6.));
#53378=CARTESIAN_POINT('',(115.,-160.,6.));
#53379=CARTESIAN_POINT('',(115.,-110.,-6.));
#53380=CARTESIAN_POINT('',(115.,-110.,6.));
#53381=CARTESIAN_POINT('',(115.,110.,-6.));
#53382=CARTESIAN_POINT('',(115.,-160.,-6.));
#53383=CARTESIAN_POINT('',(115.,110.,6.));
#53384=CARTESIAN_POINT('Origin',(-320.,160.,6.));
#53385=CARTESIAN_POINT('',(-308.,160.,6.));
#53386=CARTESIAN_POINT('',(64.9999999999999,160.,6.));
#53387=CARTESIAN_POINT('',(-320.,160.,6.));
#53388=CARTESIAN_POINT('',(64.9999999999999,160.,-6.));
#53389=CARTESIAN_POINT('',(64.9999999999999,160.,-6.));
#53390=CARTESIAN_POINT('',(-308.,160.,-6.));
#53391=CARTESIAN_POINT('',(-320.,160.,-6.));
#53392=CARTESIAN_POINT('',(-308.,160.,6.));
#53393=CARTESIAN_POINT('Origin',(0.,0.,6.));
#53394=CARTESIAN_POINT('',(115.,-110.,6.));
#53395=CARTESIAN_POINT('',(64.9999999999999,160.,6.));
#53396=CARTESIAN_POINT('',(-308.,0.,6.));
#53397=CARTESIAN_POINT('',(17.5,-55.,6.00000000000001));
#53398=CARTESIAN_POINT('',(17.5,-55.,6.00000000000001));
#53399=CARTESIAN_POINT('',(17.5,55.,6.00000000000001));
#53400=CARTESIAN_POINT('',(17.5,55.,6.00000000000001));
#53401=CARTESIAN_POINT('Origin',(17.5,0.,6.00000000000001));
#53402=CARTESIAN_POINT('Origin',(0.,0.,-6.));
#53403=CARTESIAN_POINT('',(112.5,-112.5,-6.));
#53404=CARTESIAN_POINT('',(-308.,0.,-6.));
#53405=CARTESIAN_POINT('',(112.5,112.5,-6.));
#53406=CARTESIAN_POINT('',(17.5,-55.,-6.));
#53407=CARTESIAN_POINT('',(17.5,-55.,-6.));
#53408=CARTESIAN_POINT('',(17.5,55.,-6.));
#53409=CARTESIAN_POINT('Origin',(17.5,0.,-6.));
#53410=CARTESIAN_POINT('',(17.5,55.,-6.));
#53411=CARTESIAN_POINT('Origin',(-308.,0.,0.));
#53412=CARTESIAN_POINT('',(-308.,-175.,90.));
#53413=CARTESIAN_POINT('',(-308.,-175.,-89.9999999999999));
#53414=CARTESIAN_POINT('',(-308.,-175.,110.));
#53415=CARTESIAN_POINT('',(-308.,-155.,-110.));
#53416=CARTESIAN_POINT('',(-308.,-132.5,-132.5));
#53417=CARTESIAN_POINT('',(-308.,155.,-110.));
#53418=CARTESIAN_POINT('',(-308.,175.,-110.));
#53419=CARTESIAN_POINT('',(-308.,175.,-90.));
#53420=CARTESIAN_POINT('',(-308.,132.499999999999,-132.5));
#53421=CARTESIAN_POINT('',(-308.,175.,89.9999999999999));
#53422=CARTESIAN_POINT('',(-308.,175.,110.));
#53423=CARTESIAN_POINT('',(-308.,155.,110.));
#53424=CARTESIAN_POINT('',(-308.,132.5,132.5));
#53425=CARTESIAN_POINT('',(-308.,-155.,110.));
#53426=CARTESIAN_POINT('',(-308.,175.,110.));
#53427=CARTESIAN_POINT('',(-308.,-132.499999999999,132.5));
#53428=CARTESIAN_POINT('Origin',(-308.,175.,-110.));
#53429=CARTESIAN_POINT('',(-308.,-155.,-110.));
#53430=CARTESIAN_POINT('',(-308.,155.,-110.));
#53431=CARTESIAN_POINT('Origin',(-308.,175.,110.));
#53432=CARTESIAN_POINT('',(-308.,175.,89.9999999999999));
#53433=CARTESIAN_POINT('',(-308.,175.,-90.));
#53434=CARTESIAN_POINT('Origin',(-308.,175.,110.));
#53435=CARTESIAN_POINT('',(-308.,-155.,110.));
#53436=CARTESIAN_POINT('',(-308.,155.,110.));
#53437=CARTESIAN_POINT('Origin',(-308.,-175.,110.));
#53438=CARTESIAN_POINT('',(-308.,-175.,-89.9999999999999));
#53439=CARTESIAN_POINT('',(-308.,-175.,90.));
#53440=CARTESIAN_POINT('Origin',(-314.4,97.3,-85.));
#53441=CARTESIAN_POINT('Origin',(-314.4,97.3,-40.));
#53442=CARTESIAN_POINT('Origin',(-314.4,154.3,-40.));
#53443=CARTESIAN_POINT('Origin',(-314.4,154.3,-85.));
#53444=CARTESIAN_POINT('Origin',(-314.4,-147.7,-85.));
#53445=CARTESIAN_POINT('Origin',(-314.4,-147.7,-40.));
#53446=CARTESIAN_POINT('Origin',(-314.4,-90.6999999999999,-40.0000000000001));
#53447=CARTESIAN_POINT('Origin',(-314.4,-90.7,-85.0000000000001));
#53448=CARTESIAN_POINT('Origin',(-314.4,97.3,40.));
#53449=CARTESIAN_POINT('Origin',(-314.4,97.3,85.));
#53450=CARTESIAN_POINT('Origin',(-314.4,154.3,85.));
#53451=CARTESIAN_POINT('Origin',(-314.4,154.3,40.));
#53452=CARTESIAN_POINT('Origin',(-314.4,-147.7,40.));
#53453=CARTESIAN_POINT('Origin',(-314.4,-147.7,85.));
#53454=CARTESIAN_POINT('Origin',(-314.4,-90.6999999999999,84.9999999999999));
#53455=CARTESIAN_POINT('Origin',(-314.4,-90.7,40.));
#53456=CARTESIAN_POINT('Origin',(-190.,0.,1.));
#53457=CARTESIAN_POINT('Origin',(115.,-110.,6.));
#53458=CARTESIAN_POINT('Origin',(64.9999999999999,160.,6.));
#53459=CARTESIAN_POINT('Origin',(17.5,-55.,110.001));
#53460=CARTESIAN_POINT('',(17.5,-55.,110.001));
#53461=CARTESIAN_POINT('Origin',(17.5,55.,110.001));
#53462=CARTESIAN_POINT('',(17.5,55.,110.001));
#53463=CARTESIAN_POINT('Origin',(17.5,0.,110.001));
#53464=CARTESIAN_POINT('Origin',(-308.,-155.,-110.));
#53465=CARTESIAN_POINT('Origin',(-308.,-175.,90.));
#53466=CARTESIAN_POINT('Origin',(-308.,155.,110.));
#53467=CARTESIAN_POINT('Origin',(-308.,175.,-90.));
#53468=CARTESIAN_POINT('',(0.,0.,0.));
#53469=CARTESIAN_POINT('',(0.,0.,0.));
#53470=CARTESIAN_POINT('Origin',(0.,22.,-420.));
#53471=CARTESIAN_POINT('',(-6.73555739531045E-16,13.,-425.5));
#53472=CARTESIAN_POINT('Origin',(0.,13.,-420.));
#53473=CARTESIAN_POINT('',(-6.73555739531045E-16,22.,-425.5));
#53474=CARTESIAN_POINT('',(-6.73555739531045E-16,22.,-425.5));
#53475=CARTESIAN_POINT('Origin',(0.,22.,-420.));
#53476=CARTESIAN_POINT('Origin',(0.,22.,-420.));
#53477=CARTESIAN_POINT('',(-1.75,0.500000000000001,-416.968911086754));
#53478=CARTESIAN_POINT('',(1.75,0.5,-416.968911086754));
#53479=CARTESIAN_POINT('Origin',(0.,0.5,-420.));
#53480=CARTESIAN_POINT('',(-2.25,0.,-417.319048676309));
#53481=CARTESIAN_POINT('Origin',(1.23513471672609E-8,2.25000001235081,-420.000000017303));
#53482=CARTESIAN_POINT('',(-2.25,0.,-422.680951323691));
#53483=CARTESIAN_POINT('Origin',(0.,0.,-420.));
#53484=CARTESIAN_POINT('',(-1.75,0.500000000000001,-423.031088913246));
#53485=CARTESIAN_POINT('Origin',(-3.10164607886243E-8,2.24999996898292,
-420.000000044163));
#53486=CARTESIAN_POINT('',(-4.28626379701572E-16,0.499999999999998,-423.5));
#53487=CARTESIAN_POINT('Origin',(0.,0.5,-420.));
#53488=CARTESIAN_POINT('',(-4.28626379701574E-16,13.,-423.5));
#53489=CARTESIAN_POINT('',(-4.28626379701574E-16,22.,-423.5));
#53490=CARTESIAN_POINT('Origin',(0.,13.,-420.));
#53491=CARTESIAN_POINT('',(1.75,0.5,-423.031088913246));
#53492=CARTESIAN_POINT('Origin',(0.,0.5,-420.));
#53493=CARTESIAN_POINT('',(2.25,0.,-422.680951323691));
#53494=CARTESIAN_POINT('Origin',(-2.43443196157322E-8,2.25000002434478,
-419.999999965121));
#53495=CARTESIAN_POINT('',(2.25,0.,-417.319048676309));
#53496=CARTESIAN_POINT('Origin',(0.,0.,-420.));
#53497=CARTESIAN_POINT('Origin',(1.14266326955992E-8,2.24999998857398,-419.999999982967));
#53498=CARTESIAN_POINT('Origin',(0.,22.,-360.));
#53499=CARTESIAN_POINT('',(-6.73555739531045E-16,13.,-365.5));
#53500=CARTESIAN_POINT('Origin',(0.,13.,-360.));
#53501=CARTESIAN_POINT('',(-6.73555739531045E-16,22.,-365.5));
#53502=CARTESIAN_POINT('',(-6.73555739531045E-16,22.,-365.5));
#53503=CARTESIAN_POINT('Origin',(0.,22.,-360.));
#53504=CARTESIAN_POINT('Origin',(0.,22.,-360.));
#53505=CARTESIAN_POINT('',(-1.75,0.500000000000001,-356.968911086754));
#53506=CARTESIAN_POINT('',(1.75,0.5,-356.968911086754));
#53507=CARTESIAN_POINT('Origin',(0.,0.5,-360.));
#53508=CARTESIAN_POINT('',(-2.25,0.,-357.319048676309));
#53509=CARTESIAN_POINT('Origin',(-1.81638087903835E-8,2.24999998183567,
-359.999999973801));
#53510=CARTESIAN_POINT('',(-2.25,0.,-362.680951323691));
#53511=CARTESIAN_POINT('Origin',(0.,0.,-360.));
#53512=CARTESIAN_POINT('',(-1.75,0.500000000000001,-363.031088913246));
#53513=CARTESIAN_POINT('Origin',(-4.23829027429434E-10,2.24999999957564,
-360.000000000522));
#53514=CARTESIAN_POINT('',(-4.28626379701572E-16,0.499999999999998,-363.5));
#53515=CARTESIAN_POINT('Origin',(0.,0.5,-360.));
#53516=CARTESIAN_POINT('',(-4.28626379701574E-16,13.,-363.5));
#53517=CARTESIAN_POINT('',(-4.28626379701574E-16,22.,-363.5));
#53518=CARTESIAN_POINT('Origin',(0.,13.,-360.));
#53519=CARTESIAN_POINT('',(1.75,0.5,-363.031088913246));
#53520=CARTESIAN_POINT('Origin',(0.,0.5,-360.));
#53521=CARTESIAN_POINT('',(2.24999999999999,0.,-362.680951323691));
#53522=CARTESIAN_POINT('Origin',(-1.81887060968222E-9,2.25000000181898,
-359.99999999671));
#53523=CARTESIAN_POINT('',(2.24999999999999,0.,-357.319048676309));
#53524=CARTESIAN_POINT('Origin',(0.,0.,-360.));
#53525=CARTESIAN_POINT('Origin',(-4.00230404373758E-8,2.2500000400232,-360.000000056605));
#53526=CARTESIAN_POINT('Origin',(0.,22.,-300.));
#53527=CARTESIAN_POINT('',(-6.73555739531045E-16,13.,-305.5));
#53528=CARTESIAN_POINT('Origin',(0.,13.,-300.));
#53529=CARTESIAN_POINT('',(-6.73555739531045E-16,22.,-305.5));
#53530=CARTESIAN_POINT('',(-6.73555739531045E-16,22.,-305.5));
#53531=CARTESIAN_POINT('Origin',(0.,22.,-300.));
#53532=CARTESIAN_POINT('Origin',(0.,22.,-300.));
#53533=CARTESIAN_POINT('',(-1.75,0.500000000000001,-296.968911086754));
#53534=CARTESIAN_POINT('',(1.75,0.5,-296.968911086754));
#53535=CARTESIAN_POINT('Origin',(0.,0.5,-300.));
#53536=CARTESIAN_POINT('',(-2.25,0.,-297.319048676309));
#53537=CARTESIAN_POINT('Origin',(-6.9596634011404E-10,2.24999999930352,
-299.999999999323));
#53538=CARTESIAN_POINT('',(-2.25,0.,-302.680951323691));
#53539=CARTESIAN_POINT('Origin',(0.,0.,-300.));
#53540=CARTESIAN_POINT('',(-1.75,0.500000000000001,-303.031088913246));
#53541=CARTESIAN_POINT('Origin',(-5.11468117858627E-9,2.24999999488474,
-300.000000007122));
#53542=CARTESIAN_POINT('',(-4.28626379701572E-16,0.499999999999998,-303.5));
#53543=CARTESIAN_POINT('Origin',(0.,0.5,-300.));
#53544=CARTESIAN_POINT('',(-4.28626379701574E-16,13.,-303.5));
#53545=CARTESIAN_POINT('',(-4.28626379701574E-16,22.,-303.5));
#53546=CARTESIAN_POINT('Origin',(0.,13.,-300.));
#53547=CARTESIAN_POINT('',(1.75,0.5,-303.031088913246));
#53548=CARTESIAN_POINT('Origin',(0.,0.5,-300.));
#53549=CARTESIAN_POINT('',(2.24999999999999,0.,-302.680951323691));
#53550=CARTESIAN_POINT('Origin',(1.1544250833051E-8,2.24999998845594,-300.000000016304));
#53551=CARTESIAN_POINT('',(2.24999999999999,0.,-297.319048676309));
#53552=CARTESIAN_POINT('Origin',(0.,0.,-300.));
#53553=CARTESIAN_POINT('Origin',(4.10078357382382E-8,2.2499999589923,-299.999999941256));
#53554=CARTESIAN_POINT('Origin',(0.,22.,-240.));
#53555=CARTESIAN_POINT('',(-6.73555739531045E-16,13.,-245.5));
#53556=CARTESIAN_POINT('Origin',(0.,13.,-240.));
#53557=CARTESIAN_POINT('',(-6.73555739531045E-16,22.,-245.5));
#53558=CARTESIAN_POINT('',(-6.73555739531045E-16,22.,-245.5));
#53559=CARTESIAN_POINT('Origin',(0.,22.,-240.));
#53560=CARTESIAN_POINT('Origin',(0.,22.,-240.));
#53561=CARTESIAN_POINT('',(-1.75,0.500000000000001,-236.968911086754));
#53562=CARTESIAN_POINT('',(1.75,0.5,-236.968911086754));
#53563=CARTESIAN_POINT('Origin',(0.,0.5,-240.));
#53564=CARTESIAN_POINT('',(-2.25,0.,-237.319048676309));
#53565=CARTESIAN_POINT('Origin',(2.09455894295552E-8,2.25000002094498,-240.00000002998));
#53566=CARTESIAN_POINT('',(-2.25,0.,-242.680951323691));
#53567=CARTESIAN_POINT('Origin',(0.,0.,-240.));
#53568=CARTESIAN_POINT('',(-1.75,0.500000000000001,-243.031088913246));
#53569=CARTESIAN_POINT('Origin',(-3.71720848546531E-9,2.24999999628211,
-240.000000004996));
#53570=CARTESIAN_POINT('',(-4.28626379701572E-16,0.499999999999998,-243.5));
#53571=CARTESIAN_POINT('Origin',(0.,0.5,-240.));
#53572=CARTESIAN_POINT('',(-4.28626379701574E-16,13.,-243.5));
#53573=CARTESIAN_POINT('',(-4.28626379701574E-16,22.,-243.5));
#53574=CARTESIAN_POINT('Origin',(0.,13.,-240.));
#53575=CARTESIAN_POINT('',(1.75,0.5,-243.031088913246));
#53576=CARTESIAN_POINT('Origin',(0.,0.5,-240.));
#53577=CARTESIAN_POINT('',(2.25,0.,-242.680951323691));
#53578=CARTESIAN_POINT('Origin',(-3.97217841952013E-9,2.25000000397282,
-239.999999995265));
#53579=CARTESIAN_POINT('',(2.25,0.,-237.319048676309));
#53580=CARTESIAN_POINT('Origin',(0.,0.,-240.));
#53581=CARTESIAN_POINT('Origin',(9.45980321853668E-9,2.24999999054093,-239.999999986565));
#53582=CARTESIAN_POINT('Origin',(0.,22.,-180.));
#53583=CARTESIAN_POINT('',(-6.73555739531045E-16,13.,-185.5));
#53584=CARTESIAN_POINT('Origin',(0.,13.,-180.));
#53585=CARTESIAN_POINT('',(-6.73555739531045E-16,22.,-185.5));
#53586=CARTESIAN_POINT('',(-6.73555739531045E-16,22.,-185.5));
#53587=CARTESIAN_POINT('Origin',(0.,22.,-180.));
#53588=CARTESIAN_POINT('Origin',(0.,22.,-180.));
#53589=CARTESIAN_POINT('',(-1.75,0.500000000000001,-176.968911086754));
#53590=CARTESIAN_POINT('',(1.75,0.5,-176.968911086755));
#53591=CARTESIAN_POINT('Origin',(0.,0.5,-180.));
#53592=CARTESIAN_POINT('',(-2.25,0.,-177.319048676309));
#53593=CARTESIAN_POINT('Origin',(1.45397632822508E-8,2.25000001453915,-180.000000021041));
#53594=CARTESIAN_POINT('',(-2.25,0.,-182.680951323691));
#53595=CARTESIAN_POINT('Origin',(0.,0.,-180.));
#53596=CARTESIAN_POINT('',(-1.75,0.500000000000001,-183.031088913246));
#53597=CARTESIAN_POINT('Origin',(-1.75473274799387E-9,2.24999999824459,
-180.000000002503));
#53598=CARTESIAN_POINT('',(-4.28626379701572E-16,0.499999999999998,-183.5));
#53599=CARTESIAN_POINT('Origin',(0.,0.5,-180.));
#53600=CARTESIAN_POINT('',(-4.28626379701574E-16,13.,-183.5));
#53601=CARTESIAN_POINT('',(-4.28626379701574E-16,22.,-183.5));
#53602=CARTESIAN_POINT('Origin',(0.,13.,-180.));
#53603=CARTESIAN_POINT('',(1.75,0.5,-183.031088913246));
#53604=CARTESIAN_POINT('Origin',(0.,0.5,-180.));
#53605=CARTESIAN_POINT('',(2.24999999999999,0.,-182.680951323691));
#53606=CARTESIAN_POINT('Origin',(-1.31895855348674E-9,2.25000000131934,
-179.999999998353));
#53607=CARTESIAN_POINT('',(2.24999999999999,0.,-177.319048676309));
#53608=CARTESIAN_POINT('Origin',(0.,0.,-180.));
#53609=CARTESIAN_POINT('Origin',(2.13298301243725E-8,2.24999997867055,-179.999999969452));
#53610=CARTESIAN_POINT('Origin',(0.,22.,-120.));
#53611=CARTESIAN_POINT('',(-6.73555739531045E-16,13.,-125.5));
#53612=CARTESIAN_POINT('Origin',(0.,13.,-120.));
#53613=CARTESIAN_POINT('',(-6.73555739531045E-16,22.,-125.5));
#53614=CARTESIAN_POINT('',(-6.73555739531045E-16,22.,-125.5));
#53615=CARTESIAN_POINT('Origin',(0.,22.,-120.));
#53616=CARTESIAN_POINT('Origin',(0.,22.,-120.));
#53617=CARTESIAN_POINT('',(-1.75,0.500000000000001,-116.968911086754));
#53618=CARTESIAN_POINT('',(1.75,0.5,-116.968911086755));
#53619=CARTESIAN_POINT('Origin',(0.,0.5,-120.));
#53620=CARTESIAN_POINT('',(-2.25,0.,-117.319048676309));
#53621=CARTESIAN_POINT('Origin',(-2.48057657747935E-9,2.24999999751883,
-119.999999996391));
#53622=CARTESIAN_POINT('',(-2.25,0.,-122.680951323691));
#53623=CARTESIAN_POINT('Origin',(0.,0.,-120.));
#53624=CARTESIAN_POINT('',(-1.75,0.500000000000001,-123.031088913246));
#53625=CARTESIAN_POINT('Origin',(6.68797350833472E-9,2.25000000668744,-119.99999999052));
#53626=CARTESIAN_POINT('',(-4.28626379701574E-16,0.499999999999998,-123.5));
#53627=CARTESIAN_POINT('Origin',(0.,0.5,-120.));
#53628=CARTESIAN_POINT('',(-4.28626379701574E-16,13.,-123.5));
#53629=CARTESIAN_POINT('',(-4.28626379701574E-16,22.,-123.5));
#53630=CARTESIAN_POINT('Origin',(0.,13.,-120.));
#53631=CARTESIAN_POINT('',(1.75,0.5,-123.031088913246));
#53632=CARTESIAN_POINT('Origin',(0.,0.5,-120.));
#53633=CARTESIAN_POINT('',(2.24999999999999,0.,-122.680951323691));
#53634=CARTESIAN_POINT('Origin',(-1.15682741164136E-9,2.25000000115695,
-119.999999998469));
#53635=CARTESIAN_POINT('',(2.24999999999999,0.,-117.319048676309));
#53636=CARTESIAN_POINT('Origin',(0.,0.,-120.));
#53637=CARTESIAN_POINT('Origin',(8.38862423968578E-9,2.24999999161153,-119.999999987973));
#53638=CARTESIAN_POINT('Origin',(0.,22.,-60.));
#53639=CARTESIAN_POINT('',(-6.73555739531044E-16,13.,-65.5));
#53640=CARTESIAN_POINT('Origin',(0.,13.,-60.));
#53641=CARTESIAN_POINT('',(-6.73555739531044E-16,22.,-65.5));
#53642=CARTESIAN_POINT('',(-6.73555739531044E-16,22.,-65.5));
#53643=CARTESIAN_POINT('Origin',(0.,22.,-60.));
#53644=CARTESIAN_POINT('Origin',(0.,22.,-60.));
#53645=CARTESIAN_POINT('',(-1.75,0.500000000000001,-56.9689110867545));
#53646=CARTESIAN_POINT('',(1.75,0.5,-56.9689110867546));
#53647=CARTESIAN_POINT('Origin',(0.,0.5,-60.));
#53648=CARTESIAN_POINT('',(-2.25,0.,-57.3190486763091));
#53649=CARTESIAN_POINT('Origin',(-5.2602575073557E-9,2.2499999947395,-59.9999999924325));
#53650=CARTESIAN_POINT('',(-2.25,0.,-62.6809513236909));
#53651=CARTESIAN_POINT('Origin',(0.,0.,-60.));
#53652=CARTESIAN_POINT('',(-1.75,0.500000000000001,-63.0310889132455));
#53653=CARTESIAN_POINT('Origin',(4.60471411001251E-9,2.25000000460459,-59.999999993365));
#53654=CARTESIAN_POINT('',(-4.28626379701573E-16,0.499999999999998,-63.5));
#53655=CARTESIAN_POINT('Origin',(0.,0.5,-60.));
#53656=CARTESIAN_POINT('',(-4.28626379701573E-16,13.,-63.5));
#53657=CARTESIAN_POINT('',(-4.28626379701573E-16,22.,-63.5));
#53658=CARTESIAN_POINT('Origin',(0.,13.,-60.));
#53659=CARTESIAN_POINT('',(1.75,0.5,-63.0310889132457));
#53660=CARTESIAN_POINT('Origin',(0.,0.5,-60.));
#53661=CARTESIAN_POINT('',(2.24999999999999,0.,-62.6809513236909));
#53662=CARTESIAN_POINT('Origin',(-6.26890206412156E-10,2.25000000062714,
-59.9999999992371));
#53663=CARTESIAN_POINT('',(2.24999999999999,0.,-57.3190486763091));
#53664=CARTESIAN_POINT('Origin',(0.,0.,-60.));
#53665=CARTESIAN_POINT('Origin',(1.79430359459332E-10,2.24999999982085,
-59.9999999997029));
#53666=CARTESIAN_POINT('Origin',(0.,22.,0.));
#53667=CARTESIAN_POINT('',(-6.73555739531044E-16,13.,-5.5));
#53668=CARTESIAN_POINT('Origin',(0.,13.,0.));
#53669=CARTESIAN_POINT('',(-6.73555739531044E-16,22.,-5.5));
#53670=CARTESIAN_POINT('',(-6.73555739531044E-16,22.,-5.5));
#53671=CARTESIAN_POINT('Origin',(0.,22.,0.));
#53672=CARTESIAN_POINT('Origin',(0.,22.,0.));
#53673=CARTESIAN_POINT('',(-1.75,0.500000000000001,3.03108891324553));
#53674=CARTESIAN_POINT('',(1.75,0.5,3.03108891324544));
#53675=CARTESIAN_POINT('Origin',(0.,0.5,0.));
#53676=CARTESIAN_POINT('',(-2.25,0.,2.68095132369089));
#53677=CARTESIAN_POINT('Origin',(6.82837120180579E-11,2.25000000006793,
-9.89575088539141E-11));
#53678=CARTESIAN_POINT('',(-2.25,0.,-2.68095132369089));
#53679=CARTESIAN_POINT('Origin',(0.,0.,0.));
#53680=CARTESIAN_POINT('',(-1.75,0.500000000000001,-3.03108891324553));
#53681=CARTESIAN_POINT('Origin',(1.41059108837993E-10,2.25000000014086,
2.02939887117282E-10));
#53682=CARTESIAN_POINT('',(-4.28626379701573E-16,0.499999999999998,-3.5));
#53683=CARTESIAN_POINT('Origin',(0.,0.5,0.));
#53684=CARTESIAN_POINT('',(-4.28626379701573E-16,13.,-3.5));
#53685=CARTESIAN_POINT('',(-4.28626379701573E-16,22.,-3.5));
#53686=CARTESIAN_POINT('Origin',(0.,13.,0.));
#53687=CARTESIAN_POINT('',(1.75,0.5,-3.03108891324566));
#53688=CARTESIAN_POINT('Origin',(0.,0.5,0.));
#53689=CARTESIAN_POINT('',(2.24999999999999,0.,-2.6809513236909));
#53690=CARTESIAN_POINT('Origin',(-1.22898358156931E-10,2.25000000012316,
9.97296689675409E-11));
#53691=CARTESIAN_POINT('',(2.24999999999999,0.,2.6809513236909));
#53692=CARTESIAN_POINT('Origin',(0.,0.,0.));
#53693=CARTESIAN_POINT('Origin',(1.95984894979517E-11,2.24999999998063,
-2.54418708323101E-11));
#53694=CARTESIAN_POINT('Origin',(-2.25,-1.4389599889981E-16,-450.));
#53695=CARTESIAN_POINT('',(-1.75,0.5,-450.));
#53696=CARTESIAN_POINT('',(-1.75,0.5,-450.));
#53697=CARTESIAN_POINT('',(-2.25,-1.4389599889981E-16,-450.));
#53698=CARTESIAN_POINT('',(-2.25,-1.4389599889981E-16,-450.));
#53699=CARTESIAN_POINT('',(-2.25,-1.4389599889981E-16,-450.));
#53700=CARTESIAN_POINT('Origin',(-1.75,0.5,-450.));
#53701=CARTESIAN_POINT('',(-1.75,0.5,-450.));
#53702=CARTESIAN_POINT('',(1.75,0.5,-450.));
#53703=CARTESIAN_POINT('Origin',(1.75,0.5,-450.));
#53704=CARTESIAN_POINT('',(2.25,-1.30104260698261E-15,-450.));
#53705=CARTESIAN_POINT('Origin',(0.,0.,-450.));
#53706=CARTESIAN_POINT('',(-2.25,-1.4389599889981E-16,-450.));
#53707=CARTESIAN_POINT('',(-2.25,-1.4389599889981E-16,-450.));
#53708=CARTESIAN_POINT('',(-2.25,-1.4389599889981E-16,-450.));
#53709=CARTESIAN_POINT('',(-2.25,-1.4389599889981E-16,-450.));
#53710=CARTESIAN_POINT('',(-2.25,-1.4389599889981E-16,-450.));
#53711=CARTESIAN_POINT('',(-2.25,-1.4389599889981E-16,-450.));
#53712=CARTESIAN_POINT('',(-2.25,-1.4389599889981E-16,-450.));
#53713=CARTESIAN_POINT('',(-2.25,-1.4389599889981E-16,30.));
#53714=CARTESIAN_POINT('',(-2.25,-1.4389599889981E-16,-450.));
#53715=CARTESIAN_POINT('',(-10.5,-1.28587913910472E-15,30.));
#53716=CARTESIAN_POINT('',(0.,0.,30.));
#53717=CARTESIAN_POINT('',(-10.5,-1.28587913910472E-15,-450.));
#53718=CARTESIAN_POINT('',(-10.5,-1.28587913910472E-15,-450.));
#53719=CARTESIAN_POINT('',(0.,0.,-450.));
#53720=CARTESIAN_POINT('Origin',(0.,0.,-450.));
#53721=CARTESIAN_POINT('',(2.24999999999999,2.75545529808154E-16,-450.));
#53722=CARTESIAN_POINT('',(2.25,-1.30104260698261E-15,-450.));
#53723=CARTESIAN_POINT('',(10.5,-1.28587913910472E-15,-450.));
#53724=CARTESIAN_POINT('',(0.,0.,-450.));
#53725=CARTESIAN_POINT('',(10.5,-1.28587913910472E-15,30.));
#53726=CARTESIAN_POINT('',(10.5,-1.28587913910472E-15,-450.));
#53727=CARTESIAN_POINT('',(2.25,-1.30104260698261E-15,30.));
#53728=CARTESIAN_POINT('',(0.,0.,30.));
#53729=CARTESIAN_POINT('',(2.25,-1.30104260698261E-15,-450.));
#53730=CARTESIAN_POINT('',(2.25,-1.30104260698261E-15,-450.));
#53731=CARTESIAN_POINT('',(2.25,-1.30104260698261E-15,-450.));
#53732=CARTESIAN_POINT('',(2.25,-1.30104260698261E-15,-450.));
#53733=CARTESIAN_POINT('',(2.25,-1.30104260698261E-15,-450.));
#53734=CARTESIAN_POINT('',(2.25,-1.30104260698261E-15,-450.));
#53735=CARTESIAN_POINT('',(2.25,-1.30104260698261E-15,-450.));
#53736=CARTESIAN_POINT('Origin',(-2.25,-1.4389599889981E-16,-450.));
#53737=CARTESIAN_POINT('Origin',(-1.75,0.5,-450.));
#53738=CARTESIAN_POINT('',(-1.75,0.5,-450.));
#53739=CARTESIAN_POINT('',(1.75,0.5,-450.));
#53740=CARTESIAN_POINT('Origin',(1.75,0.5,-450.));
#53741=CARTESIAN_POINT('Origin',(-2.25,-1.4389599889981E-16,-450.));
#53742=CARTESIAN_POINT('Origin',(-1.75,0.5,-450.));
#53743=CARTESIAN_POINT('',(-1.75,0.5,-450.));
#53744=CARTESIAN_POINT('',(1.75,0.5,-450.));
#53745=CARTESIAN_POINT('Origin',(1.75,0.5,-450.));
#53746=CARTESIAN_POINT('Origin',(-2.25,-1.4389599889981E-16,-450.));
#53747=CARTESIAN_POINT('Origin',(1.75,0.5,-450.));
#53748=CARTESIAN_POINT('',(1.75,0.5,-450.));
#53749=CARTESIAN_POINT('Origin',(-1.75,0.5,-450.));
#53750=CARTESIAN_POINT('',(-1.75,0.5,-450.));
#53751=CARTESIAN_POINT('Origin',(-2.25,-1.4389599889981E-16,-450.));
#53752=CARTESIAN_POINT('Origin',(-1.75,0.5,-450.));
#53753=CARTESIAN_POINT('',(-1.75,0.5,-450.));
#53754=CARTESIAN_POINT('',(1.75,0.5,-450.));
#53755=CARTESIAN_POINT('Origin',(1.75,0.5,-450.));
#53756=CARTESIAN_POINT('Origin',(-2.25,-1.4389599889981E-16,-450.));
#53757=CARTESIAN_POINT('Origin',(-1.75,0.5,-450.));
#53758=CARTESIAN_POINT('',(-1.75,0.5,-450.));
#53759=CARTESIAN_POINT('',(1.75,0.5,-450.));
#53760=CARTESIAN_POINT('Origin',(1.75,0.5,-450.));
#53761=CARTESIAN_POINT('Origin',(-2.25,-1.4389599889981E-16,-450.));
#53762=CARTESIAN_POINT('Origin',(-1.75,0.5,-450.));
#53763=CARTESIAN_POINT('',(-1.75,0.5,-450.));
#53764=CARTESIAN_POINT('',(1.75,0.5,-450.));
#53765=CARTESIAN_POINT('Origin',(1.75,0.5,-450.));
#53766=CARTESIAN_POINT('Origin',(-2.25,-1.4389599889981E-16,-450.));
#53767=CARTESIAN_POINT('Origin',(-1.75,0.5,-450.));
#53768=CARTESIAN_POINT('',(-1.75,0.5,30.));
#53769=CARTESIAN_POINT('',(-1.75,0.5,-450.));
#53770=CARTESIAN_POINT('',(1.75,0.5,30.));
#53771=CARTESIAN_POINT('',(1.75,0.5,-450.));
#53772=CARTESIAN_POINT('',(-1.75,0.5,30.));
#53773=CARTESIAN_POINT('Origin',(1.75,0.5,-450.));
#53774=CARTESIAN_POINT('',(1.75,0.5,30.));
#53775=CARTESIAN_POINT('Origin',(0.,0.,-450.));
#53776=CARTESIAN_POINT('',(-11.5,1.00000000000001,-450.));
#53777=CARTESIAN_POINT('',(-10.5,-1.28587913910472E-15,-450.));
#53778=CARTESIAN_POINT('',(-11.5,5.8257864376269,-450.));
#53779=CARTESIAN_POINT('',(-11.5,1.00000000000001,-450.));
#53780=CARTESIAN_POINT('',(-11.2071067811865,6.53289321881345,-450.));
#53781=CARTESIAN_POINT('Origin',(-10.5,5.8257864376269,-450.));
#53782=CARTESIAN_POINT('',(-8.19644660940673,9.54355339059324,-450.));
#53783=CARTESIAN_POINT('',(-11.5,6.24,-450.));
#53784=CARTESIAN_POINT('',(-8.05,9.89710678118651,-450.));
#53785=CARTESIAN_POINT('Origin',(-8.55,9.89710678118651,-450.));
#53786=CARTESIAN_POINT('',(-8.05,13.5928932188135,-450.));
#53787=CARTESIAN_POINT('',(-8.05,9.68999999999997,-450.));
#53788=CARTESIAN_POINT('',(-8.19644660940672,13.9464466094067,-450.));
#53789=CARTESIAN_POINT('Origin',(-8.55,13.5928932188135,-450.));
#53790=CARTESIAN_POINT('',(-8.57259699813414,14.3225969981341,-450.));
#53791=CARTESIAN_POINT('',(-8.05,13.8,-450.));
#53792=CARTESIAN_POINT('',(-8.71475010619428,14.6107663907404,-450.));
#53793=CARTESIAN_POINT('Origin',(-8.21904360754086,14.6761503887274,-450.));
#53794=CARTESIAN_POINT('',(-10.6942336092596,16.5902498938057,-450.));
#53795=CARTESIAN_POINT('Origin',(-10.995,14.31,-450.));
#53796=CARTESIAN_POINT('',(-10.9824030018658,16.7324030018659,-450.));
#53797=CARTESIAN_POINT('Origin',(-10.6288496112726,17.0859563924591,-450.));
#53798=CARTESIAN_POINT('',(-11.3535533905933,17.1035533905933,-450.));
#53799=CARTESIAN_POINT('',(-8.05,13.8,-450.));
#53800=CARTESIAN_POINT('',(-11.5,17.4571067811866,-450.));
#53801=CARTESIAN_POINT('Origin',(-11.,17.4571067811866,-450.));
#53802=CARTESIAN_POINT('',(-11.5,18.3428932188135,-450.));
#53803=CARTESIAN_POINT('',(-11.5,18.55,-450.));
#53804=CARTESIAN_POINT('',(-11.3535533905933,18.6964466094068,-450.));
#53805=CARTESIAN_POINT('Origin',(-11.,18.3428932188135,-450.));
#53806=CARTESIAN_POINT('',(-10.9824030018659,19.0675969981341,-450.));
#53807=CARTESIAN_POINT('',(-8.05,22.,-450.));
#53808=CARTESIAN_POINT('',(-10.6942336092596,19.2097501061943,-450.));
#53809=CARTESIAN_POINT('Origin',(-10.6288496112726,18.7140436075409,-450.));
#53810=CARTESIAN_POINT('',(-8.71475010619428,21.1892336092596,-450.));
#53811=CARTESIAN_POINT('Origin',(-10.995,21.49,-450.));
#53812=CARTESIAN_POINT('',(-8.57259699813413,21.4774030018659,-450.));
#53813=CARTESIAN_POINT('Origin',(-8.21904360754086,21.1238496112726,-450.));
#53814=CARTESIAN_POINT('',(-8.05,22.,-450.));
#53815=CARTESIAN_POINT('',(-8.05,22.,-450.));
#53816=CARTESIAN_POINT('',(8.05,22.,-450.));
#53817=CARTESIAN_POINT('',(-8.05,22.,-450.));
#53818=CARTESIAN_POINT('',(8.57259699813413,21.4774030018659,-450.));
#53819=CARTESIAN_POINT('',(8.05,22.,-450.));
#53820=CARTESIAN_POINT('',(8.71475010619428,21.1892336092596,-450.));
#53821=CARTESIAN_POINT('Origin',(8.21904360754086,21.1238496112726,-450.));
#53822=CARTESIAN_POINT('',(10.6942336092596,19.2097501061943,-450.));
#53823=CARTESIAN_POINT('Origin',(10.995,21.49,-450.));
#53824=CARTESIAN_POINT('',(10.9824030018659,19.0675969981341,-450.));
#53825=CARTESIAN_POINT('Origin',(10.6288496112726,18.7140436075409,-450.));
#53826=CARTESIAN_POINT('',(11.3535533905933,18.6964466094068,-450.));
#53827=CARTESIAN_POINT('',(8.05,22.,-450.));
#53828=CARTESIAN_POINT('',(11.5,18.3428932188135,-450.));
#53829=CARTESIAN_POINT('Origin',(11.,18.3428932188135,-450.));
#53830=CARTESIAN_POINT('',(11.5,17.4571067811866,-450.));
#53831=CARTESIAN_POINT('',(11.5,18.55,-450.));
#53832=CARTESIAN_POINT('',(11.3535533905933,17.1035533905933,-450.));
#53833=CARTESIAN_POINT('Origin',(11.,17.4571067811866,-450.));
#53834=CARTESIAN_POINT('',(10.9824030018658,16.7324030018659,-450.));
#53835=CARTESIAN_POINT('',(8.05,13.8,-450.));
#53836=CARTESIAN_POINT('',(10.6942336092596,16.5902498938057,-450.));
#53837=CARTESIAN_POINT('Origin',(10.6288496112726,17.0859563924591,-450.));
#53838=CARTESIAN_POINT('',(8.71475010619428,14.6107663907404,-450.));
#53839=CARTESIAN_POINT('Origin',(10.995,14.31,-450.));
#53840=CARTESIAN_POINT('',(8.57259699813414,14.3225969981341,-450.));
#53841=CARTESIAN_POINT('Origin',(8.21904360754086,14.6761503887274,-450.));
#53842=CARTESIAN_POINT('',(8.19644660940672,13.9464466094067,-450.));
#53843=CARTESIAN_POINT('',(8.05,13.8,-450.));
#53844=CARTESIAN_POINT('',(8.05,13.5928932188135,-450.));
#53845=CARTESIAN_POINT('Origin',(8.55,13.5928932188135,-450.));
#53846=CARTESIAN_POINT('',(8.05,9.89710678118651,-450.));
#53847=CARTESIAN_POINT('',(8.05,9.68999999999997,-450.));
#53848=CARTESIAN_POINT('',(8.19644660940673,9.54355339059324,-450.));
#53849=CARTESIAN_POINT('Origin',(8.55,9.89710678118651,-450.));
#53850=CARTESIAN_POINT('',(11.2071067811865,6.53289321881345,-450.));
#53851=CARTESIAN_POINT('',(11.5,6.24,-450.));
#53852=CARTESIAN_POINT('',(11.5,5.8257864376269,-450.));
#53853=CARTESIAN_POINT('Origin',(10.5,5.8257864376269,-450.));
#53854=CARTESIAN_POINT('',(11.5,1.00000000000001,-450.));
#53855=CARTESIAN_POINT('',(11.5,1.00000000000001,-450.));
#53856=CARTESIAN_POINT('',(10.5,-1.28587913910472E-15,-450.));
#53857=CARTESIAN_POINT('',(1.75,0.5,-450.));
#53858=CARTESIAN_POINT('',(1.75,0.5,-450.));
#53859=CARTESIAN_POINT('',(-1.75,0.5,-450.));
#53860=CARTESIAN_POINT('Origin',(0.,0.,30.));
#53861=CARTESIAN_POINT('',(-2.25,-1.4389599889981E-16,30.));
#53862=CARTESIAN_POINT('',(11.5,1.00000000000001,30.));
#53863=CARTESIAN_POINT('',(10.5,-1.28587913910472E-15,30.));
#53864=CARTESIAN_POINT('',(11.5,5.8257864376269,30.));
#53865=CARTESIAN_POINT('',(11.5,1.00000000000001,30.));
#53866=CARTESIAN_POINT('',(11.2071067811865,6.53289321881345,30.));
#53867=CARTESIAN_POINT('Origin',(10.5,5.8257864376269,30.));
#53868=CARTESIAN_POINT('',(8.19644660940673,9.54355339059324,30.));
#53869=CARTESIAN_POINT('',(11.5,6.24,30.));
#53870=CARTESIAN_POINT('',(8.05,9.89710678118651,30.));
#53871=CARTESIAN_POINT('Origin',(8.55,9.89710678118651,30.));
#53872=CARTESIAN_POINT('',(8.05,13.5928932188135,30.));
#53873=CARTESIAN_POINT('',(8.05,9.68999999999997,30.));
#53874=CARTESIAN_POINT('',(8.19644660940672,13.9464466094067,30.));
#53875=CARTESIAN_POINT('Origin',(8.55,13.5928932188135,30.));
#53876=CARTESIAN_POINT('',(8.57259699813414,14.3225969981341,30.));
#53877=CARTESIAN_POINT('',(8.05,13.8,30.));
#53878=CARTESIAN_POINT('',(8.71475010619428,14.6107663907404,30.));
#53879=CARTESIAN_POINT('Origin',(8.21904360754086,14.6761503887274,30.));
#53880=CARTESIAN_POINT('',(10.6942336092596,16.5902498938057,30.));
#53881=CARTESIAN_POINT('Origin',(10.995,14.31,30.));
#53882=CARTESIAN_POINT('',(10.9824030018658,16.7324030018659,30.));
#53883=CARTESIAN_POINT('Origin',(10.6288496112726,17.0859563924591,30.));
#53884=CARTESIAN_POINT('',(11.3535533905933,17.1035533905933,30.));
#53885=CARTESIAN_POINT('',(8.05,13.8,30.));
#53886=CARTESIAN_POINT('',(11.5,17.4571067811866,30.));
#53887=CARTESIAN_POINT('Origin',(11.,17.4571067811866,30.));
#53888=CARTESIAN_POINT('',(11.5,18.3428932188135,30.));
#53889=CARTESIAN_POINT('',(11.5,18.55,30.));
#53890=CARTESIAN_POINT('',(11.3535533905933,18.6964466094068,30.));
#53891=CARTESIAN_POINT('Origin',(11.,18.3428932188135,30.));
#53892=CARTESIAN_POINT('',(10.9824030018659,19.0675969981341,30.));
#53893=CARTESIAN_POINT('',(8.05,22.,30.));
#53894=CARTESIAN_POINT('',(10.6942336092596,19.2097501061943,30.));
#53895=CARTESIAN_POINT('Origin',(10.6288496112726,18.7140436075409,30.));
#53896=CARTESIAN_POINT('',(8.71475010619428,21.1892336092596,30.));
#53897=CARTESIAN_POINT('Origin',(10.995,21.49,30.));
#53898=CARTESIAN_POINT('',(8.57259699813413,21.4774030018659,30.));
#53899=CARTESIAN_POINT('Origin',(8.21904360754086,21.1238496112726,30.));
#53900=CARTESIAN_POINT('',(8.05,22.,30.));
#53901=CARTESIAN_POINT('',(8.05,22.,30.));
#53902=CARTESIAN_POINT('',(-8.05,22.,30.));
#53903=CARTESIAN_POINT('',(-8.05,22.,30.));
#53904=CARTESIAN_POINT('',(-8.57259699813413,21.4774030018659,30.));
#53905=CARTESIAN_POINT('',(-8.05,22.,30.));
#53906=CARTESIAN_POINT('',(-8.71475010619428,21.1892336092596,30.));
#53907=CARTESIAN_POINT('Origin',(-8.21904360754086,21.1238496112726,30.));
#53908=CARTESIAN_POINT('',(-10.6942336092596,19.2097501061943,30.));
#53909=CARTESIAN_POINT('Origin',(-10.995,21.49,30.));
#53910=CARTESIAN_POINT('',(-10.9824030018659,19.0675969981341,30.));
#53911=CARTESIAN_POINT('Origin',(-10.6288496112726,18.7140436075409,30.));
#53912=CARTESIAN_POINT('',(-11.3535533905933,18.6964466094068,30.));
#53913=CARTESIAN_POINT('',(-8.05,22.,30.));
#53914=CARTESIAN_POINT('',(-11.5,18.3428932188135,30.));
#53915=CARTESIAN_POINT('Origin',(-11.,18.3428932188135,30.));
#53916=CARTESIAN_POINT('',(-11.5,17.4571067811866,30.));
#53917=CARTESIAN_POINT('',(-11.5,18.55,30.));
#53918=CARTESIAN_POINT('',(-11.3535533905933,17.1035533905933,30.));
#53919=CARTESIAN_POINT('Origin',(-11.,17.4571067811866,30.));
#53920=CARTESIAN_POINT('',(-10.9824030018658,16.7324030018659,30.));
#53921=CARTESIAN_POINT('',(-8.05,13.8,30.));
#53922=CARTESIAN_POINT('',(-10.6942336092596,16.5902498938057,30.));
#53923=CARTESIAN_POINT('Origin',(-10.6288496112726,17.0859563924591,30.));
#53924=CARTESIAN_POINT('',(-8.71475010619428,14.6107663907404,30.));
#53925=CARTESIAN_POINT('Origin',(-10.995,14.31,30.));
#53926=CARTESIAN_POINT('',(-8.57259699813414,14.3225969981341,30.));
#53927=CARTESIAN_POINT('Origin',(-8.21904360754086,14.6761503887274,30.));
#53928=CARTESIAN_POINT('',(-8.19644660940672,13.9464466094067,30.));
#53929=CARTESIAN_POINT('',(-8.05,13.8,30.));
#53930=CARTESIAN_POINT('',(-8.05,13.5928932188135,30.));
#53931=CARTESIAN_POINT('Origin',(-8.55,13.5928932188135,30.));
#53932=CARTESIAN_POINT('',(-8.05,9.89710678118651,30.));
#53933=CARTESIAN_POINT('',(-8.05,9.68999999999997,30.));
#53934=CARTESIAN_POINT('',(-8.19644660940673,9.54355339059324,30.));
#53935=CARTESIAN_POINT('Origin',(-8.55,9.89710678118651,30.));
#53936=CARTESIAN_POINT('',(-11.2071067811865,6.53289321881345,30.));
#53937=CARTESIAN_POINT('',(-11.5,6.24,30.));
#53938=CARTESIAN_POINT('',(-11.5,5.8257864376269,30.));
#53939=CARTESIAN_POINT('Origin',(-10.5,5.8257864376269,30.));
#53940=CARTESIAN_POINT('',(-11.5,1.00000000000001,30.));
#53941=CARTESIAN_POINT('',(-11.5,1.00000000000001,30.));
#53942=CARTESIAN_POINT('',(-10.5,-1.28587913910472E-15,30.));
#53943=CARTESIAN_POINT('Origin',(8.05,13.8,-450.));
#53944=CARTESIAN_POINT('',(8.19644660940672,13.9464466094067,-450.));
#53945=CARTESIAN_POINT('',(8.57259699813414,14.3225969981341,30.));
#53946=CARTESIAN_POINT('Origin',(8.05,13.8,-450.));
#53947=CARTESIAN_POINT('',(11.3535533905933,17.1035533905933,-450.));
#53948=CARTESIAN_POINT('',(10.9824030018658,16.7324030018659,-450.));
#53949=CARTESIAN_POINT('Origin',(8.05,22.,-450.));
#53950=CARTESIAN_POINT('',(10.9824030018659,19.0675969981341,30.));
#53951=CARTESIAN_POINT('',(11.3535533905933,18.6964466094068,-450.));
#53952=CARTESIAN_POINT('Origin',(8.05,22.,-450.));
#53953=CARTESIAN_POINT('',(8.57259699813413,21.4774030018659,-450.));
#53954=CARTESIAN_POINT('',(8.05,22.,-450.));
#53955=CARTESIAN_POINT('Origin',(-8.05,13.8,-450.));
#53956=CARTESIAN_POINT('',(-8.19644660940672,13.9464466094067,30.));
#53957=CARTESIAN_POINT('',(-8.57259699813414,14.3225969981341,-450.));
#53958=CARTESIAN_POINT('Origin',(-8.05,22.,-450.));
#53959=CARTESIAN_POINT('',(-10.9824030018659,19.0675969981341,-450.));
#53960=CARTESIAN_POINT('',(-11.3535533905933,18.6964466094068,-450.));
#53961=CARTESIAN_POINT('Origin',(-8.05,22.,-450.));
#53962=CARTESIAN_POINT('',(-8.05,22.,-450.));
#53963=CARTESIAN_POINT('Origin',(-10.5,-1.28587913910472E-15,-450.));
#53964=CARTESIAN_POINT('',(-11.5,1.00000000000001,-450.));
#53965=CARTESIAN_POINT('Origin',(-11.5,1.00000000000001,-450.));
#53966=CARTESIAN_POINT('',(-11.5,5.8257864376269,-450.));
#53967=CARTESIAN_POINT('Origin',(-11.5,6.24,-450.));
#53968=CARTESIAN_POINT('',(-11.2071067811865,6.53289321881345,-450.));
#53969=CARTESIAN_POINT('',(-8.19644660940673,9.54355339059324,-450.));
#53970=CARTESIAN_POINT('Origin',(-8.05,9.68999999999997,-450.));
#53971=CARTESIAN_POINT('',(-8.05,9.89710678118651,30.));
#53972=CARTESIAN_POINT('',(-8.05,13.5928932188135,-450.));
#53973=CARTESIAN_POINT('Origin',(-8.05,13.8,-450.));
#53974=CARTESIAN_POINT('',(-11.3535533905933,17.1035533905933,-450.));
#53975=CARTESIAN_POINT('',(-10.9824030018658,16.7324030018659,30.));
#53976=CARTESIAN_POINT('Origin',(-11.5,18.55,-450.));
#53977=CARTESIAN_POINT('',(-11.5,18.3428932188135,-450.));
#53978=CARTESIAN_POINT('',(-11.5,17.4571067811866,-450.));
#53979=CARTESIAN_POINT('Origin',(-8.05,22.,-450.));
#53980=CARTESIAN_POINT('',(-8.57259699813413,21.4774030018659,30.));
#53981=CARTESIAN_POINT('Origin',(-10.995,21.49,-450.));
#53982=CARTESIAN_POINT('',(-10.6942336092596,19.2097501061943,-450.));
#53983=CARTESIAN_POINT('',(-8.71475010619428,21.1892336092596,-450.));
#53984=CARTESIAN_POINT('Origin',(-10.995,14.31,-450.));
#53985=CARTESIAN_POINT('',(-10.6942336092596,16.5902498938057,-450.));
#53986=CARTESIAN_POINT('',(-8.71475010619428,14.6107663907404,-450.));
#53987=CARTESIAN_POINT('Origin',(-10.6288496112726,18.7140436075409,-450.));
#53988=CARTESIAN_POINT('Origin',(-11.,18.3428932188135,-450.));
#53989=CARTESIAN_POINT('Origin',(-11.,17.4571067811866,-450.));
#53990=CARTESIAN_POINT('Origin',(-10.6288496112726,17.0859563924591,-450.));
#53991=CARTESIAN_POINT('Origin',(-8.55,9.89710678118651,-450.));
#53992=CARTESIAN_POINT('Origin',(-8.55,13.5928932188135,-450.));
#53993=CARTESIAN_POINT('Origin',(-8.21904360754086,14.6761503887274,-450.));
#53994=CARTESIAN_POINT('Origin',(-8.21904360754086,21.1238496112726,-450.));
#53995=CARTESIAN_POINT('Origin',(-10.5,5.8257864376269,-450.));
#53996=CARTESIAN_POINT('Origin',(11.5,18.55,-450.));
#53997=CARTESIAN_POINT('',(11.5,18.3428932188135,-450.));
#53998=CARTESIAN_POINT('',(11.5,17.4571067811866,-450.));
#53999=CARTESIAN_POINT('Origin',(8.05,9.68999999999997,-450.));
#54000=CARTESIAN_POINT('',(8.05,9.89710678118651,-450.));
#54001=CARTESIAN_POINT('',(8.05,13.5928932188135,30.));
#54002=CARTESIAN_POINT('Origin',(11.5,6.24,-450.));
#54003=CARTESIAN_POINT('',(11.2071067811865,6.53289321881345,-450.));
#54004=CARTESIAN_POINT('',(8.19644660940673,9.54355339059324,30.));
#54005=CARTESIAN_POINT('Origin',(11.5,1.00000000000001,-450.));
#54006=CARTESIAN_POINT('',(11.5,5.8257864376269,-450.));
#54007=CARTESIAN_POINT('',(11.5,1.00000000000001,-450.));
#54008=CARTESIAN_POINT('Origin',(10.5,-1.28587913910472E-15,-450.));
#54009=CARTESIAN_POINT('Origin',(10.995,21.49,-450.));
#54010=CARTESIAN_POINT('',(10.6942336092596,19.2097501061943,-450.));
#54011=CARTESIAN_POINT('',(8.71475010619428,21.1892336092596,-450.));
#54012=CARTESIAN_POINT('Origin',(10.995,14.31,-450.));
#54013=CARTESIAN_POINT('',(10.6942336092596,16.5902498938057,-450.));
#54014=CARTESIAN_POINT('',(8.71475010619428,14.6107663907404,-450.));
#54015=CARTESIAN_POINT('Origin',(10.6288496112726,18.7140436075409,-450.));
#54016=CARTESIAN_POINT('Origin',(11.,18.3428932188135,-450.));
#54017=CARTESIAN_POINT('Origin',(11.,17.4571067811866,-450.));
#54018=CARTESIAN_POINT('Origin',(10.6288496112726,17.0859563924591,-450.));
#54019=CARTESIAN_POINT('Origin',(8.55,9.89710678118651,-450.));
#54020=CARTESIAN_POINT('Origin',(8.55,13.5928932188135,-450.));
#54021=CARTESIAN_POINT('Origin',(8.21904360754086,14.6761503887274,-450.));
#54022=CARTESIAN_POINT('Origin',(8.21904360754086,21.1238496112726,-450.));
#54023=CARTESIAN_POINT('Origin',(10.5,5.8257864376269,-450.));
#54024=CARTESIAN_POINT('Origin',(-2.25,-1.4389599889981E-16,-450.));
#54025=CARTESIAN_POINT('Origin',(-1.75,0.5,-450.));
#54026=CARTESIAN_POINT('',(1.75,0.5,-450.));
#54027=CARTESIAN_POINT('Origin',(1.75,0.5,-450.));
#54028=CARTESIAN_POINT('Origin',(3.5,13.,0.));
#54029=CARTESIAN_POINT('Origin',(3.5,13.,-60.));
#54030=CARTESIAN_POINT('Origin',(3.5,13.,-120.));
#54031=CARTESIAN_POINT('Origin',(3.5,13.,-180.));
#54032=CARTESIAN_POINT('Origin',(3.5,13.,-240.));
#54033=CARTESIAN_POINT('Origin',(3.5,13.,-300.));
#54034=CARTESIAN_POINT('Origin',(3.5,13.,-360.));
#54035=CARTESIAN_POINT('Origin',(3.5,13.,-420.));
#54036=CARTESIAN_POINT('',(0.,0.,0.));
#54037=CARTESIAN_POINT('Origin',(23.2,9.00000000000001,-77.4));
#54038=CARTESIAN_POINT('',(17.28,9.00000000000001,-74.9));
#54039=CARTESIAN_POINT('Origin',(17.28,9.00000000000001,-77.4));
#54040=CARTESIAN_POINT('',(23.2,9.00000000000001,-74.9));
#54041=CARTESIAN_POINT('',(23.2,9.00000000000001,-74.9));
#54042=CARTESIAN_POINT('Origin',(23.2,9.00000000000001,-77.4));
#54043=CARTESIAN_POINT('Origin',(-23.2,9.00000000000001,-77.4));
#54044=CARTESIAN_POINT('',(-17.28,9.00000000000001,-79.9));
#54045=CARTESIAN_POINT('Origin',(-17.28,9.00000000000001,-77.4));
#54046=CARTESIAN_POINT('',(-23.2,9.00000000000001,-79.9));
#54047=CARTESIAN_POINT('',(-23.2,9.00000000000001,-79.9));
#54048=CARTESIAN_POINT('Origin',(-23.2,9.00000000000001,-77.4));
#54049=CARTESIAN_POINT('Origin',(-1.54689479616415E-14,13.,-76.7));
#54050=CARTESIAN_POINT('',(3.64999999999998,13.,-76.7));
#54051=CARTESIAN_POINT('Origin',(-1.54689479616415E-14,13.,-76.7));
#54052=CARTESIAN_POINT('',(3.64999999999998,13.8,-76.7));
#54053=CARTESIAN_POINT('',(3.64999999999998,13.,-76.7));
#54054=CARTESIAN_POINT('Origin',(-1.65097820472275E-14,13.8,-76.7));
#54055=CARTESIAN_POINT('Origin',(17.28,9.00000000000001,-77.4));
#54056=CARTESIAN_POINT('',(15.7778484524311,9.,-77.4));
#54057=CARTESIAN_POINT('',(17.28,9.00000000000001,-74.9));
#54058=CARTESIAN_POINT('Origin',(-17.28,9.00000000000001,-77.4));
#54059=CARTESIAN_POINT('',(-15.7778484524311,9.,-77.4));
#54060=CARTESIAN_POINT('',(-17.28,9.00000000000001,-79.9));
#54061=CARTESIAN_POINT('Origin',(28.5,14.,-64.9));
#54062=CARTESIAN_POINT('',(28.5,0.500000000000005,-68.2235));
#54063=CARTESIAN_POINT('Origin',(28.5,0.500000000000006,-64.9));
#54064=CARTESIAN_POINT('',(28.5,14.,-68.2235));
#54065=CARTESIAN_POINT('',(28.5,14.,-68.2235));
#54066=CARTESIAN_POINT('Origin',(28.5,14.,-64.9));
#54067=CARTESIAN_POINT('Origin',(28.5,14.,-19.9));
#54068=CARTESIAN_POINT('',(28.5,0.500000000000005,-23.2235));
#54069=CARTESIAN_POINT('Origin',(28.5,0.500000000000006,-19.9));
#54070=CARTESIAN_POINT('',(28.5,14.,-23.2235));
#54071=CARTESIAN_POINT('',(28.5,14.,-23.2235));
#54072=CARTESIAN_POINT('Origin',(28.5,14.,-19.9));
#54073=CARTESIAN_POINT('Origin',(-28.5,14.,-64.9));
#54074=CARTESIAN_POINT('',(-28.5,0.500000000000005,-68.2235));
#54075=CARTESIAN_POINT('Origin',(-28.5,0.500000000000006,-64.9));
#54076=CARTESIAN_POINT('',(-28.5,14.,-68.2235));
#54077=CARTESIAN_POINT('',(-28.5,14.,-68.2235));
#54078=CARTESIAN_POINT('Origin',(-28.5,14.,-64.9));
#54079=CARTESIAN_POINT('Origin',(-28.5,14.,-19.9));
#54080=CARTESIAN_POINT('',(-28.5,0.500000000000003,-23.2235));
#54081=CARTESIAN_POINT('Origin',(-28.5,0.500000000000004,-19.9));
#54082=CARTESIAN_POINT('',(-28.5,14.,-23.2235));
#54083=CARTESIAN_POINT('',(-28.5,14.,-23.2235));
#54084=CARTESIAN_POINT('Origin',(-28.5,14.,-19.9));
#54085=CARTESIAN_POINT('Origin',(-23.2,9.00000000000001,-7.4));
#54086=CARTESIAN_POINT('',(-17.28,9.00000000000001,-9.9));
#54087=CARTESIAN_POINT('Origin',(-17.28,9.00000000000001,-7.4));
#54088=CARTESIAN_POINT('',(-23.2,9.00000000000001,-9.9));
#54089=CARTESIAN_POINT('',(-23.2,9.00000000000001,-9.9));
#54090=CARTESIAN_POINT('Origin',(-23.2,9.00000000000001,-7.4));
#54091=CARTESIAN_POINT('Origin',(23.2,9.00000000000001,-7.4));
#54092=CARTESIAN_POINT('',(17.28,9.00000000000001,-4.90000000000001));
#54093=CARTESIAN_POINT('Origin',(17.28,9.00000000000001,-7.4));
#54094=CARTESIAN_POINT('',(23.2,9.00000000000001,-4.90000000000001));
#54095=CARTESIAN_POINT('',(23.2,9.00000000000001,-4.90000000000001));
#54096=CARTESIAN_POINT('Origin',(23.2,9.00000000000001,-7.4));
#54097=CARTESIAN_POINT('Origin',(-1.54689479616415E-14,13.,-8.1));
#54098=CARTESIAN_POINT('',(3.64999999999998,13.,-8.1));
#54099=CARTESIAN_POINT('Origin',(-1.54689479616415E-14,13.,-8.1));
#54100=CARTESIAN_POINT('',(3.64999999999998,13.8,-8.1));
#54101=CARTESIAN_POINT('',(3.64999999999998,13.,-8.1));
#54102=CARTESIAN_POINT('Origin',(-1.65097820472275E-14,13.8,-8.1));
#54103=CARTESIAN_POINT('Origin',(-1.90276438129354E-14,12.7,-74.2));
#54104=CARTESIAN_POINT('',(0.499999999999987,12.5,-74.2));
#54105=CARTESIAN_POINT('Origin',(-1.87674352915389E-14,12.5,-74.2));
#54106=CARTESIAN_POINT('',(0.499999999999987,12.7,-74.2));
#54107=CARTESIAN_POINT('',(0.499999999999987,12.7,-74.2));
#54108=CARTESIAN_POINT('',(-0.500000000000023,12.7,-74.2));
#54109=CARTESIAN_POINT('Origin',(-1.90276438129354E-14,12.7,-74.2));
#54110=CARTESIAN_POINT('',(-0.500000000000025,13.,-74.2));
#54111=CARTESIAN_POINT('',(-0.500000000000025,12.7,-74.2));
#54112=CARTESIAN_POINT('',(0.499999999999986,13.,-74.2));
#54113=CARTESIAN_POINT('Origin',(-1.94179565950302E-14,13.,-74.2));
#54114=CARTESIAN_POINT('',(0.499999999999987,12.7,-74.2));
#54115=CARTESIAN_POINT('Origin',(-17.28,9.00000000000001,-7.4));
#54116=CARTESIAN_POINT('',(-15.7778484524311,9.,-7.4));
#54117=CARTESIAN_POINT('',(-17.28,9.00000000000001,-9.9));
#54118=CARTESIAN_POINT('Origin',(17.28,9.00000000000001,-7.4));
#54119=CARTESIAN_POINT('',(15.7778484524311,9.,-7.4));
#54120=CARTESIAN_POINT('',(17.28,9.00000000000001,-4.90000000000001));
#54121=CARTESIAN_POINT('Origin',(-1.65232411086791E-14,12.7,-10.6));
#54122=CARTESIAN_POINT('',(0.499999999999984,12.5,-10.6));
#54123=CARTESIAN_POINT('Origin',(-1.62630325872826E-14,12.5,-10.6));
#54124=CARTESIAN_POINT('',(0.499999999999984,12.7,-10.6));
#54125=CARTESIAN_POINT('',(0.499999999999984,12.7,-10.6));
#54126=CARTESIAN_POINT('',(0.499999999999983,13.,-10.6));
#54127=CARTESIAN_POINT('',(0.499999999999984,12.7,-10.6));
#54128=CARTESIAN_POINT('',(-0.500000000000017,13.,-10.6));
#54129=CARTESIAN_POINT('Origin',(-1.69135538907739E-14,13.,-10.6));
#54130=CARTESIAN_POINT('',(-0.500000000000017,12.7,-10.6));
#54131=CARTESIAN_POINT('',(-0.500000000000017,12.7,-10.6));
#54132=CARTESIAN_POINT('Origin',(-1.65232411086791E-14,12.7,-10.6));
#54133=CARTESIAN_POINT('Ctrl Pts',(4.,8.,-84.5));
#54134=CARTESIAN_POINT('Ctrl Pts',(4.,4.,-84.5));
#54135=CARTESIAN_POINT('Ctrl Pts',(0.,4.,-84.5));
#54136=CARTESIAN_POINT('Ctrl Pts',(-4.,4.,-84.5));
#54137=CARTESIAN_POINT('Ctrl Pts',(-4.,8.,-84.5));
#54138=CARTESIAN_POINT('Ctrl Pts',(-4.,12.,-84.5));
#54139=CARTESIAN_POINT('Ctrl Pts',(0.,12.,-84.5));
#54140=CARTESIAN_POINT('Ctrl Pts',(4.,12.,-84.5));
#54141=CARTESIAN_POINT('Ctrl Pts',(4.,8.,-84.5));
#54142=CARTESIAN_POINT('Ctrl Pts',(4.,8.,-86.5172334444062));
#54143=CARTESIAN_POINT('Ctrl Pts',(4.,4.,-86.5172334444062));
#54144=CARTESIAN_POINT('Ctrl Pts',(0.,4.,-86.5172334444062));
#54145=CARTESIAN_POINT('Ctrl Pts',(-4.,4.,-86.5172334444062));
#54146=CARTESIAN_POINT('Ctrl Pts',(-4.,8.,-86.5172334444062));
#54147=CARTESIAN_POINT('Ctrl Pts',(-4.,12.,-86.5172334444062));
#54148=CARTESIAN_POINT('Ctrl Pts',(0.,12.,-86.5172334444062));
#54149=CARTESIAN_POINT('Ctrl Pts',(4.,12.,-86.5172334444062));
#54150=CARTESIAN_POINT('Ctrl Pts',(4.,8.,-86.5172334444062));
#54151=CARTESIAN_POINT('Ctrl Pts',(2.,8.,-86.7803508501983));
#54152=CARTESIAN_POINT('Ctrl Pts',(2.,6.,-86.7803508501983));
#54153=CARTESIAN_POINT('Ctrl Pts',(0.,6.,-86.7803508501983));
#54154=CARTESIAN_POINT('Ctrl Pts',(-2.,6.,-86.7803508501983));
#54155=CARTESIAN_POINT('Ctrl Pts',(-2.,8.,-86.7803508501983));
#54156=CARTESIAN_POINT('Ctrl Pts',(-2.,10.,-86.7803508501983));
#54157=CARTESIAN_POINT('Ctrl Pts',(0.,10.,-86.7803508501983));
#54158=CARTESIAN_POINT('Ctrl Pts',(2.,10.,-86.7803508501983));
#54159=CARTESIAN_POINT('Ctrl Pts',(2.,8.,-86.7803508501983));
#54160=CARTESIAN_POINT('',(-1.15470053837925,6.,-86.7177985317981));
#54161=CARTESIAN_POINT('',(-2.3094010767585,8.,-86.7177985317981));
#54162=CARTESIAN_POINT('Ctrl Pts',(-1.15470053837925,6.,-86.7177985317981));
#54163=CARTESIAN_POINT('Ctrl Pts',(-1.16052376017366,6.01008611601166,-86.7193986219689));
#54164=CARTESIAN_POINT('Ctrl Pts',(-1.16635206467311,6.02018103552669,-86.7209572835343));
#54165=CARTESIAN_POINT('Ctrl Pts',(-1.36167110655042,6.35848353974387,-86.7717992509189));
#54166=CARTESIAN_POINT('Ctrl Pts',(-1.5557141858025,6.69457601186558,-86.7803508501983));
#54167=CARTESIAN_POINT('Ctrl Pts',(-1.90838742933526,7.30542398813443,-86.7803508501983));
#54168=CARTESIAN_POINT('Ctrl Pts',(-2.10243050858733,7.64151646025614,-86.7717992509189));
#54169=CARTESIAN_POINT('Ctrl Pts',(-2.29774955046464,7.97981896447331,-86.7209572835343));
#54170=CARTESIAN_POINT('Ctrl Pts',(-2.3035778549641,7.98991388398835,-86.7193986219689));
#54171=CARTESIAN_POINT('Ctrl Pts',(-2.30940107675851,8.00000000000001,-86.7177985317981));
#54172=CARTESIAN_POINT('',(1.15470053837925,6.,-86.7177985317981));
#54173=CARTESIAN_POINT('Ctrl Pts',(1.15470053837925,6.,-86.7177985317981));
#54174=CARTESIAN_POINT('Ctrl Pts',(1.14305409479044,6.,-86.7193986219689));
#54175=CARTESIAN_POINT('Ctrl Pts',(1.13139748579153,6.,-86.7209572835343));
#54176=CARTESIAN_POINT('Ctrl Pts',(0.740759402036912,6.,-86.7717992509189));
#54177=CARTESIAN_POINT('Ctrl Pts',(0.352673243532761,6.,-86.7803508501983));
#54178=CARTESIAN_POINT('Ctrl Pts',(-0.352673243532758,6.,-86.7803508501983));
#54179=CARTESIAN_POINT('Ctrl Pts',(-0.740759402036907,6.,-86.7717992509189));
#54180=CARTESIAN_POINT('Ctrl Pts',(-1.13139748579153,6.,-86.7209572835343));
#54181=CARTESIAN_POINT('Ctrl Pts',(-1.14305409479043,6.,-86.7193986219689));
#54182=CARTESIAN_POINT('Ctrl Pts',(-1.15470053837925,6.,-86.7177985317981));
#54183=CARTESIAN_POINT('',(2.3094010767585,8.,-86.7177985317981));
#54184=CARTESIAN_POINT('Ctrl Pts',(2.3094010767585,8.,-86.7177985317981));
#54185=CARTESIAN_POINT('Ctrl Pts',(2.30357785496409,7.98991388398834,-86.7193986219689));
#54186=CARTESIAN_POINT('Ctrl Pts',(2.29774955046465,7.97981896447331,-86.7209572835343));
#54187=CARTESIAN_POINT('Ctrl Pts',(2.10243050858733,7.64151646025614,-86.7717992509189));
#54188=CARTESIAN_POINT('Ctrl Pts',(1.90838742933526,7.30542398813443,-86.7803508501983));
#54189=CARTESIAN_POINT('Ctrl Pts',(1.5557141858025,6.69457601186558,-86.7803508501983));
#54190=CARTESIAN_POINT('Ctrl Pts',(1.36167110655042,6.35848353974387,-86.7717992509189));
#54191=CARTESIAN_POINT('Ctrl Pts',(1.16635206467311,6.02018103552669,-86.7209572835344));
#54192=CARTESIAN_POINT('Ctrl Pts',(1.16052376017366,6.01008611601166,-86.7193986219689));
#54193=CARTESIAN_POINT('Ctrl Pts',(1.15470053837925,6.00000000000001,-86.7177985317981));
#54194=CARTESIAN_POINT('',(4.,8.,-84.5));
#54195=CARTESIAN_POINT('Ctrl Pts',(2.3094010767585,8.,-86.7177985317981));
#54196=CARTESIAN_POINT('Ctrl Pts',(4.,8.,-86.2532600313803));
#54197=CARTESIAN_POINT('Ctrl Pts',(4.,8.,-84.5));
#54198=CARTESIAN_POINT('',(-4.,8.,-84.5));
#54199=CARTESIAN_POINT('Origin',(0.,8.,-84.5));
#54200=CARTESIAN_POINT('Origin',(0.,8.,-84.5));
#54201=CARTESIAN_POINT('',(1.15470053837925,10.,-86.7177985317981));
#54202=CARTESIAN_POINT('Ctrl Pts',(1.15470053837925,10.,-86.7177985317981));
#54203=CARTESIAN_POINT('Ctrl Pts',(1.16052376017366,9.98991388398835,-86.7193986219689));
#54204=CARTESIAN_POINT('Ctrl Pts',(1.16635206467311,9.97981896447332,-86.7209572835343));
#54205=CARTESIAN_POINT('Ctrl Pts',(1.36167110655042,9.64151646025614,-86.7717992509189));
#54206=CARTESIAN_POINT('Ctrl Pts',(1.5557141858025,9.30542398813443,-86.7803508501983));
#54207=CARTESIAN_POINT('Ctrl Pts',(1.90838742933526,8.69457601186558,-86.7803508501983));
#54208=CARTESIAN_POINT('Ctrl Pts',(2.10243050858733,8.35848353974387,-86.7717992509189));
#54209=CARTESIAN_POINT('Ctrl Pts',(2.29774955046465,8.02018103552669,-86.7209572835343));
#54210=CARTESIAN_POINT('Ctrl Pts',(2.3035778549641,8.01008611601166,-86.7193986219689));
#54211=CARTESIAN_POINT('Ctrl Pts',(2.30940107675851,8.,-86.7177985317981));
#54212=CARTESIAN_POINT('',(-1.15470053837925,10.,-86.7177985317981));
#54213=CARTESIAN_POINT('Ctrl Pts',(-1.15470053837925,10.,-86.7177985317981));
#54214=CARTESIAN_POINT('Ctrl Pts',(-1.14305409479043,10.,-86.7193986219689));
#54215=CARTESIAN_POINT('Ctrl Pts',(-1.13139748579153,10.,-86.7209572835343));
#54216=CARTESIAN_POINT('Ctrl Pts',(-0.740759402036911,10.,-86.7717992509189));
#54217=CARTESIAN_POINT('Ctrl Pts',(-0.352673243532759,10.,-86.7803508501983));
#54218=CARTESIAN_POINT('Ctrl Pts',(0.352673243532759,10.,-86.7803508501983));
#54219=CARTESIAN_POINT('Ctrl Pts',(0.740759402036911,10.,-86.7717992509189));
#54220=CARTESIAN_POINT('Ctrl Pts',(1.13139748579153,10.,-86.7209572835343));
#54221=CARTESIAN_POINT('Ctrl Pts',(1.14305409479044,10.,-86.7193986219689));
#54222=CARTESIAN_POINT('Ctrl Pts',(1.15470053837925,10.,-86.7177985317981));
#54223=CARTESIAN_POINT('Ctrl Pts',(-2.3094010767585,8.,-86.7177985317981));
#54224=CARTESIAN_POINT('Ctrl Pts',(-2.3035778549641,8.01008611601166,-86.7193986219689));
#54225=CARTESIAN_POINT('Ctrl Pts',(-2.29774955046464,8.02018103552669,-86.7209572835343));
#54226=CARTESIAN_POINT('Ctrl Pts',(-2.10243050858733,8.35848353974387,-86.7717992509189));
#54227=CARTESIAN_POINT('Ctrl Pts',(-1.90838742933526,8.69457601186558,-86.7803508501983));
#54228=CARTESIAN_POINT('Ctrl Pts',(-1.5557141858025,9.30542398813443,-86.7803508501983));
#54229=CARTESIAN_POINT('Ctrl Pts',(-1.36167110655042,9.64151646025614,-86.7717992509189));
#54230=CARTESIAN_POINT('Ctrl Pts',(-1.16635206467311,9.97981896447332,-86.7209572835343));
#54231=CARTESIAN_POINT('Ctrl Pts',(-1.16052376017366,9.98991388398835,-86.7193986219689));
#54232=CARTESIAN_POINT('Ctrl Pts',(-1.15470053837925,10.,-86.7177985317981));
#54233=CARTESIAN_POINT('Origin',(0.,8.,-86.8));
#54234=CARTESIAN_POINT('',(-4.,8.,-83.8));
#54235=CARTESIAN_POINT('Origin',(0.,8.,-83.8));
#54236=CARTESIAN_POINT('',(-4.,8.,-86.8));
#54237=CARTESIAN_POINT('Origin',(0.,8.,-83.8));
#54238=CARTESIAN_POINT('',(4.99995,8.,-83.8));
#54239=CARTESIAN_POINT('Origin',(0.,8.,-83.8));
#54240=CARTESIAN_POINT('',(4.99995,8.,-84.8));
#54241=CARTESIAN_POINT('',(4.99995,8.,-83.8));
#54242=CARTESIAN_POINT('Origin',(0.,8.,-84.8));
#54243=CARTESIAN_POINT('Origin',(25.4958861827765,-14.55,-104.175753233145));
#54244=CARTESIAN_POINT('',(23.,-16.5,-64.9));
#54245=CARTESIAN_POINT('',(25.4958861827765,-14.55,-69.5070923773207));
#54246=CARTESIAN_POINT('Origin',(28.4999999999971,-12.2029290542153,-64.9000000000014));
#54247=CARTESIAN_POINT('',(23.,-16.5,-71.4));
#54248=CARTESIAN_POINT('',(23.,-16.5,-84.8));
#54249=CARTESIAN_POINT('',(25.4958861827765,-14.55,-71.4));
#54250=CARTESIAN_POINT('',(25.4958861827765,-14.55,-71.4));
#54251=CARTESIAN_POINT('',(25.4958861827765,-14.55,-104.175753233145));
#54252=CARTESIAN_POINT('Origin',(25.4958861827765,-14.55,-104.175753233145));
#54253=CARTESIAN_POINT('',(25.4958861827765,-14.55,-60.2929076226793));
#54254=CARTESIAN_POINT('Origin',(28.5000000000002,-12.2029290542129,-64.9000000000003));
#54255=CARTESIAN_POINT('',(25.4958861827765,-14.55,-24.5070923773207));
#54256=CARTESIAN_POINT('',(25.4958861827765,-14.55,-104.175753233145));
#54257=CARTESIAN_POINT('',(23.,-16.5,-19.9));
#54258=CARTESIAN_POINT('Origin',(28.4999999999964,-12.2029290542158,-19.900000000002));
#54259=CARTESIAN_POINT('',(23.,-16.5,-84.8));
#54260=CARTESIAN_POINT('Origin',(-25.4958861827765,-14.55,-104.175753233145));
#54261=CARTESIAN_POINT('',(-23.,-16.5,-64.9));
#54262=CARTESIAN_POINT('',(-25.4958861827765,-14.55,-60.2929076226793));
#54263=CARTESIAN_POINT('Origin',(-28.5000000000003,-12.2029290542127,-64.9000000000003));
#54264=CARTESIAN_POINT('',(-23.,-16.5,-19.9));
#54265=CARTESIAN_POINT('',(-23.,-16.5,-84.8));
#54266=CARTESIAN_POINT('',(-25.4958861827765,-14.55,-24.5070923773207));
#54267=CARTESIAN_POINT('Origin',(-28.4999999999988,-12.2029290542139,-19.9000000000006));
#54268=CARTESIAN_POINT('',(-25.4958861827765,-14.55,-104.175753233145));
#54269=CARTESIAN_POINT('Origin',(-25.4958861827765,-14.55,-104.175753233145));
#54270=CARTESIAN_POINT('',(-25.4958861827765,-14.55,-15.2929076226793));
#54271=CARTESIAN_POINT('Origin',(-28.4999999999998,-12.2029290542132,-19.8999999999999));
#54272=CARTESIAN_POINT('',(-23.,-16.5,-13.4));
#54273=CARTESIAN_POINT('',(-23.,-16.5,-84.8));
#54274=CARTESIAN_POINT('',(-25.4958861827765,-14.55,-13.4));
#54275=CARTESIAN_POINT('',(-25.4958861827765,-14.55,-13.4));
#54276=CARTESIAN_POINT('',(-25.4958861827765,-14.55,-104.175753233145));
#54277=CARTESIAN_POINT('Origin',(8.05,-8.2,-84.8));
#54278=CARTESIAN_POINT('',(8.57259699813413,-7.67740300186587,-81.35));
#54279=CARTESIAN_POINT('',(8.19644660940673,-8.05355339059327,-81.35));
#54280=CARTESIAN_POINT('',(8.57259699813413,-7.67740300186587,-81.35));
#54281=CARTESIAN_POINT('',(8.57259699813413,-7.67740300186587,-84.8));
#54282=CARTESIAN_POINT('',(8.57259699813413,-7.67740300186587,-84.8));
#54283=CARTESIAN_POINT('',(8.19644660940673,-8.05355339059327,-84.8));
#54284=CARTESIAN_POINT('',(8.05,-8.2,-84.8));
#54285=CARTESIAN_POINT('',(8.19644660940673,-8.05355339059327,-84.8));
#54286=CARTESIAN_POINT('Origin',(8.05,3.67394039744206E-16,-84.8));
#54287=CARTESIAN_POINT('',(10.9824030018659,-2.93240300186586,-81.35));
#54288=CARTESIAN_POINT('',(11.3535533905933,-3.30355339059329,-81.35));
#54289=CARTESIAN_POINT('',(10.9824030018659,-2.93240300186586,-81.35));
#54290=CARTESIAN_POINT('',(10.9824030018659,-2.93240300186586,-84.8));
#54291=CARTESIAN_POINT('',(10.9824030018659,-2.93240300186586,-84.8));
#54292=CARTESIAN_POINT('',(11.3535533905933,-3.30355339059329,-84.8));
#54293=CARTESIAN_POINT('',(8.05,3.67394039744206E-16,-84.8));
#54294=CARTESIAN_POINT('',(11.3535533905933,-3.30355339059329,0.));
#54295=CARTESIAN_POINT('Origin',(-8.05,-8.2,-84.8));
#54296=CARTESIAN_POINT('',(-10.9824030018659,-5.26759699813413,-81.35));
#54297=CARTESIAN_POINT('',(-11.3535533905933,-4.89644660940674,-81.35));
#54298=CARTESIAN_POINT('',(-10.9824030018659,-5.26759699813413,-81.35));
#54299=CARTESIAN_POINT('',(-10.9824030018659,-5.26759699813413,-84.8));
#54300=CARTESIAN_POINT('',(-10.9824030018659,-5.26759699813413,-84.8));
#54301=CARTESIAN_POINT('',(-11.3535533905933,-4.89644660940674,-84.8));
#54302=CARTESIAN_POINT('',(-8.05,-8.2,-84.8));
#54303=CARTESIAN_POINT('',(-11.3535533905933,-4.89644660940674,0.));
#54304=CARTESIAN_POINT('Origin',(-8.05,-1.60428730688303E-15,-84.8));
#54305=CARTESIAN_POINT('',(-8.57259699813413,-0.522596998134137,-81.35));
#54306=CARTESIAN_POINT('',(-8.05,-1.60428730688303E-15,-81.35));
#54307=CARTESIAN_POINT('',(-8.57259699813413,-0.522596998134137,-81.35));
#54308=CARTESIAN_POINT('',(-8.57259699813413,-0.522596998134137,-84.8));
#54309=CARTESIAN_POINT('',(-8.57259699813413,-0.522596998134137,-84.8));
#54310=CARTESIAN_POINT('',(-8.05,-1.60428730688303E-15,-84.8));
#54311=CARTESIAN_POINT('',(-8.05,-1.60428730688303E-15,-84.8));
#54312=CARTESIAN_POINT('',(-8.05,-1.60428730688303E-15,-84.8));
#54313=CARTESIAN_POINT('Origin',(-8.05,-1.60428730688303E-15,-84.8));
#54314=CARTESIAN_POINT('',(-11.3535533905933,-3.30355339059329,-81.35));
#54315=CARTESIAN_POINT('',(-10.9824030018659,-2.93240300186587,-81.35));
#54316=CARTESIAN_POINT('',(-11.3535533905933,-3.30355339059329,-81.35));
#54317=CARTESIAN_POINT('',(-11.3535533905933,-3.30355339059329,-84.8));
#54318=CARTESIAN_POINT('',(-11.3535533905933,-3.30355339059329,-84.8));
#54319=CARTESIAN_POINT('',(-10.9824030018659,-2.93240300186587,-84.8));
#54320=CARTESIAN_POINT('',(-8.05,-1.60428730688303E-15,-84.8));
#54321=CARTESIAN_POINT('',(-10.9824030018659,-2.93240300186587,0.));
#54322=CARTESIAN_POINT('Origin',(-11.5,-4.75000000000001,-84.8));
#54323=CARTESIAN_POINT('',(-11.5,-4.54289321881346,-81.35));
#54324=CARTESIAN_POINT('',(-11.5,-3.65710678118656,-81.35));
#54325=CARTESIAN_POINT('',(-11.5,-4.54289321881346,-81.35));
#54326=CARTESIAN_POINT('',(-11.5,-4.54289321881346,-84.8));
#54327=CARTESIAN_POINT('',(-11.5,-4.54289321881346,-84.8));
#54328=CARTESIAN_POINT('',(-11.5,-3.65710678118656,-84.8));
#54329=CARTESIAN_POINT('',(-11.5,-4.75000000000001,-84.8));
#54330=CARTESIAN_POINT('',(-11.5,-3.65710678118656,0.));
#54331=CARTESIAN_POINT('Origin',(-8.05,-8.2,-84.8));
#54332=CARTESIAN_POINT('',(-8.19644660940673,-8.05355339059327,-81.35));
#54333=CARTESIAN_POINT('',(-8.57259699813413,-7.67740300186587,-81.35));
#54334=CARTESIAN_POINT('',(-8.19644660940673,-8.05355339059327,-81.35));
#54335=CARTESIAN_POINT('',(-8.19644660940673,-8.05355339059327,-84.8));
#54336=CARTESIAN_POINT('',(-8.19644660940673,-8.05355339059327,-84.8));
#54337=CARTESIAN_POINT('',(-8.57259699813413,-7.67740300186587,-84.8));
#54338=CARTESIAN_POINT('',(-8.05,-8.2,-84.8));
#54339=CARTESIAN_POINT('',(-8.57259699813413,-7.67740300186587,0.));
#54340=CARTESIAN_POINT('Origin',(-8.05,-12.24,-84.8));
#54341=CARTESIAN_POINT('',(-8.05,-12.0328932188134,-81.35));
#54342=CARTESIAN_POINT('',(-8.05,-8.40710678118654,-81.35));
#54343=CARTESIAN_POINT('',(-8.05,-12.0328932188134,-81.35));
#54344=CARTESIAN_POINT('',(-8.05,-12.0328932188134,-84.8));
#54345=CARTESIAN_POINT('',(-8.05,-12.0328932188134,-84.8));
#54346=CARTESIAN_POINT('',(-8.05,-8.40710678118654,-84.8));
#54347=CARTESIAN_POINT('',(-8.05,-12.24,-84.8));
#54348=CARTESIAN_POINT('',(-8.05,-8.40710678118654,-84.8));
#54349=CARTESIAN_POINT('Origin',(-12.31,-16.5,-84.8));
#54350=CARTESIAN_POINT('',(-12.31,-16.5,-81.35));
#54351=CARTESIAN_POINT('',(-8.19644660940672,-12.3864466094067,-81.35));
#54352=CARTESIAN_POINT('',(-12.31,-16.5,-81.35));
#54353=CARTESIAN_POINT('',(-12.31,-16.5,-84.8));
#54354=CARTESIAN_POINT('',(-12.31,-16.5,-84.8));
#54355=CARTESIAN_POINT('',(-8.19644660940672,-12.3864466094067,-84.8));
#54356=CARTESIAN_POINT('',(-12.31,-16.5,-84.8));
#54357=CARTESIAN_POINT('',(-8.19644660940672,-12.3864466094067,-84.8));
#54358=CARTESIAN_POINT('Origin',(-23.,-16.5,-84.8));
#54359=CARTESIAN_POINT('',(-22.2,-16.5,-81.35));
#54360=CARTESIAN_POINT('',(-22.2,-16.5,-81.35));
#54361=CARTESIAN_POINT('',(-22.2,-16.5,-84.8));
#54362=CARTESIAN_POINT('',(-22.2,-16.5,-84.8));
#54363=CARTESIAN_POINT('',(-23.,-16.5,-84.8));
#54364=CARTESIAN_POINT('Origin',(12.31,-16.5,-84.8));
#54365=CARTESIAN_POINT('',(12.31,-16.5,-81.35));
#54366=CARTESIAN_POINT('',(22.2,-16.5,-81.35));
#54367=CARTESIAN_POINT('',(12.31,-16.5,-81.35));
#54368=CARTESIAN_POINT('',(12.31,-16.5,-84.8));
#54369=CARTESIAN_POINT('',(12.31,-16.5,-84.8));
#54370=CARTESIAN_POINT('',(22.2,-16.5,-84.8));
#54371=CARTESIAN_POINT('',(12.31,-16.5,-84.8));
#54372=CARTESIAN_POINT('',(22.2,-16.5,-84.8));
#54373=CARTESIAN_POINT('Origin',(12.31,-16.5,-84.8));
#54374=CARTESIAN_POINT('',(8.19644660940673,-12.3864466094067,-81.35));
#54375=CARTESIAN_POINT('',(8.19644660940673,-12.3864466094067,-81.35));
#54376=CARTESIAN_POINT('',(8.19644660940673,-12.3864466094067,-84.8));
#54377=CARTESIAN_POINT('',(8.19644660940673,-12.3864466094067,-84.8));
#54378=CARTESIAN_POINT('',(12.31,-16.5,-84.8));
#54379=CARTESIAN_POINT('Origin',(8.05,-12.24,-84.8));
#54380=CARTESIAN_POINT('',(8.05,-8.40710678118654,-81.35));
#54381=CARTESIAN_POINT('',(8.05,-12.0328932188134,-81.35));
#54382=CARTESIAN_POINT('',(8.05,-8.40710678118654,-81.35));
#54383=CARTESIAN_POINT('',(8.05,-8.40710678118654,-84.8));
#54384=CARTESIAN_POINT('',(8.05,-8.40710678118654,-84.8));
#54385=CARTESIAN_POINT('',(8.05,-12.0328932188134,-84.8));
#54386=CARTESIAN_POINT('',(8.05,-12.24,-84.8));
#54387=CARTESIAN_POINT('',(8.05,-12.0328932188134,-84.8));
#54388=CARTESIAN_POINT('Origin',(8.05,-8.2,-84.8));
#54389=CARTESIAN_POINT('',(11.3535533905933,-4.89644660940673,-81.35));
#54390=CARTESIAN_POINT('',(10.9824030018659,-5.26759699813413,-81.35));
#54391=CARTESIAN_POINT('',(11.3535533905933,-4.89644660940673,-81.35));
#54392=CARTESIAN_POINT('',(11.3535533905933,-4.89644660940673,-84.8));
#54393=CARTESIAN_POINT('',(11.3535533905933,-4.89644660940673,-84.8));
#54394=CARTESIAN_POINT('',(10.9824030018659,-5.26759699813413,-84.8));
#54395=CARTESIAN_POINT('',(8.05,-8.2,-84.8));
#54396=CARTESIAN_POINT('',(10.9824030018659,-5.26759699813413,0.));
#54397=CARTESIAN_POINT('Origin',(11.5,-4.75000000000001,-84.8));
#54398=CARTESIAN_POINT('',(11.5,-3.65710678118656,-81.35));
#54399=CARTESIAN_POINT('',(11.5,-4.54289321881346,-81.35));
#54400=CARTESIAN_POINT('',(11.5,-3.65710678118656,-81.35));
#54401=CARTESIAN_POINT('',(11.5,-3.65710678118656,-84.8));
#54402=CARTESIAN_POINT('',(11.5,-3.65710678118656,-84.8));
#54403=CARTESIAN_POINT('',(11.5,-4.54289321881346,-84.8));
#54404=CARTESIAN_POINT('',(11.5,-4.75000000000001,-84.8));
#54405=CARTESIAN_POINT('',(11.5,-4.54289321881346,0.));
#54406=CARTESIAN_POINT('Origin',(8.05,3.67394039744206E-16,-84.8));
#54407=CARTESIAN_POINT('',(8.05,3.67394039744206E-16,-81.35));
#54408=CARTESIAN_POINT('',(8.57259699813413,-0.522596998134133,-81.35));
#54409=CARTESIAN_POINT('',(8.05,3.67394039744206E-16,-81.35));
#54410=CARTESIAN_POINT('',(8.05,3.67394039744206E-16,-84.8));
#54411=CARTESIAN_POINT('',(8.05,3.67394039744206E-16,-84.8));
#54412=CARTESIAN_POINT('',(8.57259699813413,-0.522596998134133,-84.8));
#54413=CARTESIAN_POINT('',(8.05,3.67394039744206E-16,-84.8));
#54414=CARTESIAN_POINT('',(8.57259699813413,-0.522596998134133,0.));
#54415=CARTESIAN_POINT('Origin',(8.05,3.67394039744206E-16,-84.8));
#54416=CARTESIAN_POINT('',(-8.05,-1.60428730688303E-15,-81.35));
#54417=CARTESIAN_POINT('',(8.05,3.67394039744206E-16,-84.8));
#54418=CARTESIAN_POINT('Origin',(-10.995,-0.510000000000002,-84.8));
#54419=CARTESIAN_POINT('',(-10.6942336092596,-2.79024989380572,-81.35));
#54420=CARTESIAN_POINT('',(-8.71475010619428,-0.810766390740372,-81.35));
#54421=CARTESIAN_POINT('Origin',(-10.995,-0.510000000000002,-81.35));
#54422=CARTESIAN_POINT('',(-10.6942336092596,-2.79024989380572,-84.8));
#54423=CARTESIAN_POINT('',(-10.6942336092596,-2.79024989380572,-84.8));
#54424=CARTESIAN_POINT('',(-8.71475010619428,-0.810766390740372,-84.8));
#54425=CARTESIAN_POINT('Origin',(-10.995,-0.510000000000002,-84.8));
#54426=CARTESIAN_POINT('',(-8.71475010619428,-0.810766390740372,-84.8));
#54427=CARTESIAN_POINT('Origin',(-10.995,-7.69,-84.8));
#54428=CARTESIAN_POINT('',(-8.71475010619428,-7.38923360925963,-81.35));
#54429=CARTESIAN_POINT('',(-10.6942336092596,-5.40975010619428,-81.35));
#54430=CARTESIAN_POINT('Origin',(-10.995,-7.69,-81.35));
#54431=CARTESIAN_POINT('',(-8.71475010619428,-7.38923360925963,-84.8));
#54432=CARTESIAN_POINT('',(-8.71475010619428,-7.38923360925963,-84.8));
#54433=CARTESIAN_POINT('',(-10.6942336092596,-5.40975010619428,-84.8));
#54434=CARTESIAN_POINT('Origin',(-10.995,-7.69,-84.8));
#54435=CARTESIAN_POINT('',(-10.6942336092596,-5.40975010619428,-84.8));
#54436=CARTESIAN_POINT('Origin',(10.995,-0.509999999999999,-84.8));
#54437=CARTESIAN_POINT('',(8.71475010619428,-0.81076639074037,-81.35));
#54438=CARTESIAN_POINT('',(10.6942336092596,-2.79024989380572,-81.35));
#54439=CARTESIAN_POINT('Origin',(10.995,-0.509999999999999,-81.35));
#54440=CARTESIAN_POINT('',(8.71475010619428,-0.81076639074037,-84.8));
#54441=CARTESIAN_POINT('',(8.71475010619428,-0.81076639074037,-84.8));
#54442=CARTESIAN_POINT('',(10.6942336092596,-2.79024989380572,-84.8));
#54443=CARTESIAN_POINT('Origin',(10.995,-0.509999999999999,-84.8));
#54444=CARTESIAN_POINT('',(10.6942336092596,-2.79024989380572,-84.8));
#54445=CARTESIAN_POINT('Origin',(10.995,-7.69,-84.8));
#54446=CARTESIAN_POINT('',(10.6942336092596,-5.40975010619428,-81.35));
#54447=CARTESIAN_POINT('',(8.71475010619428,-7.38923360925963,-81.35));
#54448=CARTESIAN_POINT('Origin',(10.995,-7.69,-81.35));
#54449=CARTESIAN_POINT('',(10.6942336092596,-5.40975010619428,-84.8));
#54450=CARTESIAN_POINT('',(10.6942336092596,-5.40975010619428,-84.8));
#54451=CARTESIAN_POINT('',(8.71475010619428,-7.38923360925963,-84.8));
#54452=CARTESIAN_POINT('Origin',(10.995,-7.69,-84.8));
#54453=CARTESIAN_POINT('',(8.71475010619428,-7.38923360925963,-84.8));
#54454=CARTESIAN_POINT('Origin',(8.55,-12.0328932188134,-84.8));
#54455=CARTESIAN_POINT('Origin',(8.55,-12.0328932188134,-81.35));
#54456=CARTESIAN_POINT('Origin',(8.55,-12.0328932188134,-84.8));
#54457=CARTESIAN_POINT('Origin',(-8.55,-12.0328932188134,-84.8));
#54458=CARTESIAN_POINT('Origin',(-8.55,-12.0328932188134,-81.35));
#54459=CARTESIAN_POINT('Origin',(-8.55,-12.0328932188134,-84.8));
#54460=CARTESIAN_POINT('Origin',(11.,-4.54289321881346,-84.8));
#54461=CARTESIAN_POINT('Origin',(11.,-4.54289321881346,-81.35));
#54462=CARTESIAN_POINT('Origin',(11.,-4.54289321881346,-84.8));
#54463=CARTESIAN_POINT('Origin',(11.,-3.65710678118656,-84.8));
#54464=CARTESIAN_POINT('Origin',(11.,-3.65710678118656,-81.35));
#54465=CARTESIAN_POINT('Origin',(11.,-3.65710678118656,-84.8));
#54466=CARTESIAN_POINT('Origin',(10.6288496112726,-3.28595639245914,-84.8));
#54467=CARTESIAN_POINT('Origin',(10.6288496112726,-3.28595639245914,-81.35));
#54468=CARTESIAN_POINT('Origin',(10.6288496112726,-3.28595639245914,-84.8));
#54469=CARTESIAN_POINT('Origin',(8.21904360754086,-0.876150388727407,-84.8));
#54470=CARTESIAN_POINT('Origin',(8.21904360754086,-0.876150388727407,-81.35));
#54471=CARTESIAN_POINT('Origin',(8.21904360754086,-0.876150388727407,-84.8));
#54472=CARTESIAN_POINT('Origin',(10.6288496112726,-4.91404360754086,-84.8));
#54473=CARTESIAN_POINT('Origin',(10.6288496112726,-4.91404360754086,-81.35));
#54474=CARTESIAN_POINT('Origin',(10.6288496112726,-4.91404360754086,-84.8));
#54475=CARTESIAN_POINT('Origin',(8.21904360754086,-7.32384961127259,-84.8));
#54476=CARTESIAN_POINT('Origin',(8.21904360754086,-7.32384961127259,-81.35));
#54477=CARTESIAN_POINT('Origin',(8.21904360754086,-7.32384961127259,-84.8));
#54478=CARTESIAN_POINT('Origin',(8.55,-8.40710678118654,-84.8));
#54479=CARTESIAN_POINT('Origin',(8.55,-8.40710678118654,-81.35));
#54480=CARTESIAN_POINT('Origin',(8.55,-8.40710678118654,-84.8));
#54481=CARTESIAN_POINT('Origin',(-8.55,-8.40710678118654,-84.8));
#54482=CARTESIAN_POINT('Origin',(-8.55,-8.40710678118654,-81.35));
#54483=CARTESIAN_POINT('Origin',(-8.55,-8.40710678118654,-84.8));
#54484=CARTESIAN_POINT('Origin',(-8.21904360754086,-7.32384961127259,-84.8));
#54485=CARTESIAN_POINT('Origin',(-8.21904360754086,-7.32384961127259,-81.35));
#54486=CARTESIAN_POINT('Origin',(-8.21904360754086,-7.32384961127259,-84.8));
#54487=CARTESIAN_POINT('Origin',(-10.6288496112726,-4.91404360754086,-84.8));
#54488=CARTESIAN_POINT('Origin',(-10.6288496112726,-4.91404360754086,-81.35));
#54489=CARTESIAN_POINT('Origin',(-10.6288496112726,-4.91404360754086,-84.8));
#54490=CARTESIAN_POINT('Origin',(-11.,-4.54289321881346,-84.8));
#54491=CARTESIAN_POINT('Origin',(-11.,-4.54289321881346,-81.35));
#54492=CARTESIAN_POINT('Origin',(-11.,-4.54289321881346,-84.8));
#54493=CARTESIAN_POINT('Origin',(-11.,-3.65710678118656,-84.8));
#54494=CARTESIAN_POINT('Origin',(-11.,-3.65710678118656,-81.35));
#54495=CARTESIAN_POINT('Origin',(-11.,-3.65710678118656,-84.8));
#54496=CARTESIAN_POINT('Origin',(-10.6288496112726,-3.28595639245914,-84.8));
#54497=CARTESIAN_POINT('Origin',(-10.6288496112726,-3.28595639245914,-81.35));
#54498=CARTESIAN_POINT('Origin',(-10.6288496112726,-3.28595639245914,-84.8));
#54499=CARTESIAN_POINT('Origin',(-8.21904360754086,-0.87615038872741,-84.8));
#54500=CARTESIAN_POINT('Origin',(-8.21904360754086,-0.87615038872741,-81.35));
#54501=CARTESIAN_POINT('Origin',(-8.21904360754086,-0.87615038872741,-84.8));
#54502=CARTESIAN_POINT('Origin',(0.,8.,-83.8));
#54503=CARTESIAN_POINT('Origin',(-22.2,13.,-84.8));
#54504=CARTESIAN_POINT('',(-22.2,13.,-84.8));
#54505=CARTESIAN_POINT('',(-22.2,13.,-81.35));
#54506=CARTESIAN_POINT('',(-22.2,13.,-84.8));
#54507=CARTESIAN_POINT('',(22.2,13.,-81.35));
#54508=CARTESIAN_POINT('',(22.2,13.,-81.35));
#54509=CARTESIAN_POINT('',(22.2,13.,-84.8));
#54510=CARTESIAN_POINT('',(22.2,13.,-84.8));
#54511=CARTESIAN_POINT('',(-22.2,13.,-84.8));
#54512=CARTESIAN_POINT('Origin',(0.,0.,-84.8));
#54513=CARTESIAN_POINT('',(-23.2,-15.5,-84.8));
#54514=CARTESIAN_POINT('',(-22.2,-16.5,-84.8));
#54515=CARTESIAN_POINT('',(-23.2,12.,-84.8));
#54516=CARTESIAN_POINT('',(-23.2,-15.5,-84.8));
#54517=CARTESIAN_POINT('',(-23.2,12.,-84.8));
#54518=CARTESIAN_POINT('',(23.2,12.,-84.8));
#54519=CARTESIAN_POINT('',(22.2,13.,-84.8));
#54520=CARTESIAN_POINT('',(23.2,-15.5,-84.8));
#54521=CARTESIAN_POINT('',(23.2,12.,-84.8));
#54522=CARTESIAN_POINT('',(23.2,-15.5,-84.8));
#54523=CARTESIAN_POINT('Origin',(-23.2,12.,-84.8));
#54524=CARTESIAN_POINT('',(-23.2,12.,-81.35));
#54525=CARTESIAN_POINT('',(-23.2,12.,-84.8));
#54526=CARTESIAN_POINT('',(-22.2,13.,-81.35));
#54527=CARTESIAN_POINT('Origin',(-23.2,-15.5,-84.8));
#54528=CARTESIAN_POINT('',(-23.2,-15.5,-81.35));
#54529=CARTESIAN_POINT('',(-23.2,-15.5,-84.8));
#54530=CARTESIAN_POINT('',(-23.2,12.,-81.35));
#54531=CARTESIAN_POINT('Origin',(-22.2,-16.5,-84.8));
#54532=CARTESIAN_POINT('',(-23.2,-15.5,-81.35));
#54533=CARTESIAN_POINT('Origin',(23.2,-15.5,-84.8));
#54534=CARTESIAN_POINT('',(23.2,-15.5,-81.35));
#54535=CARTESIAN_POINT('',(23.2,-15.5,-84.8));
#54536=CARTESIAN_POINT('',(22.2,-16.5,-81.35));
#54537=CARTESIAN_POINT('Origin',(23.2,12.,-84.8));
#54538=CARTESIAN_POINT('',(23.2,12.,-81.35));
#54539=CARTESIAN_POINT('',(23.2,12.,-84.8));
#54540=CARTESIAN_POINT('',(23.2,-15.5,-81.35));
#54541=CARTESIAN_POINT('Origin',(22.2,13.,-84.8));
#54542=CARTESIAN_POINT('',(23.2,12.,-81.35));
#54543=CARTESIAN_POINT('Origin',(-2.3094010767585,8.,-84.4));
#54544=CARTESIAN_POINT('',(-2.3094010767585,8.,-84.4));
#54545=CARTESIAN_POINT('',(-2.3094010767585,8.,-84.4));
#54546=CARTESIAN_POINT('',(-1.15470053837925,10.,-84.4));
#54547=CARTESIAN_POINT('',(-1.15470053837925,10.,-84.4));
#54548=CARTESIAN_POINT('',(-2.3094010767585,8.,-84.4));
#54549=CARTESIAN_POINT('Origin',(-1.15470053837925,6.,-84.4));
#54550=CARTESIAN_POINT('',(-1.15470053837925,6.,-84.4));
#54551=CARTESIAN_POINT('',(-1.15470053837925,6.,-84.4));
#54552=CARTESIAN_POINT('',(-1.15470053837925,6.,-84.4));
#54553=CARTESIAN_POINT('Origin',(1.15470053837925,6.,-84.4));
#54554=CARTESIAN_POINT('',(1.15470053837925,6.,-84.4));
#54555=CARTESIAN_POINT('',(1.15470053837925,6.,-84.4));
#54556=CARTESIAN_POINT('',(1.15470053837925,6.,-84.4));
#54557=CARTESIAN_POINT('Origin',(2.3094010767585,8.,-84.4));
#54558=CARTESIAN_POINT('',(2.3094010767585,8.,-84.4));
#54559=CARTESIAN_POINT('',(2.3094010767585,8.,-84.4));
#54560=CARTESIAN_POINT('',(2.3094010767585,8.,-84.4));
#54561=CARTESIAN_POINT('Origin',(1.15470053837925,10.,-84.4));
#54562=CARTESIAN_POINT('',(1.15470053837925,10.,-84.4));
#54563=CARTESIAN_POINT('',(1.15470053837925,10.,-84.4));
#54564=CARTESIAN_POINT('',(1.15470053837925,10.,-84.4));
#54565=CARTESIAN_POINT('Origin',(-1.15470053837925,10.,-84.4));
#54566=CARTESIAN_POINT('',(-1.15470053837925,10.,-84.4));
#54567=CARTESIAN_POINT('Origin',(0.,0.,-84.4));
#54568=CARTESIAN_POINT('Origin',(-8.55,-12.0328932188134,-81.35));
#54569=CARTESIAN_POINT('',(8.23180194846605,-12.3510912703474,-81.35));
#54570=CARTESIAN_POINT('',(12.3307106781187,-16.45,-81.35));
#54571=CARTESIAN_POINT('',(8.23180194846605,-12.3510912703474,-81.35));
#54572=CARTESIAN_POINT('',(8.1,-12.0328932188134,-81.35));
#54573=CARTESIAN_POINT('Origin',(8.55,-12.0328932188134,-81.35));
#54574=CARTESIAN_POINT('',(8.1,-8.40710678118654,-81.35));
#54575=CARTESIAN_POINT('',(8.1,-8.40710678118654,-81.35));
#54576=CARTESIAN_POINT('',(8.23180194846606,-8.08890872965259,-81.35));
#54577=CARTESIAN_POINT('Origin',(8.55,-8.40710678118654,-81.35));
#54578=CARTESIAN_POINT('',(8.60795233719346,-7.71275834092519,-81.35));
#54579=CARTESIAN_POINT('',(8.60795233719346,-7.71275834092519,-81.35));
#54580=CARTESIAN_POINT('',(8.76432075605962,-7.39577200905833,-81.35));
#54581=CARTESIAN_POINT('Origin',(8.21904360754086,-7.32384961127259,-81.35));
#54582=CARTESIAN_POINT('',(10.7007720090583,-5.45932075605962,-81.35));
#54583=CARTESIAN_POINT('Origin',(10.995,-7.69,-81.35));
#54584=CARTESIAN_POINT('',(11.0177583409252,-5.30295233719346,-81.35));
#54585=CARTESIAN_POINT('Origin',(10.6288496112726,-4.91404360754086,-81.35));
#54586=CARTESIAN_POINT('',(11.3889087296526,-4.93180194846606,-81.35));
#54587=CARTESIAN_POINT('',(11.3889087296526,-4.93180194846606,-81.35));
#54588=CARTESIAN_POINT('',(11.55,-4.54289321881346,-81.35));
#54589=CARTESIAN_POINT('Origin',(11.,-4.54289321881346,-81.35));
#54590=CARTESIAN_POINT('',(11.55,-3.65710678118656,-81.35));
#54591=CARTESIAN_POINT('',(11.55,-3.65710678118656,-81.35));
#54592=CARTESIAN_POINT('',(11.3889087296526,-3.26819805153396,-81.35));
#54593=CARTESIAN_POINT('Origin',(11.,-3.65710678118656,-81.35));
#54594=CARTESIAN_POINT('',(11.0177583409252,-2.89704766280654,-81.35));
#54595=CARTESIAN_POINT('',(11.0177583409252,-2.89704766280654,-81.35));
#54596=CARTESIAN_POINT('',(10.7007720090583,-2.74067924394038,-81.35));
#54597=CARTESIAN_POINT('Origin',(10.6288496112726,-3.28595639245914,-81.35));
#54598=CARTESIAN_POINT('',(8.76432075605962,-0.804227990941667,-81.35));
#54599=CARTESIAN_POINT('Origin',(10.995,-0.509999999999999,-81.35));
#54600=CARTESIAN_POINT('',(8.60795233719346,-0.487241659074806,-81.35));
#54601=CARTESIAN_POINT('Origin',(8.21904360754086,-0.876150388727407,-81.35));
#54602=CARTESIAN_POINT('',(8.07071067811865,0.0500000000000006,-81.35));
#54603=CARTESIAN_POINT('',(8.07071067811865,0.0500000000000006,-81.35));
#54604=CARTESIAN_POINT('',(-8.07071067811865,0.0499999999999998,-81.35));
#54605=CARTESIAN_POINT('',(-8.07071067811865,0.0499999999999998,-81.35));
#54606=CARTESIAN_POINT('',(-8.60795233719346,-0.48724165907481,-81.35));
#54607=CARTESIAN_POINT('',(-8.60795233719346,-0.487241659074809,-81.35));
#54608=CARTESIAN_POINT('',(-8.76432075605962,-0.804227990941668,-81.35));
#54609=CARTESIAN_POINT('Origin',(-8.21904360754086,-0.87615038872741,-81.35));
#54610=CARTESIAN_POINT('',(-10.7007720090583,-2.74067924394038,-81.35));
#54611=CARTESIAN_POINT('Origin',(-10.995,-0.510000000000002,-81.35));
#54612=CARTESIAN_POINT('',(-11.0177583409252,-2.89704766280654,-81.35));
#54613=CARTESIAN_POINT('Origin',(-10.6288496112726,-3.28595639245914,-81.35));
#54614=CARTESIAN_POINT('',(-11.3889087296526,-3.26819805153396,-81.35));
#54615=CARTESIAN_POINT('',(-11.3889087296526,-3.26819805153396,-81.35));
#54616=CARTESIAN_POINT('',(-11.55,-3.65710678118656,-81.35));
#54617=CARTESIAN_POINT('Origin',(-11.,-3.65710678118656,-81.35));
#54618=CARTESIAN_POINT('',(-11.55,-4.54289321881346,-81.35));
#54619=CARTESIAN_POINT('',(-11.55,-4.54289321881346,-81.35));
#54620=CARTESIAN_POINT('',(-11.3889087296526,-4.93180194846607,-81.35));
#54621=CARTESIAN_POINT('Origin',(-11.,-4.54289321881346,-81.35));
#54622=CARTESIAN_POINT('',(-11.0177583409252,-5.30295233719346,-81.35));
#54623=CARTESIAN_POINT('',(-11.0177583409252,-5.30295233719346,-81.35));
#54624=CARTESIAN_POINT('',(-10.7007720090583,-5.45932075605962,-81.35));
#54625=CARTESIAN_POINT('Origin',(-10.6288496112726,-4.91404360754086,-81.35));
#54626=CARTESIAN_POINT('',(-8.76432075605962,-7.39577200905833,-81.35));
#54627=CARTESIAN_POINT('Origin',(-10.995,-7.69,-81.35));
#54628=CARTESIAN_POINT('',(-8.60795233719346,-7.7127583409252,-81.35));
#54629=CARTESIAN_POINT('Origin',(-8.21904360754086,-7.32384961127259,-81.35));
#54630=CARTESIAN_POINT('',(-8.23180194846605,-8.0889087296526,-81.35));
#54631=CARTESIAN_POINT('',(-8.23180194846605,-8.0889087296526,-81.35));
#54632=CARTESIAN_POINT('',(-8.1,-8.40710678118654,-81.35));
#54633=CARTESIAN_POINT('Origin',(-8.55,-8.40710678118654,-81.35));
#54634=CARTESIAN_POINT('',(-8.1,-12.0328932188134,-81.35));
#54635=CARTESIAN_POINT('',(-8.1,-12.0328932188134,-81.35));
#54636=CARTESIAN_POINT('',(-8.23180194846605,-12.3510912703474,-81.35));
#54637=CARTESIAN_POINT('Origin',(-8.55,-12.0328932188134,-81.35));
#54638=CARTESIAN_POINT('',(-12.3307106781186,-16.45,-81.35));
#54639=CARTESIAN_POINT('',(-12.3307106781186,-16.45,-81.35));
#54640=CARTESIAN_POINT('',(-22.1792893218814,-16.45,-81.35));
#54641=CARTESIAN_POINT('',(-22.1792893218814,-16.45,-81.35));
#54642=CARTESIAN_POINT('',(-23.15,-15.4792893218813,-81.35));
#54643=CARTESIAN_POINT('',(-23.15,-15.4792893218813,-81.35));
#54644=CARTESIAN_POINT('',(-23.15,11.9792893218814,-81.35));
#54645=CARTESIAN_POINT('',(-23.15,11.9792893218814,-81.35));
#54646=CARTESIAN_POINT('',(-22.1792893218813,12.95,-81.35));
#54647=CARTESIAN_POINT('',(-22.1792893218813,12.95,-81.35));
#54648=CARTESIAN_POINT('',(22.1792893218813,12.95,-81.35));
#54649=CARTESIAN_POINT('',(22.1792893218813,12.95,-81.35));
#54650=CARTESIAN_POINT('',(23.15,11.9792893218814,-81.35));
#54651=CARTESIAN_POINT('',(23.15,11.9792893218814,-81.35));
#54652=CARTESIAN_POINT('',(23.15,-15.4792893218813,-81.35));
#54653=CARTESIAN_POINT('',(23.15,-15.4792893218813,-81.35));
#54654=CARTESIAN_POINT('',(22.1792893218814,-16.45,-81.35));
#54655=CARTESIAN_POINT('',(22.1792893218814,-16.45,-81.35));
#54656=CARTESIAN_POINT('',(12.3307106781187,-16.45,-81.35));
#54657=CARTESIAN_POINT('Origin',(8.23180194846605,-12.3510912703474,-81.35));
#54658=CARTESIAN_POINT('',(8.23180194846605,-12.3510912703474,-81.3));
#54659=CARTESIAN_POINT('',(12.3307106781187,-16.45,-81.3));
#54660=CARTESIAN_POINT('',(8.23180194846605,-12.3510912703474,-81.3));
#54661=CARTESIAN_POINT('',(8.23180194846605,-12.3510912703474,-81.35));
#54662=CARTESIAN_POINT('',(12.3307106781187,-16.45,-81.35));
#54663=CARTESIAN_POINT('Origin',(8.55,-12.0328932188134,-81.35));
#54664=CARTESIAN_POINT('',(8.1,-12.0328932188134,-81.3));
#54665=CARTESIAN_POINT('Origin',(8.55,-12.0328932188134,-81.3));
#54666=CARTESIAN_POINT('',(8.1,-12.0328932188134,-81.35));
#54667=CARTESIAN_POINT('Origin',(8.1,-8.40710678118654,-81.35));
#54668=CARTESIAN_POINT('',(8.1,-8.40710678118654,-81.3));
#54669=CARTESIAN_POINT('',(8.1,-8.40710678118654,-81.3));
#54670=CARTESIAN_POINT('',(8.1,-8.40710678118654,-81.35));
#54671=CARTESIAN_POINT('Origin',(8.55,-8.40710678118654,-81.35));
#54672=CARTESIAN_POINT('',(8.23180194846606,-8.08890872965259,-81.3));
#54673=CARTESIAN_POINT('Origin',(8.55,-8.40710678118654,-81.3));
#54674=CARTESIAN_POINT('',(8.23180194846606,-8.08890872965259,-81.35));
#54675=CARTESIAN_POINT('Origin',(8.60795233719346,-7.71275834092519,-81.35));
#54676=CARTESIAN_POINT('',(8.60795233719346,-7.71275834092519,-81.3));
#54677=CARTESIAN_POINT('',(8.60795233719346,-7.71275834092519,-81.3));
#54678=CARTESIAN_POINT('',(8.60795233719346,-7.71275834092519,-81.35));
#54679=CARTESIAN_POINT('Origin',(8.21904360754086,-7.32384961127259,-81.35));
#54680=CARTESIAN_POINT('',(8.76432075605962,-7.39577200905833,-81.3));
#54681=CARTESIAN_POINT('Origin',(8.21904360754086,-7.32384961127259,-81.3));
#54682=CARTESIAN_POINT('',(8.76432075605962,-7.39577200905833,-81.35));
#54683=CARTESIAN_POINT('Origin',(10.995,-7.69,-81.35));
#54684=CARTESIAN_POINT('',(10.7007720090583,-5.45932075605962,-81.3));
#54685=CARTESIAN_POINT('Origin',(10.995,-7.69,-81.3));
#54686=CARTESIAN_POINT('',(10.7007720090583,-5.45932075605962,-81.35));
#54687=CARTESIAN_POINT('Origin',(10.6288496112726,-4.91404360754086,-81.35));
#54688=CARTESIAN_POINT('',(11.0177583409252,-5.30295233719346,-81.3));
#54689=CARTESIAN_POINT('Origin',(10.6288496112726,-4.91404360754086,-81.3));
#54690=CARTESIAN_POINT('',(11.0177583409252,-5.30295233719346,-81.35));
#54691=CARTESIAN_POINT('Origin',(11.3889087296526,-4.93180194846606,-81.35));
#54692=CARTESIAN_POINT('',(11.3889087296526,-4.93180194846606,-81.3));
#54693=CARTESIAN_POINT('',(11.3889087296526,-4.93180194846606,-81.3));
#54694=CARTESIAN_POINT('',(11.3889087296526,-4.93180194846606,-81.35));
#54695=CARTESIAN_POINT('Origin',(11.,-4.54289321881346,-81.35));
#54696=CARTESIAN_POINT('',(11.55,-4.54289321881346,-81.3));
#54697=CARTESIAN_POINT('Origin',(11.,-4.54289321881346,-81.3));
#54698=CARTESIAN_POINT('',(11.55,-4.54289321881346,-81.35));
#54699=CARTESIAN_POINT('Origin',(11.55,-3.65710678118656,-81.35));
#54700=CARTESIAN_POINT('',(11.55,-3.65710678118656,-81.3));
#54701=CARTESIAN_POINT('',(11.55,-3.65710678118656,-81.3));
#54702=CARTESIAN_POINT('',(11.55,-3.65710678118656,-81.35));
#54703=CARTESIAN_POINT('Origin',(11.,-3.65710678118656,-81.35));
#54704=CARTESIAN_POINT('',(11.3889087296526,-3.26819805153396,-81.3));
#54705=CARTESIAN_POINT('Origin',(11.,-3.65710678118656,-81.3));
#54706=CARTESIAN_POINT('',(11.3889087296526,-3.26819805153396,-81.35));
#54707=CARTESIAN_POINT('Origin',(11.0177583409252,-2.89704766280654,-81.35));
#54708=CARTESIAN_POINT('',(11.0177583409252,-2.89704766280654,-81.3));
#54709=CARTESIAN_POINT('',(11.0177583409252,-2.89704766280654,-81.3));
#54710=CARTESIAN_POINT('',(11.0177583409252,-2.89704766280654,-81.35));
#54711=CARTESIAN_POINT('Origin',(10.6288496112726,-3.28595639245914,-81.35));
#54712=CARTESIAN_POINT('',(10.7007720090583,-2.74067924394038,-81.3));
#54713=CARTESIAN_POINT('Origin',(10.6288496112726,-3.28595639245914,-81.3));
#54714=CARTESIAN_POINT('',(10.7007720090583,-2.74067924394038,-81.35));
#54715=CARTESIAN_POINT('Origin',(10.995,-0.509999999999999,-81.35));
#54716=CARTESIAN_POINT('',(8.76432075605962,-0.804227990941667,-81.3));
#54717=CARTESIAN_POINT('Origin',(10.995,-0.509999999999999,-81.3));
#54718=CARTESIAN_POINT('',(8.76432075605962,-0.804227990941667,-81.35));
#54719=CARTESIAN_POINT('Origin',(8.21904360754086,-0.876150388727407,-81.35));
#54720=CARTESIAN_POINT('',(8.60795233719346,-0.487241659074806,-81.3));
#54721=CARTESIAN_POINT('Origin',(8.21904360754086,-0.876150388727407,-81.3));
#54722=CARTESIAN_POINT('',(8.60795233719346,-0.487241659074806,-81.35));
#54723=CARTESIAN_POINT('Origin',(8.07071067811865,0.0500000000000006,-81.35));
#54724=CARTESIAN_POINT('',(8.07071067811865,0.0500000000000006,-81.3));
#54725=CARTESIAN_POINT('',(8.07071067811865,0.0500000000000006,-81.3));
#54726=CARTESIAN_POINT('',(8.07071067811865,0.0500000000000006,-81.35));
#54727=CARTESIAN_POINT('Origin',(-8.07071067811865,0.0499999999999998,-81.35));
#54728=CARTESIAN_POINT('',(-8.07071067811865,0.0499999999999998,-81.3));
#54729=CARTESIAN_POINT('',(-8.07071067811865,0.0499999999999998,-81.3));
#54730=CARTESIAN_POINT('',(-8.07071067811865,0.0499999999999998,-81.35));
#54731=CARTESIAN_POINT('Origin',(-8.60795233719346,-0.487241659074809,-81.35));
#54732=CARTESIAN_POINT('',(-8.60795233719346,-0.48724165907481,-81.3));
#54733=CARTESIAN_POINT('',(-8.60795233719346,-0.487241659074809,-81.3));
#54734=CARTESIAN_POINT('',(-8.60795233719346,-0.48724165907481,-81.35));
#54735=CARTESIAN_POINT('Origin',(-8.21904360754086,-0.87615038872741,-81.35));
#54736=CARTESIAN_POINT('',(-8.76432075605962,-0.804227990941668,-81.3));
#54737=CARTESIAN_POINT('Origin',(-8.21904360754086,-0.87615038872741,-81.3));
#54738=CARTESIAN_POINT('',(-8.76432075605962,-0.804227990941668,-81.35));
#54739=CARTESIAN_POINT('Origin',(-10.995,-0.510000000000002,-81.35));
#54740=CARTESIAN_POINT('',(-10.7007720090583,-2.74067924394038,-81.3));
#54741=CARTESIAN_POINT('Origin',(-10.995,-0.510000000000002,-81.3));
#54742=CARTESIAN_POINT('',(-10.7007720090583,-2.74067924394038,-81.35));
#54743=CARTESIAN_POINT('Origin',(-10.6288496112726,-3.28595639245914,-81.35));
#54744=CARTESIAN_POINT('',(-11.0177583409252,-2.89704766280654,-81.3));
#54745=CARTESIAN_POINT('Origin',(-10.6288496112726,-3.28595639245914,-81.3));
#54746=CARTESIAN_POINT('',(-11.0177583409252,-2.89704766280654,-81.35));
#54747=CARTESIAN_POINT('Origin',(-11.3889087296526,-3.26819805153396,-81.35));
#54748=CARTESIAN_POINT('',(-11.3889087296526,-3.26819805153396,-81.3));
#54749=CARTESIAN_POINT('',(-11.3889087296526,-3.26819805153396,-81.3));
#54750=CARTESIAN_POINT('',(-11.3889087296526,-3.26819805153396,-81.35));
#54751=CARTESIAN_POINT('Origin',(-11.,-3.65710678118656,-81.35));
#54752=CARTESIAN_POINT('',(-11.55,-3.65710678118656,-81.3));
#54753=CARTESIAN_POINT('Origin',(-11.,-3.65710678118656,-81.3));
#54754=CARTESIAN_POINT('',(-11.55,-3.65710678118656,-81.35));
#54755=CARTESIAN_POINT('Origin',(-11.55,-4.54289321881346,-81.35));
#54756=CARTESIAN_POINT('',(-11.55,-4.54289321881346,-81.3));
#54757=CARTESIAN_POINT('',(-11.55,-4.54289321881346,-81.3));
#54758=CARTESIAN_POINT('',(-11.55,-4.54289321881346,-81.35));
#54759=CARTESIAN_POINT('Origin',(-11.,-4.54289321881346,-81.35));
#54760=CARTESIAN_POINT('',(-11.3889087296526,-4.93180194846607,-81.3));
#54761=CARTESIAN_POINT('Origin',(-11.,-4.54289321881346,-81.3));
#54762=CARTESIAN_POINT('',(-11.3889087296526,-4.93180194846607,-81.35));
#54763=CARTESIAN_POINT('Origin',(-11.0177583409252,-5.30295233719346,-81.35));
#54764=CARTESIAN_POINT('',(-11.0177583409252,-5.30295233719346,-81.3));
#54765=CARTESIAN_POINT('',(-11.0177583409252,-5.30295233719346,-81.3));
#54766=CARTESIAN_POINT('',(-11.0177583409252,-5.30295233719346,-81.35));
#54767=CARTESIAN_POINT('Origin',(-10.6288496112726,-4.91404360754086,-81.35));
#54768=CARTESIAN_POINT('',(-10.7007720090583,-5.45932075605962,-81.3));
#54769=CARTESIAN_POINT('Origin',(-10.6288496112726,-4.91404360754086,-81.3));
#54770=CARTESIAN_POINT('',(-10.7007720090583,-5.45932075605962,-81.35));
#54771=CARTESIAN_POINT('Origin',(-10.995,-7.69,-81.35));
#54772=CARTESIAN_POINT('',(-8.76432075605962,-7.39577200905833,-81.3));
#54773=CARTESIAN_POINT('Origin',(-10.995,-7.69,-81.3));
#54774=CARTESIAN_POINT('',(-8.76432075605962,-7.39577200905833,-81.35));
#54775=CARTESIAN_POINT('Origin',(-8.21904360754086,-7.32384961127259,-81.35));
#54776=CARTESIAN_POINT('',(-8.60795233719346,-7.7127583409252,-81.3));
#54777=CARTESIAN_POINT('Origin',(-8.21904360754086,-7.32384961127259,-81.3));
#54778=CARTESIAN_POINT('',(-8.60795233719346,-7.7127583409252,-81.35));
#54779=CARTESIAN_POINT('Origin',(-8.23180194846605,-8.0889087296526,-81.35));
#54780=CARTESIAN_POINT('',(-8.23180194846605,-8.0889087296526,-81.3));
#54781=CARTESIAN_POINT('',(-8.23180194846605,-8.0889087296526,-81.3));
#54782=CARTESIAN_POINT('',(-8.23180194846605,-8.0889087296526,-81.35));
#54783=CARTESIAN_POINT('Origin',(-8.55,-8.40710678118654,-81.35));
#54784=CARTESIAN_POINT('',(-8.1,-8.40710678118654,-81.3));
#54785=CARTESIAN_POINT('Origin',(-8.55,-8.40710678118654,-81.3));
#54786=CARTESIAN_POINT('',(-8.1,-8.40710678118654,-81.35));
#54787=CARTESIAN_POINT('Origin',(-8.1,-12.0328932188134,-81.35));
#54788=CARTESIAN_POINT('',(-8.1,-12.0328932188134,-81.3));
#54789=CARTESIAN_POINT('',(-8.1,-12.0328932188134,-81.3));
#54790=CARTESIAN_POINT('',(-8.1,-12.0328932188134,-81.35));
#54791=CARTESIAN_POINT('Origin',(-8.55,-12.0328932188134,-81.35));
#54792=CARTESIAN_POINT('',(-8.23180194846605,-12.3510912703474,-81.3));
#54793=CARTESIAN_POINT('Origin',(-8.55,-12.0328932188134,-81.3));
#54794=CARTESIAN_POINT('',(-8.23180194846605,-12.3510912703474,-81.35));
#54795=CARTESIAN_POINT('Origin',(-12.3307106781186,-16.45,-81.35));
#54796=CARTESIAN_POINT('',(-12.3307106781186,-16.45,-81.3));
#54797=CARTESIAN_POINT('',(-12.3307106781186,-16.45,-81.3));
#54798=CARTESIAN_POINT('',(-12.3307106781186,-16.45,-81.35));
#54799=CARTESIAN_POINT('Origin',(-22.1792893218814,-16.45,-81.35));
#54800=CARTESIAN_POINT('',(-22.1792893218814,-16.45,-81.3));
#54801=CARTESIAN_POINT('',(-22.1792893218814,-16.45,-81.3));
#54802=CARTESIAN_POINT('',(-22.1792893218814,-16.45,-81.35));
#54803=CARTESIAN_POINT('Origin',(-23.15,-15.4792893218813,-81.35));
#54804=CARTESIAN_POINT('',(-23.15,-15.4792893218813,-81.3));
#54805=CARTESIAN_POINT('',(-23.15,-15.4792893218813,-81.3));
#54806=CARTESIAN_POINT('',(-23.15,-15.4792893218813,-81.35));
#54807=CARTESIAN_POINT('Origin',(-23.15,11.9792893218814,-81.35));
#54808=CARTESIAN_POINT('',(-23.15,11.9792893218814,-81.3));
#54809=CARTESIAN_POINT('',(-23.15,11.9792893218814,-81.3));
#54810=CARTESIAN_POINT('',(-23.15,11.9792893218814,-81.35));
#54811=CARTESIAN_POINT('Origin',(-22.1792893218813,12.95,-81.35));
#54812=CARTESIAN_POINT('',(-22.1792893218813,12.95,-81.3));
#54813=CARTESIAN_POINT('',(-22.1792893218813,12.95,-81.3));
#54814=CARTESIAN_POINT('',(-22.1792893218813,12.95,-81.35));
#54815=CARTESIAN_POINT('Origin',(22.1792893218813,12.95,-81.35));
#54816=CARTESIAN_POINT('',(22.1792893218813,12.95,-81.3));
#54817=CARTESIAN_POINT('',(22.1792893218813,12.95,-81.3));
#54818=CARTESIAN_POINT('',(22.1792893218813,12.95,-81.35));
#54819=CARTESIAN_POINT('Origin',(23.15,11.9792893218814,-81.35));
#54820=CARTESIAN_POINT('',(23.15,11.9792893218814,-81.3));
#54821=CARTESIAN_POINT('',(23.15,11.9792893218814,-81.3));
#54822=CARTESIAN_POINT('',(23.15,11.9792893218814,-81.35));
#54823=CARTESIAN_POINT('Origin',(23.15,-15.4792893218813,-81.35));
#54824=CARTESIAN_POINT('',(23.15,-15.4792893218813,-81.3));
#54825=CARTESIAN_POINT('',(23.15,-15.4792893218813,-81.3));
#54826=CARTESIAN_POINT('',(23.15,-15.4792893218813,-81.35));
#54827=CARTESIAN_POINT('Origin',(22.1792893218814,-16.45,-81.35));
#54828=CARTESIAN_POINT('',(22.1792893218814,-16.45,-81.3));
#54829=CARTESIAN_POINT('',(22.1792893218814,-16.45,-81.3));
#54830=CARTESIAN_POINT('',(22.1792893218814,-16.45,-81.35));
#54831=CARTESIAN_POINT('Origin',(12.3307106781187,-16.45,-81.35));
#54832=CARTESIAN_POINT('',(12.3307106781187,-16.45,-81.3));
#54833=CARTESIAN_POINT('Origin',(-1.62630325872826E-14,12.5,-10.6));
#54834=CARTESIAN_POINT('Origin',(-1.50786351795467E-14,12.7,-8.1));
#54835=CARTESIAN_POINT('',(-0.500000000000016,12.7,-8.1));
#54836=CARTESIAN_POINT('',(-0.500000000000016,12.7,-8.1));
#54837=CARTESIAN_POINT('',(0.499999999999983,12.7,-8.1));
#54838=CARTESIAN_POINT('Origin',(-1.50786351795467E-14,12.7,-8.1));
#54839=CARTESIAN_POINT('',(0.499999999999983,12.7,-8.1));
#54840=CARTESIAN_POINT('Origin',(0.,0.,0.));
#54841=CARTESIAN_POINT('',(4.99995,13.,0.));
#54842=CARTESIAN_POINT('',(22.2,13.,0.));
#54843=CARTESIAN_POINT('',(-22.2,13.,0.));
#54844=CARTESIAN_POINT('',(4.99995,8.,0.));
#54845=CARTESIAN_POINT('',(4.99995,13.,0.));
#54846=CARTESIAN_POINT('',(-4.99995,8.,0.));
#54847=CARTESIAN_POINT('Origin',(0.,8.,0.));
#54848=CARTESIAN_POINT('',(-4.99995,13.,0.));
#54849=CARTESIAN_POINT('',(-4.99995,13.,0.));
#54850=CARTESIAN_POINT('',(-22.2,13.,0.));
#54851=CARTESIAN_POINT('',(-22.2,13.,0.));
#54852=CARTESIAN_POINT('',(-23.2,12.,0.));
#54853=CARTESIAN_POINT('',(-22.2,13.,0.));
#54854=CARTESIAN_POINT('',(-23.2,-15.5,0.));
#54855=CARTESIAN_POINT('',(-23.2,12.,0.));
#54856=CARTESIAN_POINT('',(-22.2,-16.5,0.));
#54857=CARTESIAN_POINT('',(-23.2,-15.5,0.));
#54858=CARTESIAN_POINT('',(-12.31,-16.5,0.));
#54859=CARTESIAN_POINT('',(-23.,-16.5,0.));
#54860=CARTESIAN_POINT('',(-8.19644660940672,-12.3864466094067,0.));
#54861=CARTESIAN_POINT('',(-12.31,-16.5,0.));
#54862=CARTESIAN_POINT('',(-8.05,-12.0328932188134,0.));
#54863=CARTESIAN_POINT('Origin',(-8.55,-12.0328932188134,0.));
#54864=CARTESIAN_POINT('',(-8.05,-8.40710678118654,0.));
#54865=CARTESIAN_POINT('',(-8.05,-12.24,0.));
#54866=CARTESIAN_POINT('',(-8.19644660940673,-8.05355339059327,0.));
#54867=CARTESIAN_POINT('Origin',(-8.55,-8.40710678118654,0.));
#54868=CARTESIAN_POINT('',(-8.57259699813413,-7.67740300186587,0.));
#54869=CARTESIAN_POINT('',(-8.05,-8.2,0.));
#54870=CARTESIAN_POINT('',(-8.71475010619428,-7.38923360925963,0.));
#54871=CARTESIAN_POINT('Origin',(-8.21904360754086,-7.32384961127259,0.));
#54872=CARTESIAN_POINT('',(-10.6942336092596,-5.40975010619428,0.));
#54873=CARTESIAN_POINT('Origin',(-10.995,-7.69,0.));
#54874=CARTESIAN_POINT('',(-10.9824030018659,-5.26759699813413,0.));
#54875=CARTESIAN_POINT('Origin',(-10.6288496112726,-4.91404360754086,0.));
#54876=CARTESIAN_POINT('',(-11.3535533905933,-4.89644660940674,0.));
#54877=CARTESIAN_POINT('',(-8.05,-8.2,0.));
#54878=CARTESIAN_POINT('',(-11.5,-4.54289321881346,0.));
#54879=CARTESIAN_POINT('Origin',(-11.,-4.54289321881346,0.));
#54880=CARTESIAN_POINT('',(-11.5,-3.65710678118656,0.));
#54881=CARTESIAN_POINT('',(-11.5,-4.75000000000001,0.));
#54882=CARTESIAN_POINT('',(-11.3535533905933,-3.30355339059329,0.));
#54883=CARTESIAN_POINT('Origin',(-11.,-3.65710678118656,0.));
#54884=CARTESIAN_POINT('',(-10.9824030018659,-2.93240300186587,0.));
#54885=CARTESIAN_POINT('',(-8.05,-1.60428730688303E-15,0.));
#54886=CARTESIAN_POINT('',(-10.6942336092596,-2.79024989380572,0.));
#54887=CARTESIAN_POINT('Origin',(-10.6288496112726,-3.28595639245914,0.));
#54888=CARTESIAN_POINT('',(-8.71475010619428,-0.810766390740372,0.));
#54889=CARTESIAN_POINT('Origin',(-10.995,-0.510000000000002,0.));
#54890=CARTESIAN_POINT('',(-8.57259699813413,-0.522596998134137,0.));
#54891=CARTESIAN_POINT('Origin',(-8.21904360754086,-0.87615038872741,0.));
#54892=CARTESIAN_POINT('',(-8.05,-1.60428730688303E-15,0.));
#54893=CARTESIAN_POINT('',(-8.05,-1.60428730688303E-15,0.));
#54894=CARTESIAN_POINT('',(8.05,3.67394039744206E-16,0.));
#54895=CARTESIAN_POINT('',(8.05,3.67394039744206E-16,0.));
#54896=CARTESIAN_POINT('',(8.57259699813413,-0.522596998134133,0.));
#54897=CARTESIAN_POINT('',(8.05,3.67394039744206E-16,0.));
#54898=CARTESIAN_POINT('',(8.71475010619428,-0.81076639074037,0.));
#54899=CARTESIAN_POINT('Origin',(8.21904360754086,-0.876150388727407,0.));
#54900=CARTESIAN_POINT('',(10.6942336092596,-2.79024989380572,0.));
#54901=CARTESIAN_POINT('Origin',(10.995,-0.509999999999999,0.));
#54902=CARTESIAN_POINT('',(10.9824030018659,-2.93240300186586,0.));
#54903=CARTESIAN_POINT('Origin',(10.6288496112726,-3.28595639245914,0.));
#54904=CARTESIAN_POINT('',(11.3535533905933,-3.30355339059329,0.));
#54905=CARTESIAN_POINT('',(8.05,3.67394039744206E-16,0.));
#54906=CARTESIAN_POINT('',(11.5,-3.65710678118656,0.));
#54907=CARTESIAN_POINT('Origin',(11.,-3.65710678118656,0.));
#54908=CARTESIAN_POINT('',(11.5,-4.54289321881346,0.));
#54909=CARTESIAN_POINT('',(11.5,-4.75000000000001,0.));
#54910=CARTESIAN_POINT('',(11.3535533905933,-4.89644660940673,0.));
#54911=CARTESIAN_POINT('Origin',(11.,-4.54289321881346,0.));
#54912=CARTESIAN_POINT('',(10.9824030018659,-5.26759699813413,0.));
#54913=CARTESIAN_POINT('',(8.05,-8.2,0.));
#54914=CARTESIAN_POINT('',(10.6942336092596,-5.40975010619428,0.));
#54915=CARTESIAN_POINT('Origin',(10.6288496112726,-4.91404360754086,0.));
#54916=CARTESIAN_POINT('',(8.71475010619428,-7.38923360925963,0.));
#54917=CARTESIAN_POINT('Origin',(10.995,-7.69,0.));
#54918=CARTESIAN_POINT('',(8.57259699813413,-7.67740300186587,0.));
#54919=CARTESIAN_POINT('Origin',(8.21904360754086,-7.32384961127259,0.));
#54920=CARTESIAN_POINT('',(8.19644660940673,-8.05355339059327,0.));
#54921=CARTESIAN_POINT('',(8.05,-8.2,0.));
#54922=CARTESIAN_POINT('',(8.05,-8.40710678118654,0.));
#54923=CARTESIAN_POINT('Origin',(8.55,-8.40710678118654,0.));
#54924=CARTESIAN_POINT('',(8.05,-12.0328932188134,0.));
#54925=CARTESIAN_POINT('',(8.05,-12.24,0.));
#54926=CARTESIAN_POINT('',(8.19644660940673,-12.3864466094067,0.));
#54927=CARTESIAN_POINT('Origin',(8.55,-12.0328932188134,0.));
#54928=CARTESIAN_POINT('',(12.31,-16.5,0.));
#54929=CARTESIAN_POINT('',(12.31,-16.5,0.));
#54930=CARTESIAN_POINT('',(22.2,-16.5,0.));
#54931=CARTESIAN_POINT('',(12.31,-16.5,0.));
#54932=CARTESIAN_POINT('',(23.2,-15.5,0.));
#54933=CARTESIAN_POINT('',(23.2,-15.5,0.));
#54934=CARTESIAN_POINT('',(23.2,12.,0.));
#54935=CARTESIAN_POINT('',(23.2,12.,0.));
#54936=CARTESIAN_POINT('',(22.2,13.,0.));
#54937=CARTESIAN_POINT('Origin',(0.499999999999983,12.7,-8.1));
#54938=CARTESIAN_POINT('',(0.499999999999983,13.,-8.1));
#54939=CARTESIAN_POINT('',(0.499999999999983,13.,-8.1));
#54940=CARTESIAN_POINT('',(0.499999999999983,12.7,-8.1));
#54941=CARTESIAN_POINT('Origin',(-0.500000000000016,12.7,-8.1));
#54942=CARTESIAN_POINT('',(-0.500000000000017,13.,-8.1));
#54943=CARTESIAN_POINT('',(-0.500000000000017,13.,-8.1));
#54944=CARTESIAN_POINT('',(-0.500000000000016,12.7,-8.1));
#54945=CARTESIAN_POINT('Origin',(-1.50786351795467E-14,12.7,-8.1));
#54946=CARTESIAN_POINT('Origin',(-1.54689479616415E-14,13.,-8.1));
#54947=CARTESIAN_POINT('Origin',(-1.87674352915389E-14,12.5,-74.2));
#54948=CARTESIAN_POINT('Origin',(-1.50786351795467E-14,12.7,-76.7));
#54949=CARTESIAN_POINT('',(0.499999999999986,12.7,-76.7));
#54950=CARTESIAN_POINT('',(0.499999999999986,12.7,-76.7));
#54951=CARTESIAN_POINT('',(-0.500000000000025,12.7,-76.7));
#54952=CARTESIAN_POINT('Origin',(-1.50786351795467E-14,12.7,-76.7));
#54953=CARTESIAN_POINT('',(-0.500000000000025,12.7,-76.7));
#54954=CARTESIAN_POINT('Origin',(12.31,-16.5,-84.8));
#54955=CARTESIAN_POINT('',(12.31,-16.5,-3.45));
#54956=CARTESIAN_POINT('',(22.2,-16.5,-3.45));
#54957=CARTESIAN_POINT('',(12.31,-16.5,-3.45));
#54958=CARTESIAN_POINT('',(22.2,-16.5,-13.4));
#54959=CARTESIAN_POINT('',(12.31,-16.5,-84.8));
#54960=CARTESIAN_POINT('Origin',(23.2,-15.5,-13.4));
#54961=CARTESIAN_POINT('',(23.2,-15.5,-3.45));
#54962=CARTESIAN_POINT('',(22.2,-16.5,-3.45));
#54963=CARTESIAN_POINT('',(23.2,-15.5,-13.4));
#54964=CARTESIAN_POINT('Origin',(23.2,12.,-13.4));
#54965=CARTESIAN_POINT('',(23.2,12.,-3.45));
#54966=CARTESIAN_POINT('',(23.2,-15.5,-3.45));
#54967=CARTESIAN_POINT('',(23.2,12.,-13.4));
#54968=CARTESIAN_POINT('Origin',(22.2,13.,-13.4));
#54969=CARTESIAN_POINT('',(22.2,13.,-3.45));
#54970=CARTESIAN_POINT('',(23.2,12.,-3.45));
#54971=CARTESIAN_POINT('',(22.2,13.,-13.4));
#54972=CARTESIAN_POINT('Origin',(-22.2,13.,-13.4));
#54973=CARTESIAN_POINT('',(4.99995,13.,-0.999999999999999));
#54974=CARTESIAN_POINT('',(-4.99995,13.,-1.));
#54975=CARTESIAN_POINT('',(-4.99995,13.,-1.));
#54976=CARTESIAN_POINT('',(4.99995,13.,-1.));
#54977=CARTESIAN_POINT('',(-22.2,13.,-3.45));
#54978=CARTESIAN_POINT('',(22.2,13.,-3.45));
#54979=CARTESIAN_POINT('',(-22.2,13.,-13.4));
#54980=CARTESIAN_POINT('',(-4.99995,13.,-1.));
#54981=CARTESIAN_POINT('Origin',(-22.2,13.,-13.4));
#54982=CARTESIAN_POINT('',(-23.2,12.,-3.45));
#54983=CARTESIAN_POINT('',(-22.2,13.,-3.45));
#54984=CARTESIAN_POINT('',(-23.2,12.,-13.4));
#54985=CARTESIAN_POINT('Origin',(-23.2,12.,-13.4));
#54986=CARTESIAN_POINT('',(-23.2,-15.5,-3.45));
#54987=CARTESIAN_POINT('',(-23.2,12.,-3.45));
#54988=CARTESIAN_POINT('',(-23.2,-15.5,-13.4));
#54989=CARTESIAN_POINT('Origin',(-23.2,-15.5,-13.4));
#54990=CARTESIAN_POINT('',(-22.2,-16.5,-3.45));
#54991=CARTESIAN_POINT('',(-23.2,-15.5,-3.45));
#54992=CARTESIAN_POINT('',(-22.2,-16.5,-13.4));
#54993=CARTESIAN_POINT('Origin',(-23.,-16.5,-84.8));
#54994=CARTESIAN_POINT('',(-12.31,-16.5,-3.45));
#54995=CARTESIAN_POINT('',(-22.2,-16.5,-3.45));
#54996=CARTESIAN_POINT('',(-12.31,-16.5,-84.8));
#54997=CARTESIAN_POINT('Origin',(-12.31,-16.5,-84.8));
#54998=CARTESIAN_POINT('',(-8.19644660940672,-12.3864466094067,-3.45));
#54999=CARTESIAN_POINT('',(-12.31,-16.5,-3.45));
#55000=CARTESIAN_POINT('',(-8.19644660940672,-12.3864466094067,-84.8));
#55001=CARTESIAN_POINT('Origin',(-8.55,-12.0328932188134,-84.8));
#55002=CARTESIAN_POINT('',(-8.05,-12.0328932188134,-3.45));
#55003=CARTESIAN_POINT('Origin',(-8.55,-12.0328932188134,-3.45));
#55004=CARTESIAN_POINT('',(-8.05,-12.0328932188134,-84.8));
#55005=CARTESIAN_POINT('Origin',(-8.05,-12.24,-84.8));
#55006=CARTESIAN_POINT('',(-8.05,-8.40710678118654,-3.45));
#55007=CARTESIAN_POINT('',(-8.05,-12.0328932188134,-3.45));
#55008=CARTESIAN_POINT('',(-8.05,-8.40710678118654,-84.8));
#55009=CARTESIAN_POINT('Origin',(-8.55,-8.40710678118654,-84.8));
#55010=CARTESIAN_POINT('',(-8.19644660940673,-8.05355339059327,-3.45));
#55011=CARTESIAN_POINT('Origin',(-8.55,-8.40710678118654,-3.45));
#55012=CARTESIAN_POINT('',(-8.19644660940673,-8.05355339059327,-84.8));
#55013=CARTESIAN_POINT('Origin',(-8.05,-8.2,-84.8));
#55014=CARTESIAN_POINT('',(-8.57259699813413,-7.67740300186587,-3.45));
#55015=CARTESIAN_POINT('',(-8.19644660940673,-8.05355339059327,-3.45));
#55016=CARTESIAN_POINT('',(-8.57259699813413,-7.67740300186587,0.));
#55017=CARTESIAN_POINT('Origin',(-8.21904360754086,-7.32384961127259,-84.8));
#55018=CARTESIAN_POINT('',(-8.71475010619428,-7.38923360925963,-3.45));
#55019=CARTESIAN_POINT('Origin',(-8.21904360754086,-7.32384961127259,-3.45));
#55020=CARTESIAN_POINT('',(-8.71475010619428,-7.38923360925963,-84.8));
#55021=CARTESIAN_POINT('Origin',(-10.995,-7.69,-84.8));
#55022=CARTESIAN_POINT('',(-10.6942336092596,-5.40975010619428,-3.45));
#55023=CARTESIAN_POINT('Origin',(-10.995,-7.69,-3.45));
#55024=CARTESIAN_POINT('',(-10.6942336092596,-5.40975010619428,-84.8));
#55025=CARTESIAN_POINT('Origin',(-10.6288496112726,-4.91404360754086,-84.8));
#55026=CARTESIAN_POINT('',(-10.9824030018659,-5.26759699813413,-3.45));
#55027=CARTESIAN_POINT('Origin',(-10.6288496112726,-4.91404360754086,-3.45));
#55028=CARTESIAN_POINT('',(-10.9824030018659,-5.26759699813413,-84.8));
#55029=CARTESIAN_POINT('Origin',(-8.05,-8.2,-84.8));
#55030=CARTESIAN_POINT('',(-11.3535533905933,-4.89644660940674,-3.45));
#55031=CARTESIAN_POINT('',(-10.9824030018659,-5.26759699813413,-3.45));
#55032=CARTESIAN_POINT('',(-11.3535533905933,-4.89644660940674,0.));
#55033=CARTESIAN_POINT('Origin',(-11.,-4.54289321881346,-84.8));
#55034=CARTESIAN_POINT('',(-11.5,-4.54289321881346,-3.45));
#55035=CARTESIAN_POINT('Origin',(-11.,-4.54289321881346,-3.45));
#55036=CARTESIAN_POINT('',(-11.5,-4.54289321881346,-84.8));
#55037=CARTESIAN_POINT('Origin',(-11.5,-4.75000000000001,-84.8));
#55038=CARTESIAN_POINT('',(-11.5,-3.65710678118656,-3.45));
#55039=CARTESIAN_POINT('',(-11.5,-4.54289321881346,-3.45));
#55040=CARTESIAN_POINT('',(-11.5,-3.65710678118656,0.));
#55041=CARTESIAN_POINT('Origin',(-11.,-3.65710678118656,-84.8));
#55042=CARTESIAN_POINT('',(-11.3535533905933,-3.30355339059329,-3.45));
#55043=CARTESIAN_POINT('Origin',(-11.,-3.65710678118656,-3.45));
#55044=CARTESIAN_POINT('',(-11.3535533905933,-3.30355339059329,-84.8));
#55045=CARTESIAN_POINT('Origin',(-8.05,-1.60428730688303E-15,-84.8));
#55046=CARTESIAN_POINT('',(-10.9824030018659,-2.93240300186587,-3.45));
#55047=CARTESIAN_POINT('',(-11.3535533905933,-3.30355339059329,-3.45));
#55048=CARTESIAN_POINT('',(-10.9824030018659,-2.93240300186587,0.));
#55049=CARTESIAN_POINT('Origin',(-10.6288496112726,-3.28595639245914,-84.8));
#55050=CARTESIAN_POINT('',(-10.6942336092596,-2.79024989380572,-3.45));
#55051=CARTESIAN_POINT('Origin',(-10.6288496112726,-3.28595639245914,-3.45));
#55052=CARTESIAN_POINT('',(-10.6942336092596,-2.79024989380572,-84.8));
#55053=CARTESIAN_POINT('Origin',(-10.995,-0.510000000000002,-84.8));
#55054=CARTESIAN_POINT('',(-8.71475010619428,-0.810766390740372,-3.45));
#55055=CARTESIAN_POINT('Origin',(-10.995,-0.510000000000002,-3.45));
#55056=CARTESIAN_POINT('',(-8.71475010619428,-0.810766390740372,-84.8));
#55057=CARTESIAN_POINT('Origin',(-8.21904360754086,-0.87615038872741,-84.8));
#55058=CARTESIAN_POINT('',(-8.57259699813413,-0.522596998134137,-3.45));
#55059=CARTESIAN_POINT('Origin',(-8.21904360754086,-0.87615038872741,-3.45));
#55060=CARTESIAN_POINT('',(-8.57259699813413,-0.522596998134137,-84.8));
#55061=CARTESIAN_POINT('Origin',(-8.05,-1.60428730688303E-15,-84.8));
#55062=CARTESIAN_POINT('',(-8.05,-1.60428730688303E-15,-3.45));
#55063=CARTESIAN_POINT('',(-8.57259699813413,-0.522596998134137,-3.45));
#55064=CARTESIAN_POINT('',(-8.05,-1.60428730688303E-15,-84.8));
#55065=CARTESIAN_POINT('Origin',(8.05,3.67394039744206E-16,-84.8));
#55066=CARTESIAN_POINT('',(8.05,3.67394039744206E-16,-3.45));
#55067=CARTESIAN_POINT('',(-8.05,-1.60428730688303E-15,-3.45));
#55068=CARTESIAN_POINT('',(8.05,3.67394039744206E-16,-84.8));
#55069=CARTESIAN_POINT('Origin',(8.05,3.67394039744206E-16,-84.8));
#55070=CARTESIAN_POINT('',(8.57259699813413,-0.522596998134133,-3.45));
#55071=CARTESIAN_POINT('',(8.05,3.67394039744206E-16,-3.45));
#55072=CARTESIAN_POINT('',(8.57259699813413,-0.522596998134133,0.));
#55073=CARTESIAN_POINT('Origin',(8.21904360754086,-0.876150388727407,-84.8));
#55074=CARTESIAN_POINT('',(8.71475010619428,-0.81076639074037,-3.45));
#55075=CARTESIAN_POINT('Origin',(8.21904360754086,-0.876150388727407,-3.45));
#55076=CARTESIAN_POINT('',(8.71475010619428,-0.81076639074037,-84.8));
#55077=CARTESIAN_POINT('Origin',(10.995,-0.509999999999999,-84.8));
#55078=CARTESIAN_POINT('',(10.6942336092596,-2.79024989380572,-3.45));
#55079=CARTESIAN_POINT('Origin',(10.995,-0.509999999999999,-3.45));
#55080=CARTESIAN_POINT('',(10.6942336092596,-2.79024989380572,-84.8));
#55081=CARTESIAN_POINT('Origin',(10.6288496112726,-3.28595639245914,-84.8));
#55082=CARTESIAN_POINT('',(10.9824030018659,-2.93240300186586,-3.45));
#55083=CARTESIAN_POINT('Origin',(10.6288496112726,-3.28595639245914,-3.45));
#55084=CARTESIAN_POINT('',(10.9824030018659,-2.93240300186586,-84.8));
#55085=CARTESIAN_POINT('Origin',(8.05,3.67394039744206E-16,-84.8));
#55086=CARTESIAN_POINT('',(11.3535533905933,-3.30355339059329,-3.45));
#55087=CARTESIAN_POINT('',(10.9824030018659,-2.93240300186586,-3.45));
#55088=CARTESIAN_POINT('',(11.3535533905933,-3.30355339059329,0.));
#55089=CARTESIAN_POINT('Origin',(11.,-3.65710678118656,-84.8));
#55090=CARTESIAN_POINT('',(11.5,-3.65710678118656,-3.45));
#55091=CARTESIAN_POINT('Origin',(11.,-3.65710678118656,-3.45));
#55092=CARTESIAN_POINT('',(11.5,-3.65710678118656,-84.8));
#55093=CARTESIAN_POINT('Origin',(11.5,-4.75000000000001,-84.8));
#55094=CARTESIAN_POINT('',(11.5,-4.54289321881346,-3.45));
#55095=CARTESIAN_POINT('',(11.5,-3.65710678118656,-3.45));
#55096=CARTESIAN_POINT('',(11.5,-4.54289321881346,0.));
#55097=CARTESIAN_POINT('Origin',(11.,-4.54289321881346,-84.8));
#55098=CARTESIAN_POINT('',(11.3535533905933,-4.89644660940673,-3.45));
#55099=CARTESIAN_POINT('Origin',(11.,-4.54289321881346,-3.45));
#55100=CARTESIAN_POINT('',(11.3535533905933,-4.89644660940673,-84.8));
#55101=CARTESIAN_POINT('Origin',(8.05,-8.2,-84.8));
#55102=CARTESIAN_POINT('',(10.9824030018659,-5.26759699813413,-3.45));
#55103=CARTESIAN_POINT('',(11.3535533905933,-4.89644660940673,-3.45));
#55104=CARTESIAN_POINT('',(10.9824030018659,-5.26759699813413,0.));
#55105=CARTESIAN_POINT('Origin',(10.6288496112726,-4.91404360754086,-84.8));
#55106=CARTESIAN_POINT('',(10.6942336092596,-5.40975010619428,-3.45));
#55107=CARTESIAN_POINT('Origin',(10.6288496112726,-4.91404360754086,-3.45));
#55108=CARTESIAN_POINT('',(10.6942336092596,-5.40975010619428,-84.8));
#55109=CARTESIAN_POINT('Origin',(10.995,-7.69,-84.8));
#55110=CARTESIAN_POINT('',(8.71475010619428,-7.38923360925963,-3.45));
#55111=CARTESIAN_POINT('Origin',(10.995,-7.69,-3.45));
#55112=CARTESIAN_POINT('',(8.71475010619428,-7.38923360925963,-84.8));
#55113=CARTESIAN_POINT('Origin',(8.21904360754086,-7.32384961127259,-84.8));
#55114=CARTESIAN_POINT('',(8.57259699813413,-7.67740300186587,-3.45));
#55115=CARTESIAN_POINT('Origin',(8.21904360754086,-7.32384961127259,-3.45));
#55116=CARTESIAN_POINT('',(8.57259699813413,-7.67740300186587,-84.8));
#55117=CARTESIAN_POINT('Origin',(8.05,-8.2,-84.8));
#55118=CARTESIAN_POINT('',(8.19644660940673,-8.05355339059327,-3.45));
#55119=CARTESIAN_POINT('',(8.57259699813413,-7.67740300186587,-3.45));
#55120=CARTESIAN_POINT('',(8.19644660940673,-8.05355339059327,-84.8));
#55121=CARTESIAN_POINT('Origin',(8.55,-8.40710678118654,-84.8));
#55122=CARTESIAN_POINT('',(8.05,-8.40710678118654,-3.45));
#55123=CARTESIAN_POINT('Origin',(8.55,-8.40710678118654,-3.45));
#55124=CARTESIAN_POINT('',(8.05,-8.40710678118654,-84.8));
#55125=CARTESIAN_POINT('Origin',(8.05,-12.24,-84.8));
#55126=CARTESIAN_POINT('',(8.05,-12.0328932188134,-3.45));
#55127=CARTESIAN_POINT('',(8.05,-8.40710678118654,-3.45));
#55128=CARTESIAN_POINT('',(8.05,-12.0328932188134,-84.8));
#55129=CARTESIAN_POINT('Origin',(8.55,-12.0328932188134,-84.8));
#55130=CARTESIAN_POINT('',(8.19644660940673,-12.3864466094067,-3.45));
#55131=CARTESIAN_POINT('Origin',(8.55,-12.0328932188134,-3.45));
#55132=CARTESIAN_POINT('',(8.19644660940673,-12.3864466094067,-84.8));
#55133=CARTESIAN_POINT('Origin',(12.31,-16.5,-84.8));
#55134=CARTESIAN_POINT('',(8.19644660940673,-12.3864466094067,-3.45));
#55135=CARTESIAN_POINT('Origin',(-1.54689479616415E-14,13.,-8.1));
#55136=CARTESIAN_POINT('Origin',(-34.5,4.40457132572236E-15,-104.175753233145));
#55137=CARTESIAN_POINT('',(-30.9292009086072,4.33680868994202E-15,-59.4));
#55138=CARTESIAN_POINT('',(-30.9292009086072,4.33680868994202E-15,-25.4));
#55139=CARTESIAN_POINT('',(-30.9292009086072,4.37613505316247E-15,-13.4));
#55140=CARTESIAN_POINT('',(-34.,4.4005895457577E-15,-25.4));
#55141=CARTESIAN_POINT('',(-34.5,4.40457132572236E-15,-25.4));
#55142=CARTESIAN_POINT('',(-34.,4.4005895457577E-15,-59.4));
#55143=CARTESIAN_POINT('',(-34.,4.4005895457577E-15,-104.175753233145));
#55144=CARTESIAN_POINT('',(-34.5,4.40457132572236E-15,-59.4));
#55145=CARTESIAN_POINT('Origin',(35.,6.66784336078585E-15,-104.175753233145));
#55146=CARTESIAN_POINT('',(34.5,6.46233547508513E-15,-59.4));
#55147=CARTESIAN_POINT('',(34.5,6.46233547508513E-15,-25.4));
#55148=CARTESIAN_POINT('',(34.5,6.46233547508513E-15,-104.175753233145));
#55149=CARTESIAN_POINT('',(30.9292009086072,4.77048955893622E-15,-25.4));
#55150=CARTESIAN_POINT('',(35.,6.66784336078585E-15,-25.4));
#55151=CARTESIAN_POINT('',(30.9292009086072,4.99468073201678E-15,-59.4));
#55152=CARTESIAN_POINT('',(30.9292009086072,4.99468073201678E-15,-71.4));
#55153=CARTESIAN_POINT('',(35.,6.66784336078585E-15,-59.4));
#55154=CARTESIAN_POINT('Origin',(-0.500000000000025,12.7,-76.7));
#55155=CARTESIAN_POINT('',(-0.500000000000025,13.,-76.7));
#55156=CARTESIAN_POINT('',(-0.500000000000025,13.,-76.7));
#55157=CARTESIAN_POINT('',(-0.500000000000025,12.7,-76.7));
#55158=CARTESIAN_POINT('Origin',(0.499999999999986,12.7,-76.7));
#55159=CARTESIAN_POINT('',(0.499999999999986,13.,-76.7));
#55160=CARTESIAN_POINT('',(0.499999999999986,13.,-76.7));
#55161=CARTESIAN_POINT('',(0.499999999999986,12.7,-76.7));
#55162=CARTESIAN_POINT('Origin',(-1.50786351795467E-14,12.7,-76.7));
#55163=CARTESIAN_POINT('Origin',(-1.54689479616415E-14,13.,-76.7));
#55164=CARTESIAN_POINT('Origin',(-30.9292009086072,-2.,-104.175753233145));
#55165=CARTESIAN_POINT('',(-28.9973492560291,-1.48236190979496,-25.4));
#55166=CARTESIAN_POINT('Origin',(-30.9292009086072,-2.,-25.4));
#55167=CARTESIAN_POINT('',(-28.9973492560291,-1.48236190979496,-59.4));
#55168=CARTESIAN_POINT('Origin',(-30.9292009086072,-2.,-59.4));
#55169=CARTESIAN_POINT('',(-28.9973492560291,-1.48236190979496,-71.4));
#55170=CARTESIAN_POINT('Origin',(0.,0.,-25.4));
#55171=CARTESIAN_POINT('',(-25.7,-13.788236863595,-25.4));
#55172=CARTESIAN_POINT('',(-29.3945469326493,4.36391374425416E-15,-25.4));
#55173=CARTESIAN_POINT('',(-25.7,0.500000000000004,-25.4));
#55174=CARTESIAN_POINT('',(-25.7,-16.5,-25.4));
#55175=CARTESIAN_POINT('',(-34.5,0.500000000000005,-25.4));
#55176=CARTESIAN_POINT('',(-25.7,0.500000000000004,-25.4));
#55177=CARTESIAN_POINT('',(-34.5,0.500000000000005,-25.4));
#55178=CARTESIAN_POINT('Origin',(-25.7,-16.5,-25.4));
#55179=CARTESIAN_POINT('',(-25.7,-13.788236863595,-24.6339201514178));
#55180=CARTESIAN_POINT('',(-25.7,-13.788236863595,-104.175753233145));
#55181=CARTESIAN_POINT('',(-25.7,0.500000000000004,-24.6339201514178));
#55182=CARTESIAN_POINT('',(-25.7,24.2065391822594,-24.6339201514178));
#55183=CARTESIAN_POINT('',(-25.7,0.500000000000004,-25.4));
#55184=CARTESIAN_POINT('Origin',(25.7,0.500000000000004,-25.4));
#55185=CARTESIAN_POINT('',(25.7,0.500000000000004,-25.4));
#55186=CARTESIAN_POINT('',(25.7,0.499999999999997,-24.6339201514179));
#55187=CARTESIAN_POINT('',(25.7,0.500000000000004,-25.4));
#55188=CARTESIAN_POINT('',(25.7,-13.788236863595,-24.6339201514178));
#55189=CARTESIAN_POINT('',(25.7,24.2065391822594,-24.6339201514179));
#55190=CARTESIAN_POINT('',(25.7,-13.788236863595,-25.4));
#55191=CARTESIAN_POINT('',(25.7,-13.788236863595,-104.175753233145));
#55192=CARTESIAN_POINT('',(25.7,0.500000000000004,-25.4));
#55193=CARTESIAN_POINT('Origin',(0.,0.,-25.4));
#55194=CARTESIAN_POINT('',(28.9973492560291,-1.48236190979496,-25.4));
#55195=CARTESIAN_POINT('',(29.3945469326493,4.36391374425416E-15,-25.4));
#55196=CARTESIAN_POINT('Origin',(30.9292009086072,-2.,-25.4));
#55197=CARTESIAN_POINT('',(35.,0.500000000000005,-25.4));
#55198=CARTESIAN_POINT('',(34.5,6.46233547508513E-15,-25.4));
#55199=CARTESIAN_POINT('',(35.,0.500000000000005,-25.4));
#55200=CARTESIAN_POINT('Origin',(30.9292009086072,-2.,-104.175753233145));
#55201=CARTESIAN_POINT('',(28.9973492560291,-1.48236190979496,-59.4));
#55202=CARTESIAN_POINT('',(28.9973492560291,-1.48236190979496,-13.4));
#55203=CARTESIAN_POINT('Origin',(30.9292009086072,-2.,-59.4));
#55204=CARTESIAN_POINT('Origin',(-8.55,-12.0328932188134,-3.45));
#55205=CARTESIAN_POINT('',(12.3307106781187,-16.45,-3.45));
#55206=CARTESIAN_POINT('',(22.1792893218814,-16.45,-3.45));
#55207=CARTESIAN_POINT('',(12.3307106781187,-16.45,-3.45));
#55208=CARTESIAN_POINT('',(23.15,-15.4792893218813,-3.45));
#55209=CARTESIAN_POINT('',(22.1792893218814,-16.45,-3.45));
#55210=CARTESIAN_POINT('',(23.15,11.9792893218814,-3.45));
#55211=CARTESIAN_POINT('',(23.15,-15.4792893218813,-3.45));
#55212=CARTESIAN_POINT('',(22.1792893218813,12.95,-3.45));
#55213=CARTESIAN_POINT('',(23.15,11.9792893218814,-3.45));
#55214=CARTESIAN_POINT('',(-22.1792893218813,12.95,-3.45));
#55215=CARTESIAN_POINT('',(22.1792893218813,12.95,-3.45));
#55216=CARTESIAN_POINT('',(-23.15,11.9792893218814,-3.45));
#55217=CARTESIAN_POINT('',(-22.1792893218813,12.95,-3.45));
#55218=CARTESIAN_POINT('',(-23.15,-15.4792893218813,-3.45));
#55219=CARTESIAN_POINT('',(-23.15,11.9792893218814,-3.45));
#55220=CARTESIAN_POINT('',(-22.1792893218814,-16.45,-3.45));
#55221=CARTESIAN_POINT('',(-23.15,-15.4792893218813,-3.45));
#55222=CARTESIAN_POINT('',(-12.3307106781186,-16.45,-3.45));
#55223=CARTESIAN_POINT('',(-22.1792893218814,-16.45,-3.45));
#55224=CARTESIAN_POINT('',(-8.23180194846605,-12.3510912703474,-3.45));
#55225=CARTESIAN_POINT('',(-12.3307106781186,-16.45,-3.45));
#55226=CARTESIAN_POINT('',(-8.1,-12.0328932188134,-3.45));
#55227=CARTESIAN_POINT('Origin',(-8.55,-12.0328932188134,-3.45));
#55228=CARTESIAN_POINT('',(-8.1,-8.40710678118654,-3.45));
#55229=CARTESIAN_POINT('',(-8.1,-12.0328932188134,-3.45));
#55230=CARTESIAN_POINT('',(-8.23180194846605,-8.0889087296526,-3.45));
#55231=CARTESIAN_POINT('Origin',(-8.55,-8.40710678118654,-3.45));
#55232=CARTESIAN_POINT('',(-8.60795233719346,-7.7127583409252,-3.45));
#55233=CARTESIAN_POINT('',(-8.23180194846605,-8.0889087296526,-3.45));
#55234=CARTESIAN_POINT('',(-8.76432075605962,-7.39577200905833,-3.45));
#55235=CARTESIAN_POINT('Origin',(-8.21904360754086,-7.32384961127259,-3.45));
#55236=CARTESIAN_POINT('',(-10.7007720090583,-5.45932075605962,-3.45));
#55237=CARTESIAN_POINT('Origin',(-10.995,-7.69,-3.45));
#55238=CARTESIAN_POINT('',(-11.0177583409252,-5.30295233719346,-3.45));
#55239=CARTESIAN_POINT('Origin',(-10.6288496112726,-4.91404360754086,-3.45));
#55240=CARTESIAN_POINT('',(-11.3889087296526,-4.93180194846607,-3.45));
#55241=CARTESIAN_POINT('',(-11.0177583409252,-5.30295233719346,-3.45));
#55242=CARTESIAN_POINT('',(-11.55,-4.54289321881346,-3.45));
#55243=CARTESIAN_POINT('Origin',(-11.,-4.54289321881346,-3.45));
#55244=CARTESIAN_POINT('',(-11.55,-3.65710678118656,-3.45));
#55245=CARTESIAN_POINT('',(-11.55,-4.54289321881346,-3.45));
#55246=CARTESIAN_POINT('',(-11.3889087296526,-3.26819805153396,-3.45));
#55247=CARTESIAN_POINT('Origin',(-11.,-3.65710678118656,-3.45));
#55248=CARTESIAN_POINT('',(-11.0177583409252,-2.89704766280654,-3.45));
#55249=CARTESIAN_POINT('',(-11.3889087296526,-3.26819805153396,-3.45));
#55250=CARTESIAN_POINT('',(-10.7007720090583,-2.74067924394038,-3.45));
#55251=CARTESIAN_POINT('Origin',(-10.6288496112726,-3.28595639245914,-3.45));
#55252=CARTESIAN_POINT('',(-8.76432075605962,-0.804227990941668,-3.45));
#55253=CARTESIAN_POINT('Origin',(-10.995,-0.510000000000002,-3.45));
#55254=CARTESIAN_POINT('',(-8.60795233719346,-0.48724165907481,-3.45));
#55255=CARTESIAN_POINT('Origin',(-8.21904360754086,-0.87615038872741,-3.45));
#55256=CARTESIAN_POINT('',(-8.07071067811865,0.0499999999999998,-3.45));
#55257=CARTESIAN_POINT('',(-8.60795233719346,-0.487241659074809,-3.45));
#55258=CARTESIAN_POINT('',(8.07071067811865,0.0500000000000006,-3.45));
#55259=CARTESIAN_POINT('',(-8.07071067811865,0.0499999999999998,-3.45));
#55260=CARTESIAN_POINT('',(8.60795233719346,-0.487241659074806,-3.45));
#55261=CARTESIAN_POINT('',(8.07071067811865,0.0500000000000006,-3.45));
#55262=CARTESIAN_POINT('',(8.76432075605962,-0.804227990941667,-3.45));
#55263=CARTESIAN_POINT('Origin',(8.21904360754086,-0.876150388727407,-3.45));
#55264=CARTESIAN_POINT('',(10.7007720090583,-2.74067924394038,-3.45));
#55265=CARTESIAN_POINT('Origin',(10.995,-0.509999999999999,-3.45));
#55266=CARTESIAN_POINT('',(11.0177583409252,-2.89704766280654,-3.45));
#55267=CARTESIAN_POINT('Origin',(10.6288496112726,-3.28595639245914,-3.45));
#55268=CARTESIAN_POINT('',(11.3889087296526,-3.26819805153396,-3.45));
#55269=CARTESIAN_POINT('',(11.0177583409252,-2.89704766280654,-3.45));
#55270=CARTESIAN_POINT('',(11.55,-3.65710678118656,-3.45));
#55271=CARTESIAN_POINT('Origin',(11.,-3.65710678118656,-3.45));
#55272=CARTESIAN_POINT('',(11.55,-4.54289321881346,-3.45));
#55273=CARTESIAN_POINT('',(11.55,-3.65710678118656,-3.45));
#55274=CARTESIAN_POINT('',(11.3889087296526,-4.93180194846606,-3.45));
#55275=CARTESIAN_POINT('Origin',(11.,-4.54289321881346,-3.45));
#55276=CARTESIAN_POINT('',(11.0177583409252,-5.30295233719346,-3.45));
#55277=CARTESIAN_POINT('',(11.3889087296526,-4.93180194846606,-3.45));
#55278=CARTESIAN_POINT('',(10.7007720090583,-5.45932075605962,-3.45));
#55279=CARTESIAN_POINT('Origin',(10.6288496112726,-4.91404360754086,-3.45));
#55280=CARTESIAN_POINT('',(8.76432075605962,-7.39577200905833,-3.45));
#55281=CARTESIAN_POINT('Origin',(10.995,-7.69,-3.45));
#55282=CARTESIAN_POINT('',(8.60795233719346,-7.71275834092519,-3.45));
#55283=CARTESIAN_POINT('Origin',(8.21904360754086,-7.32384961127259,-3.45));
#55284=CARTESIAN_POINT('',(8.23180194846606,-8.08890872965259,-3.45));
#55285=CARTESIAN_POINT('',(8.60795233719346,-7.71275834092519,-3.45));
#55286=CARTESIAN_POINT('',(8.1,-8.40710678118654,-3.45));
#55287=CARTESIAN_POINT('Origin',(8.55,-8.40710678118654,-3.45));
#55288=CARTESIAN_POINT('',(8.1,-12.0328932188134,-3.45));
#55289=CARTESIAN_POINT('',(8.1,-8.40710678118654,-3.45));
#55290=CARTESIAN_POINT('',(8.23180194846605,-12.3510912703474,-3.45));
#55291=CARTESIAN_POINT('Origin',(8.55,-12.0328932188134,-3.45));
#55292=CARTESIAN_POINT('',(8.23180194846605,-12.3510912703474,-3.45));
#55293=CARTESIAN_POINT('Origin',(34.5,6.46233547508513E-15,-104.175753233145));
#55294=CARTESIAN_POINT('',(35.,0.500000000000005,-59.4));
#55295=CARTESIAN_POINT('',(35.,0.500000000000007,-104.175753233145));
#55296=CARTESIAN_POINT('',(34.5,6.46233547508513E-15,-59.4));
#55297=CARTESIAN_POINT('Origin',(-34.5,0.500000000000005,-104.175753233145));
#55298=CARTESIAN_POINT('',(-34.5,0.500000000000005,-59.4));
#55299=CARTESIAN_POINT('',(-34.5,0.500000000000005,-104.175753233145));
#55300=CARTESIAN_POINT('',(-34.5,0.500000000000005,-59.4));
#55301=CARTESIAN_POINT('Origin',(0.,0.,-59.4));
#55302=CARTESIAN_POINT('',(-25.7,0.500000000000004,-59.4));
#55303=CARTESIAN_POINT('',(-25.7,-13.788236863595,-59.4));
#55304=CARTESIAN_POINT('',(-25.7,0.500000000000004,-59.4));
#55305=CARTESIAN_POINT('',(-29.3945469326493,4.36391374425416E-15,-59.4));
#55306=CARTESIAN_POINT('',(-35.,0.500000000000005,-59.4));
#55307=CARTESIAN_POINT('Origin',(-25.7,0.500000000000004,-59.4));
#55308=CARTESIAN_POINT('',(-25.7,0.500000000000004,-60.1660798485821));
#55309=CARTESIAN_POINT('',(-25.7,0.500000000000004,-59.4));
#55310=CARTESIAN_POINT('',(-25.7,-13.788236863595,-60.1660798485821));
#55311=CARTESIAN_POINT('',(-25.7,24.2065391822594,-60.1660798485822));
#55312=CARTESIAN_POINT('',(-25.7,-13.788236863595,-104.175753233145));
#55313=CARTESIAN_POINT('Origin',(0.,0.,-59.4));
#55314=CARTESIAN_POINT('',(25.7,0.500000000000004,-59.4));
#55315=CARTESIAN_POINT('',(35.,0.500000000000005,-59.4));
#55316=CARTESIAN_POINT('',(25.7,-13.788236863595,-59.4));
#55317=CARTESIAN_POINT('',(29.3945469326493,4.36391374425416E-15,-59.4));
#55318=CARTESIAN_POINT('',(25.7,0.500000000000004,-59.4));
#55319=CARTESIAN_POINT('Origin',(25.7,0.500000000000004,-59.4));
#55320=CARTESIAN_POINT('',(25.7,-13.788236863595,-60.1660798485821));
#55321=CARTESIAN_POINT('',(25.7,-13.788236863595,-104.175753233145));
#55322=CARTESIAN_POINT('',(25.7,0.499999999999997,-60.1660798485821));
#55323=CARTESIAN_POINT('',(25.7,24.2065391822594,-60.1660798485821));
#55324=CARTESIAN_POINT('',(25.7,0.500000000000004,-59.4));
#55325=CARTESIAN_POINT('Origin',(-1.54689479616415E-14,13.,-76.7));
#55326=CARTESIAN_POINT('Origin',(-29.3945469326493,4.36391374425416E-15,
-104.175753233145));
#55327=CARTESIAN_POINT('Origin',(-28.5,-3.33849460240199,-64.9));
#55328=CARTESIAN_POINT('Origin',(-28.5,-3.33849460240201,-19.9));
#55329=CARTESIAN_POINT('Origin',(35.,0.500000000000005,-25.4));
#55330=CARTESIAN_POINT('',(25.7,0.499999999999997,-15.1660798485821));
#55331=CARTESIAN_POINT('Origin',(28.5,0.499999999999997,-19.9));
#55332=CARTESIAN_POINT('',(35.,0.500000000000005,-13.4));
#55333=CARTESIAN_POINT('',(35.,0.500000000000007,-104.175753233145));
#55334=CARTESIAN_POINT('',(25.7,0.500000000000004,-13.4));
#55335=CARTESIAN_POINT('',(35.,0.500000000000005,-13.4));
#55336=CARTESIAN_POINT('',(25.7,0.500000000000004,-25.4));
#55337=CARTESIAN_POINT('Origin',(25.7,0.500000000000004,-25.4));
#55338=CARTESIAN_POINT('',(25.7,-13.788236863595,-13.4));
#55339=CARTESIAN_POINT('',(25.7,-13.788236863595,-15.1660798485821));
#55340=CARTESIAN_POINT('',(25.7,-13.788236863595,-104.175753233145));
#55341=CARTESIAN_POINT('',(25.7,24.2065391822594,-15.1660798485821));
#55342=CARTESIAN_POINT('',(25.7,0.500000000000004,-13.4));
#55343=CARTESIAN_POINT('Origin',(-29.3945469326493,4.36391374425416E-15,
-104.175753233145));
#55344=CARTESIAN_POINT('',(-25.7,-13.788236863595,-15.1660798485821));
#55345=CARTESIAN_POINT('Origin',(-28.5,-3.33849460240201,-19.9));
#55346=CARTESIAN_POINT('',(-25.7,-13.788236863595,-13.4));
#55347=CARTESIAN_POINT('',(-29.3945469326493,4.36391374425416E-15,-13.4));
#55348=CARTESIAN_POINT('',(-25.7,-13.788236863595,-104.175753233145));
#55349=CARTESIAN_POINT('Origin',(-25.7,-16.5,-25.4));
#55350=CARTESIAN_POINT('',(-25.7,0.500000000000004,-15.1660798485822));
#55351=CARTESIAN_POINT('',(-25.7,0.500000000000004,-13.4));
#55352=CARTESIAN_POINT('',(-25.7,0.500000000000004,-25.4));
#55353=CARTESIAN_POINT('',(-25.7,24.2065391822594,-15.1660798485822));
#55354=CARTESIAN_POINT('',(-25.7,-16.5,-13.4));
#55355=CARTESIAN_POINT('Origin',(-25.7,0.500000000000004,-25.4));
#55356=CARTESIAN_POINT('',(-34.5,0.500000000000005,-13.4));
#55357=CARTESIAN_POINT('',(-25.7,0.500000000000004,-13.4));
#55358=CARTESIAN_POINT('',(-34.5,0.500000000000005,-104.175753233145));
#55359=CARTESIAN_POINT('Origin',(-28.5,0.500000000000004,-19.9));
#55360=CARTESIAN_POINT('Origin',(29.3945469326493,4.36391374425416E-15,
-104.175753233145));
#55361=CARTESIAN_POINT('',(25.4958861827765,-14.55,-15.2929076226792));
#55362=CARTESIAN_POINT('Origin',(28.5,-3.33849460240214,-19.9));
#55363=CARTESIAN_POINT('',(25.4958861827765,-14.55,-13.4));
#55364=CARTESIAN_POINT('',(29.3945469326493,4.36391374425416E-15,-13.4));
#55365=CARTESIAN_POINT('',(25.4958861827765,-14.55,-104.175753233145));
#55366=CARTESIAN_POINT('Origin',(29.3945469326493,4.36391374425416E-15,
-104.175753233145));
#55367=CARTESIAN_POINT('Origin',(28.5,-3.33849460240214,-64.9));
#55368=CARTESIAN_POINT('Origin',(28.5,-3.33849460240214,-19.9));
#55369=CARTESIAN_POINT('Origin',(12.3307106781187,-16.45,-3.45));
#55370=CARTESIAN_POINT('',(12.3307106781187,-16.45,-3.5));
#55371=CARTESIAN_POINT('',(22.1792893218814,-16.45,-3.5));
#55372=CARTESIAN_POINT('',(12.3307106781187,-16.45,-3.5));
#55373=CARTESIAN_POINT('',(22.1792893218814,-16.45,-3.45));
#55374=CARTESIAN_POINT('',(12.3307106781187,-16.45,-3.45));
#55375=CARTESIAN_POINT('Origin',(22.1792893218814,-16.45,-3.45));
#55376=CARTESIAN_POINT('',(23.15,-15.4792893218813,-3.5));
#55377=CARTESIAN_POINT('',(22.1792893218814,-16.45,-3.5));
#55378=CARTESIAN_POINT('',(23.15,-15.4792893218813,-3.45));
#55379=CARTESIAN_POINT('Origin',(23.15,-15.4792893218813,-3.45));
#55380=CARTESIAN_POINT('',(23.15,11.9792893218814,-3.5));
#55381=CARTESIAN_POINT('',(23.15,-15.4792893218813,-3.5));
#55382=CARTESIAN_POINT('',(23.15,11.9792893218814,-3.45));
#55383=CARTESIAN_POINT('Origin',(23.15,11.9792893218814,-3.45));
#55384=CARTESIAN_POINT('',(22.1792893218813,12.95,-3.5));
#55385=CARTESIAN_POINT('',(23.15,11.9792893218814,-3.5));
#55386=CARTESIAN_POINT('',(22.1792893218813,12.95,-3.45));
#55387=CARTESIAN_POINT('Origin',(22.1792893218813,12.95,-3.45));
#55388=CARTESIAN_POINT('',(-22.1792893218813,12.95,-3.5));
#55389=CARTESIAN_POINT('',(22.1792893218813,12.95,-3.5));
#55390=CARTESIAN_POINT('',(-22.1792893218813,12.95,-3.45));
#55391=CARTESIAN_POINT('Origin',(-22.1792893218813,12.95,-3.45));
#55392=CARTESIAN_POINT('',(-23.15,11.9792893218814,-3.5));
#55393=CARTESIAN_POINT('',(-22.1792893218813,12.95,-3.5));
#55394=CARTESIAN_POINT('',(-23.15,11.9792893218814,-3.45));
#55395=CARTESIAN_POINT('Origin',(-23.15,11.9792893218814,-3.45));
#55396=CARTESIAN_POINT('',(-23.15,-15.4792893218813,-3.5));
#55397=CARTESIAN_POINT('',(-23.15,11.9792893218814,-3.5));
#55398=CARTESIAN_POINT('',(-23.15,-15.4792893218813,-3.45));
#55399=CARTESIAN_POINT('Origin',(-23.15,-15.4792893218813,-3.45));
#55400=CARTESIAN_POINT('',(-22.1792893218814,-16.45,-3.5));
#55401=CARTESIAN_POINT('',(-23.15,-15.4792893218813,-3.5));
#55402=CARTESIAN_POINT('',(-22.1792893218814,-16.45,-3.45));
#55403=CARTESIAN_POINT('Origin',(-22.1792893218814,-16.45,-3.45));
#55404=CARTESIAN_POINT('',(-12.3307106781186,-16.45,-3.5));
#55405=CARTESIAN_POINT('',(-22.1792893218814,-16.45,-3.5));
#55406=CARTESIAN_POINT('',(-12.3307106781186,-16.45,-3.45));
#55407=CARTESIAN_POINT('Origin',(-12.3307106781186,-16.45,-3.45));
#55408=CARTESIAN_POINT('',(-8.23180194846605,-12.3510912703474,-3.5));
#55409=CARTESIAN_POINT('',(-12.3307106781186,-16.45,-3.5));
#55410=CARTESIAN_POINT('',(-8.23180194846605,-12.3510912703474,-3.45));
#55411=CARTESIAN_POINT('Origin',(-8.55,-12.0328932188134,-3.45));
#55412=CARTESIAN_POINT('',(-8.1,-12.0328932188134,-3.5));
#55413=CARTESIAN_POINT('Origin',(-8.55,-12.0328932188134,-3.5));
#55414=CARTESIAN_POINT('',(-8.1,-12.0328932188134,-3.45));
#55415=CARTESIAN_POINT('Origin',(-8.1,-12.0328932188134,-3.45));
#55416=CARTESIAN_POINT('',(-8.1,-8.40710678118654,-3.5));
#55417=CARTESIAN_POINT('',(-8.1,-12.0328932188134,-3.5));
#55418=CARTESIAN_POINT('',(-8.1,-8.40710678118654,-3.45));
#55419=CARTESIAN_POINT('Origin',(-8.55,-8.40710678118654,-3.45));
#55420=CARTESIAN_POINT('',(-8.23180194846605,-8.0889087296526,-3.5));
#55421=CARTESIAN_POINT('Origin',(-8.55,-8.40710678118654,-3.5));
#55422=CARTESIAN_POINT('',(-8.23180194846605,-8.0889087296526,-3.45));
#55423=CARTESIAN_POINT('Origin',(-8.23180194846605,-8.0889087296526,-3.45));
#55424=CARTESIAN_POINT('',(-8.60795233719346,-7.7127583409252,-3.5));
#55425=CARTESIAN_POINT('',(-8.23180194846605,-8.0889087296526,-3.5));
#55426=CARTESIAN_POINT('',(-8.60795233719346,-7.7127583409252,-3.45));
#55427=CARTESIAN_POINT('Origin',(-8.21904360754086,-7.32384961127259,-3.45));
#55428=CARTESIAN_POINT('',(-8.76432075605962,-7.39577200905833,-3.5));
#55429=CARTESIAN_POINT('Origin',(-8.21904360754086,-7.32384961127259,-3.5));
#55430=CARTESIAN_POINT('',(-8.76432075605962,-7.39577200905833,-3.45));
#55431=CARTESIAN_POINT('Origin',(-10.995,-7.69,-3.45));
#55432=CARTESIAN_POINT('',(-10.7007720090583,-5.45932075605962,-3.5));
#55433=CARTESIAN_POINT('Origin',(-10.995,-7.69,-3.5));
#55434=CARTESIAN_POINT('',(-10.7007720090583,-5.45932075605962,-3.45));
#55435=CARTESIAN_POINT('Origin',(-10.6288496112726,-4.91404360754086,-3.45));
#55436=CARTESIAN_POINT('',(-11.0177583409252,-5.30295233719346,-3.5));
#55437=CARTESIAN_POINT('Origin',(-10.6288496112726,-4.91404360754086,-3.5));
#55438=CARTESIAN_POINT('',(-11.0177583409252,-5.30295233719346,-3.45));
#55439=CARTESIAN_POINT('Origin',(-11.0177583409252,-5.30295233719346,-3.45));
#55440=CARTESIAN_POINT('',(-11.3889087296526,-4.93180194846607,-3.5));
#55441=CARTESIAN_POINT('',(-11.0177583409252,-5.30295233719346,-3.5));
#55442=CARTESIAN_POINT('',(-11.3889087296526,-4.93180194846607,-3.45));
#55443=CARTESIAN_POINT('Origin',(-11.,-4.54289321881346,-3.45));
#55444=CARTESIAN_POINT('',(-11.55,-4.54289321881346,-3.5));
#55445=CARTESIAN_POINT('Origin',(-11.,-4.54289321881346,-3.5));
#55446=CARTESIAN_POINT('',(-11.55,-4.54289321881346,-3.45));
#55447=CARTESIAN_POINT('Origin',(-11.55,-4.54289321881346,-3.45));
#55448=CARTESIAN_POINT('',(-11.55,-3.65710678118656,-3.5));
#55449=CARTESIAN_POINT('',(-11.55,-4.54289321881346,-3.5));
#55450=CARTESIAN_POINT('',(-11.55,-3.65710678118656,-3.45));
#55451=CARTESIAN_POINT('Origin',(-11.,-3.65710678118656,-3.45));
#55452=CARTESIAN_POINT('',(-11.3889087296526,-3.26819805153396,-3.5));
#55453=CARTESIAN_POINT('Origin',(-11.,-3.65710678118656,-3.5));
#55454=CARTESIAN_POINT('',(-11.3889087296526,-3.26819805153396,-3.45));
#55455=CARTESIAN_POINT('Origin',(-11.3889087296526,-3.26819805153396,-3.45));
#55456=CARTESIAN_POINT('',(-11.0177583409252,-2.89704766280654,-3.5));
#55457=CARTESIAN_POINT('',(-11.3889087296526,-3.26819805153396,-3.5));
#55458=CARTESIAN_POINT('',(-11.0177583409252,-2.89704766280654,-3.45));
#55459=CARTESIAN_POINT('Origin',(-10.6288496112726,-3.28595639245914,-3.45));
#55460=CARTESIAN_POINT('',(-10.7007720090583,-2.74067924394038,-3.5));
#55461=CARTESIAN_POINT('Origin',(-10.6288496112726,-3.28595639245914,-3.5));
#55462=CARTESIAN_POINT('',(-10.7007720090583,-2.74067924394038,-3.45));
#55463=CARTESIAN_POINT('Origin',(-10.995,-0.510000000000002,-3.45));
#55464=CARTESIAN_POINT('',(-8.76432075605962,-0.804227990941668,-3.5));
#55465=CARTESIAN_POINT('Origin',(-10.995,-0.510000000000002,-3.5));
#55466=CARTESIAN_POINT('',(-8.76432075605962,-0.804227990941668,-3.45));
#55467=CARTESIAN_POINT('Origin',(-8.21904360754086,-0.87615038872741,-3.45));
#55468=CARTESIAN_POINT('',(-8.60795233719346,-0.48724165907481,-3.5));
#55469=CARTESIAN_POINT('Origin',(-8.21904360754086,-0.87615038872741,-3.5));
#55470=CARTESIAN_POINT('',(-8.60795233719346,-0.48724165907481,-3.45));
#55471=CARTESIAN_POINT('Origin',(-8.60795233719346,-0.487241659074809,-3.45));
#55472=CARTESIAN_POINT('',(-8.07071067811865,0.0499999999999998,-3.5));
#55473=CARTESIAN_POINT('',(-8.60795233719346,-0.487241659074809,-3.5));
#55474=CARTESIAN_POINT('',(-8.07071067811865,0.0499999999999998,-3.45));
#55475=CARTESIAN_POINT('Origin',(-8.07071067811865,0.0499999999999998,-3.45));
#55476=CARTESIAN_POINT('',(8.07071067811865,0.0500000000000006,-3.5));
#55477=CARTESIAN_POINT('',(-8.07071067811865,0.0499999999999998,-3.5));
#55478=CARTESIAN_POINT('',(8.07071067811865,0.0500000000000006,-3.45));
#55479=CARTESIAN_POINT('Origin',(8.07071067811865,0.0500000000000006,-3.45));
#55480=CARTESIAN_POINT('',(8.60795233719346,-0.487241659074806,-3.5));
#55481=CARTESIAN_POINT('',(8.07071067811865,0.0500000000000006,-3.5));
#55482=CARTESIAN_POINT('',(8.60795233719346,-0.487241659074806,-3.45));
#55483=CARTESIAN_POINT('Origin',(8.21904360754086,-0.876150388727407,-3.45));
#55484=CARTESIAN_POINT('',(8.76432075605962,-0.804227990941667,-3.5));
#55485=CARTESIAN_POINT('Origin',(8.21904360754086,-0.876150388727407,-3.5));
#55486=CARTESIAN_POINT('',(8.76432075605962,-0.804227990941667,-3.45));
#55487=CARTESIAN_POINT('Origin',(10.995,-0.509999999999999,-3.45));
#55488=CARTESIAN_POINT('',(10.7007720090583,-2.74067924394038,-3.5));
#55489=CARTESIAN_POINT('Origin',(10.995,-0.509999999999999,-3.5));
#55490=CARTESIAN_POINT('',(10.7007720090583,-2.74067924394038,-3.45));
#55491=CARTESIAN_POINT('Origin',(10.6288496112726,-3.28595639245914,-3.45));
#55492=CARTESIAN_POINT('',(11.0177583409252,-2.89704766280654,-3.5));
#55493=CARTESIAN_POINT('Origin',(10.6288496112726,-3.28595639245914,-3.5));
#55494=CARTESIAN_POINT('',(11.0177583409252,-2.89704766280654,-3.45));
#55495=CARTESIAN_POINT('Origin',(11.0177583409252,-2.89704766280654,-3.45));
#55496=CARTESIAN_POINT('',(11.3889087296526,-3.26819805153396,-3.5));
#55497=CARTESIAN_POINT('',(11.0177583409252,-2.89704766280654,-3.5));
#55498=CARTESIAN_POINT('',(11.3889087296526,-3.26819805153396,-3.45));
#55499=CARTESIAN_POINT('Origin',(11.,-3.65710678118656,-3.45));
#55500=CARTESIAN_POINT('',(11.55,-3.65710678118656,-3.5));
#55501=CARTESIAN_POINT('Origin',(11.,-3.65710678118656,-3.5));
#55502=CARTESIAN_POINT('',(11.55,-3.65710678118656,-3.45));
#55503=CARTESIAN_POINT('Origin',(11.55,-3.65710678118656,-3.45));
#55504=CARTESIAN_POINT('',(11.55,-4.54289321881346,-3.5));
#55505=CARTESIAN_POINT('',(11.55,-3.65710678118656,-3.5));
#55506=CARTESIAN_POINT('',(11.55,-4.54289321881346,-3.45));
#55507=CARTESIAN_POINT('Origin',(11.,-4.54289321881346,-3.45));
#55508=CARTESIAN_POINT('',(11.3889087296526,-4.93180194846606,-3.5));
#55509=CARTESIAN_POINT('Origin',(11.,-4.54289321881346,-3.5));
#55510=CARTESIAN_POINT('',(11.3889087296526,-4.93180194846606,-3.45));
#55511=CARTESIAN_POINT('Origin',(11.3889087296526,-4.93180194846606,-3.45));
#55512=CARTESIAN_POINT('',(11.0177583409252,-5.30295233719346,-3.5));
#55513=CARTESIAN_POINT('',(11.3889087296526,-4.93180194846606,-3.5));
#55514=CARTESIAN_POINT('',(11.0177583409252,-5.30295233719346,-3.45));
#55515=CARTESIAN_POINT('Origin',(10.6288496112726,-4.91404360754086,-3.45));
#55516=CARTESIAN_POINT('',(10.7007720090583,-5.45932075605962,-3.5));
#55517=CARTESIAN_POINT('Origin',(10.6288496112726,-4.91404360754086,-3.5));
#55518=CARTESIAN_POINT('',(10.7007720090583,-5.45932075605962,-3.45));
#55519=CARTESIAN_POINT('Origin',(10.995,-7.69,-3.45));
#55520=CARTESIAN_POINT('',(8.76432075605962,-7.39577200905833,-3.5));
#55521=CARTESIAN_POINT('Origin',(10.995,-7.69,-3.5));
#55522=CARTESIAN_POINT('',(8.76432075605962,-7.39577200905833,-3.45));
#55523=CARTESIAN_POINT('Origin',(8.21904360754086,-7.32384961127259,-3.45));
#55524=CARTESIAN_POINT('',(8.60795233719346,-7.71275834092519,-3.5));
#55525=CARTESIAN_POINT('Origin',(8.21904360754086,-7.32384961127259,-3.5));
#55526=CARTESIAN_POINT('',(8.60795233719346,-7.71275834092519,-3.45));
#55527=CARTESIAN_POINT('Origin',(8.60795233719346,-7.71275834092519,-3.45));
#55528=CARTESIAN_POINT('',(8.23180194846606,-8.08890872965259,-3.5));
#55529=CARTESIAN_POINT('',(8.60795233719346,-7.71275834092519,-3.5));
#55530=CARTESIAN_POINT('',(8.23180194846606,-8.08890872965259,-3.45));
#55531=CARTESIAN_POINT('Origin',(8.55,-8.40710678118654,-3.45));
#55532=CARTESIAN_POINT('',(8.1,-8.40710678118654,-3.5));
#55533=CARTESIAN_POINT('Origin',(8.55,-8.40710678118654,-3.5));
#55534=CARTESIAN_POINT('',(8.1,-8.40710678118654,-3.45));
#55535=CARTESIAN_POINT('Origin',(8.1,-8.40710678118654,-3.45));
#55536=CARTESIAN_POINT('',(8.1,-12.0328932188134,-3.5));
#55537=CARTESIAN_POINT('',(8.1,-8.40710678118654,-3.5));
#55538=CARTESIAN_POINT('',(8.1,-12.0328932188134,-3.45));
#55539=CARTESIAN_POINT('Origin',(8.55,-12.0328932188134,-3.45));
#55540=CARTESIAN_POINT('',(8.23180194846605,-12.3510912703474,-3.5));
#55541=CARTESIAN_POINT('Origin',(8.55,-12.0328932188134,-3.5));
#55542=CARTESIAN_POINT('',(8.23180194846605,-12.3510912703474,-3.45));
#55543=CARTESIAN_POINT('Origin',(8.23180194846605,-12.3510912703474,-3.45));
#55544=CARTESIAN_POINT('',(8.23180194846605,-12.3510912703474,-3.5));
#55545=CARTESIAN_POINT('Origin',(-1.64657055886728E-14,13.8,-1.36260717503886E-30));
#55546=CARTESIAN_POINT('',(-4.99999999999999,13.8,-3.5));
#55547=CARTESIAN_POINT('',(5.00000000000001,13.8,-3.5));
#55548=CARTESIAN_POINT('',(-5.8,13.8,-3.5));
#55549=CARTESIAN_POINT('',(5.,13.8,-13.4));
#55550=CARTESIAN_POINT('',(5.,13.8,-13.4));
#55551=CARTESIAN_POINT('',(-4.99999999999999,13.8,-13.4));
#55552=CARTESIAN_POINT('',(-5.8,13.8,-13.4));
#55553=CARTESIAN_POINT('',(-4.99999999999999,13.8,-3.5));
#55554=CARTESIAN_POINT('Origin',(5.00000000000001,13.8,-2.19030741916265E-15));
#55555=CARTESIAN_POINT('',(5.8,13.,-3.5));
#55556=CARTESIAN_POINT('',(5.00000000000001,13.8,-3.5));
#55557=CARTESIAN_POINT('',(5.8,13.,-13.4));
#55558=CARTESIAN_POINT('',(5.8,13.,-13.4));
#55559=CARTESIAN_POINT('',(5.00000000000001,13.8,-13.4));
#55560=CARTESIAN_POINT('Origin',(-22.2,13.,-13.4));
#55561=CARTESIAN_POINT('',(22.2,13.,-3.5));
#55562=CARTESIAN_POINT('',(22.2,13.,-3.5));
#55563=CARTESIAN_POINT('',(22.2,13.,-13.4));
#55564=CARTESIAN_POINT('',(22.2,13.,-13.4));
#55565=CARTESIAN_POINT('',(-22.2,13.,-13.4));
#55566=CARTESIAN_POINT('Origin',(22.2,13.,-13.4));
#55567=CARTESIAN_POINT('',(23.2,12.,-3.5));
#55568=CARTESIAN_POINT('',(23.2,12.,-3.5));
#55569=CARTESIAN_POINT('',(23.2,12.,-13.4));
#55570=CARTESIAN_POINT('',(23.2,12.,-13.4));
#55571=CARTESIAN_POINT('',(22.2,13.,-13.4));
#55572=CARTESIAN_POINT('Origin',(23.2,12.,-13.4));
#55573=CARTESIAN_POINT('',(23.2,-15.5,-3.5));
#55574=CARTESIAN_POINT('',(23.2,-15.5,-3.5));
#55575=CARTESIAN_POINT('',(23.2,-15.5,-13.4));
#55576=CARTESIAN_POINT('',(23.2,-15.5,-13.4));
#55577=CARTESIAN_POINT('',(23.2,12.,-13.4));
#55578=CARTESIAN_POINT('Origin',(-23.2,12.,-13.4));
#55579=CARTESIAN_POINT('',(-23.2,12.,-3.5));
#55580=CARTESIAN_POINT('',(-23.2,-15.5,-3.5));
#55581=CARTESIAN_POINT('',(-23.2,12.,-3.5));
#55582=CARTESIAN_POINT('',(-23.2,12.,-13.4));
#55583=CARTESIAN_POINT('',(-23.2,12.,-13.4));
#55584=CARTESIAN_POINT('',(-23.2,-15.5,-13.4));
#55585=CARTESIAN_POINT('',(-23.2,12.,-13.4));
#55586=CARTESIAN_POINT('',(-23.2,-15.5,-13.4));
#55587=CARTESIAN_POINT('Origin',(-22.2,13.,-13.4));
#55588=CARTESIAN_POINT('',(-22.2,13.,-3.5));
#55589=CARTESIAN_POINT('',(-22.2,13.,-3.5));
#55590=CARTESIAN_POINT('',(-22.2,13.,-13.4));
#55591=CARTESIAN_POINT('',(-22.2,13.,-13.4));
#55592=CARTESIAN_POINT('',(-22.2,13.,-13.4));
#55593=CARTESIAN_POINT('Origin',(-22.2,13.,-13.4));
#55594=CARTESIAN_POINT('',(-5.8,13.,-3.5));
#55595=CARTESIAN_POINT('',(22.2,13.,-3.5));
#55596=CARTESIAN_POINT('',(-5.8,13.,-13.4));
#55597=CARTESIAN_POINT('',(-5.8,13.,-13.4));
#55598=CARTESIAN_POINT('',(-22.2,13.,-13.4));
#55599=CARTESIAN_POINT('Origin',(-4.99999999999999,13.8,-4.38061483832526E-16));
#55600=CARTESIAN_POINT('',(-4.99999999999999,13.8,-13.4));
#55601=CARTESIAN_POINT('',(-4.99999999999999,13.8,-3.5));
#55602=CARTESIAN_POINT('Origin',(35.,13.,-104.175753233145));
#55603=CARTESIAN_POINT('',(35.,13.,-13.4));
#55604=CARTESIAN_POINT('',(35.,13.,-13.4));
#55605=CARTESIAN_POINT('',(35.,0.500000000000005,-71.4));
#55606=CARTESIAN_POINT('',(35.,0.500000000000005,-59.4));
#55607=CARTESIAN_POINT('',(35.,13.,-71.4));
#55608=CARTESIAN_POINT('',(35.,13.,-71.4));
#55609=CARTESIAN_POINT('',(35.,13.,-104.175753233145));
#55610=CARTESIAN_POINT('Origin',(34.,14.,-104.175753233145));
#55611=CARTESIAN_POINT('',(34.,14.,-71.4));
#55612=CARTESIAN_POINT('',(34.,14.,-71.4));
#55613=CARTESIAN_POINT('',(34.,14.,-13.4));
#55614=CARTESIAN_POINT('',(34.,14.,-104.175753233145));
#55615=CARTESIAN_POINT('',(34.,14.,-13.4));
#55616=CARTESIAN_POINT('Origin',(-23.,14.,-84.8));
#55617=CARTESIAN_POINT('',(17.505,14.,-71.4));
#55618=CARTESIAN_POINT('',(17.505,14.,-13.4));
#55619=CARTESIAN_POINT('',(17.505,14.,-83.0807063142603));
#55620=CARTESIAN_POINT('',(23.,14.,-13.4));
#55621=CARTESIAN_POINT('',(23.,14.,-71.4));
#55622=CARTESIAN_POINT('Origin',(17.005,13.5,-83.0807063142603));
#55623=CARTESIAN_POINT('',(17.005,13.5,-71.4));
#55624=CARTESIAN_POINT('',(17.005,13.5,-13.4));
#55625=CARTESIAN_POINT('',(17.005,13.5,-83.0807063142603));
#55626=CARTESIAN_POINT('',(17.005,13.5,-13.4));
#55627=CARTESIAN_POINT('',(17.005,13.5,-71.4));
#55628=CARTESIAN_POINT('Origin',(17.005,13.5,-83.0807063142603));
#55629=CARTESIAN_POINT('',(6.33500000000001,13.5,-71.4));
#55630=CARTESIAN_POINT('',(6.33500000000001,13.5,-13.4));
#55631=CARTESIAN_POINT('',(6.33500000000001,13.5,-83.0807063142603));
#55632=CARTESIAN_POINT('',(17.005,13.5,-13.4));
#55633=CARTESIAN_POINT('',(17.005,13.5,-71.4));
#55634=CARTESIAN_POINT('Origin',(6.33500000000001,13.5,-83.0807063142603));
#55635=CARTESIAN_POINT('',(5.835,14.,-71.4));
#55636=CARTESIAN_POINT('',(5.835,14.,-13.4));
#55637=CARTESIAN_POINT('',(5.835,14.,-83.0807063142603));
#55638=CARTESIAN_POINT('',(6.33500000000001,13.5,-13.4));
#55639=CARTESIAN_POINT('',(6.33500000000001,13.5,-71.4));
#55640=CARTESIAN_POINT('Origin',(-23.,14.,-84.8));
#55641=CARTESIAN_POINT('',(-5.835,14.,-71.4));
#55642=CARTESIAN_POINT('',(23.,14.,-71.4));
#55643=CARTESIAN_POINT('',(-5.835,14.,-13.4));
#55644=CARTESIAN_POINT('',(-5.835,14.,-83.0807063142603));
#55645=CARTESIAN_POINT('',(23.,14.,-13.4));
#55646=CARTESIAN_POINT('Origin',(-6.33500000000001,13.5,-83.0807063142603));
#55647=CARTESIAN_POINT('',(-6.33500000000001,13.5,-71.4));
#55648=CARTESIAN_POINT('',(-6.33500000000001,13.5,-13.4));
#55649=CARTESIAN_POINT('',(-6.33500000000001,13.5,-83.0807063142603));
#55650=CARTESIAN_POINT('',(-6.33500000000001,13.5,-13.4));
#55651=CARTESIAN_POINT('',(-6.33500000000001,13.5,-71.4));
#55652=CARTESIAN_POINT('Origin',(-17.005,13.5,-83.0807063142603));
#55653=CARTESIAN_POINT('',(-17.005,13.5,-71.4));
#55654=CARTESIAN_POINT('',(-17.005,13.5,-13.4));
#55655=CARTESIAN_POINT('',(-17.005,13.5,-83.0807063142603));
#55656=CARTESIAN_POINT('',(-17.005,13.5,-13.4));
#55657=CARTESIAN_POINT('',(-17.005,13.5,-71.4));
#55658=CARTESIAN_POINT('Origin',(-17.005,13.5,-83.0807063142603));
#55659=CARTESIAN_POINT('',(-17.505,14.,-71.4));
#55660=CARTESIAN_POINT('',(-17.505,14.,-13.4));
#55661=CARTESIAN_POINT('',(-17.505,14.,-83.0807063142603));
#55662=CARTESIAN_POINT('',(-17.005,13.5,-13.4));
#55663=CARTESIAN_POINT('',(-17.005,13.5,-71.4));
#55664=CARTESIAN_POINT('Origin',(-23.,14.,-84.8));
#55665=CARTESIAN_POINT('',(-34.,14.,-71.4));
#55666=CARTESIAN_POINT('',(23.,14.,-71.4));
#55667=CARTESIAN_POINT('',(-34.,14.,-13.4));
#55668=CARTESIAN_POINT('',(-34.,14.,-104.175753233145));
#55669=CARTESIAN_POINT('',(23.,14.,-13.4));
#55670=CARTESIAN_POINT('Origin',(-34.,14.,-104.175753233145));
#55671=CARTESIAN_POINT('',(-35.,13.,-71.4));
#55672=CARTESIAN_POINT('',(-34.,14.,-71.4));
#55673=CARTESIAN_POINT('',(-35.,13.,-13.4));
#55674=CARTESIAN_POINT('',(-35.,13.,-104.175753233145));
#55675=CARTESIAN_POINT('',(-34.,14.,-13.4));
#55676=CARTESIAN_POINT('Origin',(-35.,13.,-104.175753233145));
#55677=CARTESIAN_POINT('',(-35.,5.6,-71.4));
#55678=CARTESIAN_POINT('',(-35.,13.,-71.4));
#55679=CARTESIAN_POINT('',(-35.,5.6,-13.4));
#55680=CARTESIAN_POINT('',(-35.,5.6,-104.175753233145));
#55681=CARTESIAN_POINT('',(-35.,13.,-13.4));
#55682=CARTESIAN_POINT('Origin',(-35.,5.6,-104.175753233145));
#55683=CARTESIAN_POINT('',(-34.5,5.10000000000001,-71.4));
#55684=CARTESIAN_POINT('',(-35.,5.6,-71.4));
#55685=CARTESIAN_POINT('',(-34.5,5.10000000000001,-13.4));
#55686=CARTESIAN_POINT('',(-34.5,5.10000000000001,-104.175753233145));
#55687=CARTESIAN_POINT('',(-35.,5.6,-13.4));
#55688=CARTESIAN_POINT('Origin',(-34.5,5.10000000000001,-104.175753233145));
#55689=CARTESIAN_POINT('',(-34.5,0.500000000000005,-71.4));
#55690=CARTESIAN_POINT('',(-34.5,5.10000000000001,-71.4));
#55691=CARTESIAN_POINT('',(-34.5,0.500000000000005,-104.175753233145));
#55692=CARTESIAN_POINT('',(-34.5,5.10000000000001,-13.4));
#55693=CARTESIAN_POINT('Origin',(-35.,0.500000000000005,-59.4));
#55694=CARTESIAN_POINT('',(-25.7,0.500000000000004,-69.6339201514178));
#55695=CARTESIAN_POINT('Origin',(-28.5,0.500000000000004,-64.9));
#55696=CARTESIAN_POINT('',(-25.7,0.500000000000004,-71.4));
#55697=CARTESIAN_POINT('',(-35.,0.500000000000005,-71.4));
#55698=CARTESIAN_POINT('',(-25.7,0.500000000000004,-59.4));
#55699=CARTESIAN_POINT('Origin',(-25.7,0.500000000000004,-59.4));
#55700=CARTESIAN_POINT('',(-25.7,-13.788236863595,-71.4));
#55701=CARTESIAN_POINT('',(-25.7,-13.788236863595,-69.6339201514178));
#55702=CARTESIAN_POINT('',(-25.7,-13.788236863595,-104.175753233145));
#55703=CARTESIAN_POINT('',(-25.7,24.2065391822594,-69.6339201514178));
#55704=CARTESIAN_POINT('',(-25.7,0.500000000000004,-71.4));
#55705=CARTESIAN_POINT('Origin',(-29.3945469326493,4.36391374425416E-15,
-104.175753233145));
#55706=CARTESIAN_POINT('',(-25.4958861827765,-14.55,-69.5070923773207));
#55707=CARTESIAN_POINT('Origin',(-28.5,-3.33849460240199,-64.9));
#55708=CARTESIAN_POINT('',(-25.4958861827765,-14.55,-71.4));
#55709=CARTESIAN_POINT('',(-29.3945469326493,4.36391374425416E-15,-71.4));
#55710=CARTESIAN_POINT('',(-25.4958861827765,-14.55,-104.175753233145));
#55711=CARTESIAN_POINT('Origin',(29.3945469326493,4.36391374425416E-15,
-104.175753233145));
#55712=CARTESIAN_POINT('',(25.7,-13.788236863595,-69.6339201514178));
#55713=CARTESIAN_POINT('Origin',(28.5,-3.33849460240214,-64.9));
#55714=CARTESIAN_POINT('',(25.7,-13.788236863595,-71.4));
#55715=CARTESIAN_POINT('',(29.3945469326493,4.36391374425416E-15,-71.4));
#55716=CARTESIAN_POINT('',(25.7,-13.788236863595,-104.175753233145));
#55717=CARTESIAN_POINT('Origin',(25.7,0.500000000000004,-59.4));
#55718=CARTESIAN_POINT('',(25.7,0.499999999999997,-69.6339201514178));
#55719=CARTESIAN_POINT('',(25.7,0.500000000000004,-71.4));
#55720=CARTESIAN_POINT('',(25.7,0.500000000000004,-59.4));
#55721=CARTESIAN_POINT('',(25.7,24.2065391822594,-69.6339201514178));
#55722=CARTESIAN_POINT('',(25.7,0.500000000000004,-71.4));
#55723=CARTESIAN_POINT('Origin',(35.,0.500000000000005,-59.4));
#55724=CARTESIAN_POINT('',(35.,0.500000000000005,-71.4));
#55725=CARTESIAN_POINT('Origin',(28.5,0.499999999999997,-64.9));
#55726=CARTESIAN_POINT('Origin',(-25.4958861827765,-14.55,-104.175753233145));
#55727=CARTESIAN_POINT('Origin',(-28.5000000000034,-12.2029290542103,-64.8999999999982));
#55728=CARTESIAN_POINT('',(-23.,-16.5,-71.4));
#55729=CARTESIAN_POINT('',(-25.4958861827765,-14.55,-71.4));
#55730=CARTESIAN_POINT('',(-23.,-16.5,-84.8));
#55731=CARTESIAN_POINT('Origin',(-23.2,-15.5,-13.4));
#55732=CARTESIAN_POINT('',(-22.2,-16.5,-3.5));
#55733=CARTESIAN_POINT('',(-23.2,-15.5,-3.5));
#55734=CARTESIAN_POINT('',(-22.2,-16.5,-13.4));
#55735=CARTESIAN_POINT('',(-23.2,-15.5,-13.4));
#55736=CARTESIAN_POINT('',(-22.2,-16.5,-13.4));
#55737=CARTESIAN_POINT('Origin',(23.2,-15.5,-13.4));
#55738=CARTESIAN_POINT('',(22.2,-16.5,-3.5));
#55739=CARTESIAN_POINT('',(22.2,-16.5,-3.5));
#55740=CARTESIAN_POINT('',(22.2,-16.5,-13.4));
#55741=CARTESIAN_POINT('',(22.2,-16.5,-13.4));
#55742=CARTESIAN_POINT('',(23.2,-15.5,-13.4));
#55743=CARTESIAN_POINT('Origin',(0.,0.,-13.4));
#55744=CARTESIAN_POINT('',(-23.,-16.5,-13.4));
#55745=CARTESIAN_POINT('',(23.,-16.5,-13.4));
#55746=CARTESIAN_POINT('',(22.2,-16.5,-13.4));
#55747=CARTESIAN_POINT('',(25.4958861827765,-14.55,-13.4));
#55748=CARTESIAN_POINT('Origin',(25.4958861827765,-14.55,-104.175753233145));
#55749=CARTESIAN_POINT('Origin',(28.5000000000021,-12.2029290542113,-19.9000000000011));
#55750=CARTESIAN_POINT('',(23.,-16.5,-84.8));
#55751=CARTESIAN_POINT('Origin',(-5.8,13.8,-3.5));
#55752=CARTESIAN_POINT('',(-12.31,-16.5,-3.5));
#55753=CARTESIAN_POINT('',(-22.2,-16.5,-3.5));
#55754=CARTESIAN_POINT('',(-8.19644660940672,-12.3864466094067,-3.5));
#55755=CARTESIAN_POINT('',(-12.31,-16.5,-3.5));
#55756=CARTESIAN_POINT('',(-8.05,-12.0328932188134,-3.5));
#55757=CARTESIAN_POINT('Origin',(-8.55,-12.0328932188134,-3.5));
#55758=CARTESIAN_POINT('',(-8.05,-8.40710678118654,-3.5));
#55759=CARTESIAN_POINT('',(-8.05,-12.0328932188134,-3.5));
#55760=CARTESIAN_POINT('',(-8.19644660940673,-8.05355339059327,-3.5));
#55761=CARTESIAN_POINT('Origin',(-8.55,-8.40710678118654,-3.5));
#55762=CARTESIAN_POINT('',(-8.57259699813413,-7.67740300186587,-3.5));
#55763=CARTESIAN_POINT('',(-8.19644660940673,-8.05355339059327,-3.5));
#55764=CARTESIAN_POINT('',(-8.71475010619428,-7.38923360925963,-3.5));
#55765=CARTESIAN_POINT('Origin',(-8.21904360754086,-7.32384961127259,-3.5));
#55766=CARTESIAN_POINT('',(-10.6942336092596,-5.40975010619428,-3.5));
#55767=CARTESIAN_POINT('Origin',(-10.995,-7.69,-3.5));
#55768=CARTESIAN_POINT('',(-10.9824030018659,-5.26759699813413,-3.5));
#55769=CARTESIAN_POINT('Origin',(-10.6288496112726,-4.91404360754086,-3.5));
#55770=CARTESIAN_POINT('',(-11.3535533905933,-4.89644660940674,-3.5));
#55771=CARTESIAN_POINT('',(-10.9824030018659,-5.26759699813413,-3.5));
#55772=CARTESIAN_POINT('',(-11.5,-4.54289321881346,-3.5));
#55773=CARTESIAN_POINT('Origin',(-11.,-4.54289321881346,-3.5));
#55774=CARTESIAN_POINT('',(-11.5,-3.65710678118656,-3.5));
#55775=CARTESIAN_POINT('',(-11.5,-4.54289321881346,-3.5));
#55776=CARTESIAN_POINT('',(-11.3535533905933,-3.30355339059329,-3.5));
#55777=CARTESIAN_POINT('Origin',(-11.,-3.65710678118656,-3.5));
#55778=CARTESIAN_POINT('',(-10.9824030018659,-2.93240300186587,-3.5));
#55779=CARTESIAN_POINT('',(-11.3535533905933,-3.30355339059329,-3.5));
#55780=CARTESIAN_POINT('',(-10.6942336092596,-2.79024989380572,-3.5));
#55781=CARTESIAN_POINT('Origin',(-10.6288496112726,-3.28595639245914,-3.5));
#55782=CARTESIAN_POINT('',(-8.71475010619428,-0.810766390740372,-3.5));
#55783=CARTESIAN_POINT('Origin',(-10.995,-0.510000000000002,-3.5));
#55784=CARTESIAN_POINT('',(-8.57259699813413,-0.522596998134137,-3.5));
#55785=CARTESIAN_POINT('Origin',(-8.21904360754086,-0.87615038872741,-3.5));
#55786=CARTESIAN_POINT('',(-8.05,-1.60428730688303E-15,-3.5));
#55787=CARTESIAN_POINT('',(-8.57259699813413,-0.522596998134137,-3.5));
#55788=CARTESIAN_POINT('',(8.05,3.67394039744206E-16,-3.5));
#55789=CARTESIAN_POINT('',(-8.05,-1.60428730688303E-15,-3.5));
#55790=CARTESIAN_POINT('',(8.57259699813413,-0.522596998134133,-3.5));
#55791=CARTESIAN_POINT('',(8.05,3.67394039744206E-16,-3.5));
#55792=CARTESIAN_POINT('',(8.71475010619428,-0.81076639074037,-3.5));
#55793=CARTESIAN_POINT('Origin',(8.21904360754086,-0.876150388727407,-3.5));
#55794=CARTESIAN_POINT('',(10.6942336092596,-2.79024989380572,-3.5));
#55795=CARTESIAN_POINT('Origin',(10.995,-0.509999999999999,-3.5));
#55796=CARTESIAN_POINT('',(10.9824030018659,-2.93240300186586,-3.5));
#55797=CARTESIAN_POINT('Origin',(10.6288496112726,-3.28595639245914,-3.5));
#55798=CARTESIAN_POINT('',(11.3535533905933,-3.30355339059329,-3.5));
#55799=CARTESIAN_POINT('',(10.9824030018659,-2.93240300186586,-3.5));
#55800=CARTESIAN_POINT('',(11.5,-3.65710678118656,-3.5));
#55801=CARTESIAN_POINT('Origin',(11.,-3.65710678118656,-3.5));
#55802=CARTESIAN_POINT('',(11.5,-4.54289321881346,-3.5));
#55803=CARTESIAN_POINT('',(11.5,-3.65710678118656,-3.5));
#55804=CARTESIAN_POINT('',(11.3535533905933,-4.89644660940673,-3.5));
#55805=CARTESIAN_POINT('Origin',(11.,-4.54289321881346,-3.5));
#55806=CARTESIAN_POINT('',(10.9824030018659,-5.26759699813413,-3.5));
#55807=CARTESIAN_POINT('',(11.3535533905933,-4.89644660940673,-3.5));
#55808=CARTESIAN_POINT('',(10.6942336092596,-5.40975010619428,-3.5));
#55809=CARTESIAN_POINT('Origin',(10.6288496112726,-4.91404360754086,-3.5));
#55810=CARTESIAN_POINT('',(8.71475010619428,-7.38923360925963,-3.5));
#55811=CARTESIAN_POINT('Origin',(10.995,-7.69,-3.5));
#55812=CARTESIAN_POINT('',(8.57259699813413,-7.67740300186587,-3.5));
#55813=CARTESIAN_POINT('Origin',(8.21904360754086,-7.32384961127259,-3.5));
#55814=CARTESIAN_POINT('',(8.19644660940673,-8.05355339059327,-3.5));
#55815=CARTESIAN_POINT('',(8.57259699813413,-7.67740300186587,-3.5));
#55816=CARTESIAN_POINT('',(8.05,-8.40710678118654,-3.5));
#55817=CARTESIAN_POINT('Origin',(8.55,-8.40710678118654,-3.5));
#55818=CARTESIAN_POINT('',(8.05,-12.0328932188134,-3.5));
#55819=CARTESIAN_POINT('',(8.05,-8.40710678118654,-3.5));
#55820=CARTESIAN_POINT('',(8.19644660940673,-12.3864466094067,-3.5));
#55821=CARTESIAN_POINT('Origin',(8.55,-12.0328932188134,-3.5));
#55822=CARTESIAN_POINT('',(12.31,-16.5,-3.5));
#55823=CARTESIAN_POINT('',(8.19644660940673,-12.3864466094067,-3.5));
#55824=CARTESIAN_POINT('',(12.31,-16.5,-3.5));
#55825=CARTESIAN_POINT('Origin',(0.,0.,-71.4));
#55826=CARTESIAN_POINT('',(22.2,-16.5,-71.4));
#55827=CARTESIAN_POINT('',(22.2,-16.5,-71.4));
#55828=CARTESIAN_POINT('',(23.2,-15.5,-71.4));
#55829=CARTESIAN_POINT('',(23.2,-15.5,-71.4));
#55830=CARTESIAN_POINT('',(23.2,12.,-71.4));
#55831=CARTESIAN_POINT('',(23.2,12.,-71.4));
#55832=CARTESIAN_POINT('',(22.2,13.,-71.4));
#55833=CARTESIAN_POINT('',(22.2,13.,-71.4));
#55834=CARTESIAN_POINT('',(5.79999999999999,13.,-71.4));
#55835=CARTESIAN_POINT('',(-22.2,13.,-71.4));
#55836=CARTESIAN_POINT('',(4.99999999999997,13.8,-71.4));
#55837=CARTESIAN_POINT('',(4.99999999999996,13.8,-71.4));
#55838=CARTESIAN_POINT('',(-4.99999999999998,13.8,-71.4));
#55839=CARTESIAN_POINT('',(-5.79999999999999,13.8,-71.4));
#55840=CARTESIAN_POINT('',(-5.79999999999999,13.,-71.4));
#55841=CARTESIAN_POINT('',(-4.99999999999997,13.8,-71.4));
#55842=CARTESIAN_POINT('',(-22.2,13.,-71.4));
#55843=CARTESIAN_POINT('',(-22.2,13.,-71.4));
#55844=CARTESIAN_POINT('',(-23.2,12.,-71.4));
#55845=CARTESIAN_POINT('',(-23.2,12.,-71.4));
#55846=CARTESIAN_POINT('',(-23.2,-15.5,-71.4));
#55847=CARTESIAN_POINT('',(-23.2,-15.5,-71.4));
#55848=CARTESIAN_POINT('',(-22.2,-16.5,-71.4));
#55849=CARTESIAN_POINT('',(-22.2,-16.5,-71.4));
#55850=CARTESIAN_POINT('',(-23.,-16.5,-71.4));
#55851=CARTESIAN_POINT('Origin',(-4.99999999999996,13.8,1.31418445149757E-15));
#55852=CARTESIAN_POINT('',(-5.79999999999999,13.,-81.3));
#55853=CARTESIAN_POINT('',(-4.99999999999999,13.8,-81.3));
#55854=CARTESIAN_POINT('',(-4.99999999999997,13.8,-81.3));
#55855=CARTESIAN_POINT('',(-5.8,13.,-81.3));
#55856=CARTESIAN_POINT('',(-4.99999999999998,13.8,-71.4));
#55857=CARTESIAN_POINT('Origin',(22.2,13.,-84.8));
#55858=CARTESIAN_POINT('',(23.2,12.,-81.3));
#55859=CARTESIAN_POINT('',(22.2,13.,-81.3));
#55860=CARTESIAN_POINT('',(23.2,12.,-81.3));
#55861=CARTESIAN_POINT('',(22.2,13.,-84.8));
#55862=CARTESIAN_POINT('',(23.2,12.,-84.8));
#55863=CARTESIAN_POINT('Origin',(23.2,12.,-84.8));
#55864=CARTESIAN_POINT('',(23.2,-15.5,-81.3));
#55865=CARTESIAN_POINT('',(23.2,-15.5,-81.3));
#55866=CARTESIAN_POINT('',(23.2,-15.5,-84.8));
#55867=CARTESIAN_POINT('Origin',(23.2,-15.5,-84.8));
#55868=CARTESIAN_POINT('',(22.2,-16.5,-81.3));
#55869=CARTESIAN_POINT('',(22.2,-16.5,-81.3));
#55870=CARTESIAN_POINT('',(22.2,-16.5,-84.8));
#55871=CARTESIAN_POINT('Origin',(-22.2,13.,-84.8));
#55872=CARTESIAN_POINT('',(5.8,13.,-81.3));
#55873=CARTESIAN_POINT('',(22.2,13.,-81.3));
#55874=CARTESIAN_POINT('',(5.8,13.,-81.3));
#55875=CARTESIAN_POINT('Origin',(8.55,-12.0328932188134,-84.8));
#55876=CARTESIAN_POINT('',(8.05,-12.0328932188134,-81.3));
#55877=CARTESIAN_POINT('',(8.05,-12.0328932188134,-84.8));
#55878=CARTESIAN_POINT('',(8.19644660940673,-12.3864466094067,-81.3));
#55879=CARTESIAN_POINT('Origin',(8.55,-12.0328932188134,-81.3));
#55880=CARTESIAN_POINT('',(8.19644660940673,-12.3864466094067,-84.8));
#55881=CARTESIAN_POINT('Origin',(8.55,-8.40710678118654,-84.8));
#55882=CARTESIAN_POINT('',(8.19644660940673,-8.05355339059327,-81.3));
#55883=CARTESIAN_POINT('',(8.19644660940673,-8.05355339059327,-84.8));
#55884=CARTESIAN_POINT('',(8.05,-8.40710678118654,-81.3));
#55885=CARTESIAN_POINT('Origin',(8.55,-8.40710678118654,-81.3));
#55886=CARTESIAN_POINT('',(8.05,-8.40710678118654,-84.8));
#55887=CARTESIAN_POINT('Origin',(8.05,-12.24,-84.8));
#55888=CARTESIAN_POINT('',(8.05,-8.40710678118654,-81.3));
#55889=CARTESIAN_POINT('Origin',(12.31,-16.5,-84.8));
#55890=CARTESIAN_POINT('',(12.31,-16.5,-81.3));
#55891=CARTESIAN_POINT('',(8.19644660940673,-12.3864466094067,-81.3));
#55892=CARTESIAN_POINT('',(12.31,-16.5,-84.8));
#55893=CARTESIAN_POINT('Origin',(12.31,-16.5,-84.8));
#55894=CARTESIAN_POINT('',(12.31,-16.5,-81.3));
#55895=CARTESIAN_POINT('Origin',(8.21904360754086,-7.32384961127259,-84.8));
#55896=CARTESIAN_POINT('',(8.71475010619428,-7.38923360925963,-81.3));
#55897=CARTESIAN_POINT('',(8.57259699813413,-7.67740300186587,-81.3));
#55898=CARTESIAN_POINT('Origin',(8.21904360754086,-7.32384961127259,-81.3));
#55899=CARTESIAN_POINT('',(8.57259699813413,-7.67740300186587,-84.8));
#55900=CARTESIAN_POINT('',(8.71475010619428,-7.38923360925963,-84.8));
#55901=CARTESIAN_POINT('Origin',(10.6288496112726,-4.91404360754086,-84.8));
#55902=CARTESIAN_POINT('',(10.9824030018659,-5.26759699813413,-81.3));
#55903=CARTESIAN_POINT('',(10.6942336092596,-5.40975010619428,-81.3));
#55904=CARTESIAN_POINT('Origin',(10.6288496112726,-4.91404360754086,-81.3));
#55905=CARTESIAN_POINT('',(10.6942336092596,-5.40975010619428,-84.8));
#55906=CARTESIAN_POINT('',(10.9824030018659,-5.26759699813413,0.));
#55907=CARTESIAN_POINT('Origin',(10.995,-7.69,-84.8));
#55908=CARTESIAN_POINT('Origin',(10.995,-7.69,-81.3));
#55909=CARTESIAN_POINT('Origin',(11.,-4.54289321881346,-84.8));
#55910=CARTESIAN_POINT('',(11.5,-4.54289321881346,-81.3));
#55911=CARTESIAN_POINT('',(11.3535533905933,-4.89644660940673,-81.3));
#55912=CARTESIAN_POINT('Origin',(11.,-4.54289321881346,-81.3));
#55913=CARTESIAN_POINT('',(11.3535533905933,-4.89644660940673,-84.8));
#55914=CARTESIAN_POINT('',(11.5,-4.54289321881346,0.));
#55915=CARTESIAN_POINT('Origin',(11.,-3.65710678118656,-84.8));
#55916=CARTESIAN_POINT('',(11.3535533905933,-3.30355339059329,-81.3));
#55917=CARTESIAN_POINT('',(11.5,-3.65710678118656,-81.3));
#55918=CARTESIAN_POINT('Origin',(11.,-3.65710678118656,-81.3));
#55919=CARTESIAN_POINT('',(11.5,-3.65710678118656,-84.8));
#55920=CARTESIAN_POINT('',(11.3535533905933,-3.30355339059329,0.));
#55921=CARTESIAN_POINT('Origin',(11.5,-4.75000000000001,-84.8));
#55922=CARTESIAN_POINT('',(11.5,-3.65710678118656,-81.3));
#55923=CARTESIAN_POINT('Origin',(8.05,-8.2,-84.8));
#55924=CARTESIAN_POINT('',(11.3535533905933,-4.89644660940673,-81.3));
#55925=CARTESIAN_POINT('Origin',(10.6288496112726,-3.28595639245914,-84.8));
#55926=CARTESIAN_POINT('',(10.6942336092596,-2.79024989380572,-81.3));
#55927=CARTESIAN_POINT('',(10.9824030018659,-2.93240300186586,-81.3));
#55928=CARTESIAN_POINT('Origin',(10.6288496112726,-3.28595639245914,-81.3));
#55929=CARTESIAN_POINT('',(10.9824030018659,-2.93240300186586,-84.8));
#55930=CARTESIAN_POINT('',(10.6942336092596,-2.79024989380572,-84.8));
#55931=CARTESIAN_POINT('Origin',(8.21904360754086,-0.876150388727407,-84.8));
#55932=CARTESIAN_POINT('',(8.57259699813413,-0.522596998134133,-81.3));
#55933=CARTESIAN_POINT('',(8.71475010619428,-0.81076639074037,-81.3));
#55934=CARTESIAN_POINT('Origin',(8.21904360754086,-0.876150388727407,-81.3));
#55935=CARTESIAN_POINT('',(8.71475010619428,-0.81076639074037,-84.8));
#55936=CARTESIAN_POINT('',(8.57259699813413,-0.522596998134133,0.));
#55937=CARTESIAN_POINT('Origin',(10.995,-0.509999999999999,-84.8));
#55938=CARTESIAN_POINT('Origin',(10.995,-0.509999999999999,-81.3));
#55939=CARTESIAN_POINT('Origin',(8.05,3.67394039744206E-16,-84.8));
#55940=CARTESIAN_POINT('',(-8.05,-1.60428730688303E-15,-81.3));
#55941=CARTESIAN_POINT('',(-8.05,-1.60428730688303E-15,-84.8));
#55942=CARTESIAN_POINT('',(8.05,3.67394039744206E-16,-81.3));
#55943=CARTESIAN_POINT('',(-8.05,-1.60428730688303E-15,-81.3));
#55944=CARTESIAN_POINT('',(8.05,3.67394039744206E-16,-84.8));
#55945=CARTESIAN_POINT('Origin',(8.05,3.67394039744206E-16,-84.8));
#55946=CARTESIAN_POINT('',(8.05,3.67394039744206E-16,-81.3));
#55947=CARTESIAN_POINT('Origin',(-8.21904360754086,-0.87615038872741,-84.8));
#55948=CARTESIAN_POINT('',(-8.71475010619428,-0.810766390740372,-81.3));
#55949=CARTESIAN_POINT('',(-8.57259699813413,-0.522596998134137,-81.3));
#55950=CARTESIAN_POINT('Origin',(-8.21904360754086,-0.87615038872741,-81.3));
#55951=CARTESIAN_POINT('',(-8.57259699813413,-0.522596998134137,-84.8));
#55952=CARTESIAN_POINT('',(-8.71475010619428,-0.810766390740372,-84.8));
#55953=CARTESIAN_POINT('Origin',(-10.6288496112726,-3.28595639245914,-84.8));
#55954=CARTESIAN_POINT('',(-10.9824030018659,-2.93240300186587,-81.3));
#55955=CARTESIAN_POINT('',(-10.6942336092596,-2.79024989380572,-81.3));
#55956=CARTESIAN_POINT('Origin',(-10.6288496112726,-3.28595639245914,-81.3));
#55957=CARTESIAN_POINT('',(-10.6942336092596,-2.79024989380572,-84.8));
#55958=CARTESIAN_POINT('',(-10.9824030018659,-2.93240300186587,0.));
#55959=CARTESIAN_POINT('Origin',(-10.995,-0.510000000000002,-84.8));
#55960=CARTESIAN_POINT('Origin',(-10.995,-0.510000000000002,-81.3));
#55961=CARTESIAN_POINT('Origin',(-11.,-3.65710678118656,-84.8));
#55962=CARTESIAN_POINT('',(-11.5,-3.65710678118656,-81.3));
#55963=CARTESIAN_POINT('',(-11.3535533905933,-3.30355339059329,-81.3));
#55964=CARTESIAN_POINT('Origin',(-11.,-3.65710678118656,-81.3));
#55965=CARTESIAN_POINT('',(-11.3535533905933,-3.30355339059329,-84.8));
#55966=CARTESIAN_POINT('',(-11.5,-3.65710678118656,0.));
#55967=CARTESIAN_POINT('Origin',(-11.,-4.54289321881346,-84.8));
#55968=CARTESIAN_POINT('',(-11.3535533905933,-4.89644660940674,-81.3));
#55969=CARTESIAN_POINT('',(-11.5,-4.54289321881346,-81.3));
#55970=CARTESIAN_POINT('Origin',(-11.,-4.54289321881346,-81.3));
#55971=CARTESIAN_POINT('',(-11.5,-4.54289321881346,-84.8));
#55972=CARTESIAN_POINT('',(-11.3535533905933,-4.89644660940674,0.));
#55973=CARTESIAN_POINT('Origin',(-11.5,-4.75000000000001,-84.8));
#55974=CARTESIAN_POINT('',(-11.5,-4.54289321881346,-81.3));
#55975=CARTESIAN_POINT('Origin',(-8.05,-1.60428730688303E-15,-84.8));
#55976=CARTESIAN_POINT('',(-11.3535533905933,-3.30355339059329,-81.3));
#55977=CARTESIAN_POINT('Origin',(-8.05,-1.60428730688303E-15,-84.8));
#55978=CARTESIAN_POINT('',(-8.57259699813413,-0.522596998134137,-81.3));
#55979=CARTESIAN_POINT('Origin',(-10.6288496112726,-4.91404360754086,-84.8));
#55980=CARTESIAN_POINT('',(-10.6942336092596,-5.40975010619428,-81.3));
#55981=CARTESIAN_POINT('',(-10.9824030018659,-5.26759699813413,-81.3));
#55982=CARTESIAN_POINT('Origin',(-10.6288496112726,-4.91404360754086,-81.3));
#55983=CARTESIAN_POINT('',(-10.9824030018659,-5.26759699813413,-84.8));
#55984=CARTESIAN_POINT('',(-10.6942336092596,-5.40975010619428,-84.8));
#55985=CARTESIAN_POINT('Origin',(-8.21904360754086,-7.32384961127259,-84.8));
#55986=CARTESIAN_POINT('',(-8.57259699813413,-7.67740300186587,-81.3));
#55987=CARTESIAN_POINT('',(-8.71475010619428,-7.38923360925963,-81.3));
#55988=CARTESIAN_POINT('Origin',(-8.21904360754086,-7.32384961127259,-81.3));
#55989=CARTESIAN_POINT('',(-8.71475010619428,-7.38923360925963,-84.8));
#55990=CARTESIAN_POINT('',(-8.57259699813413,-7.67740300186587,0.));
#55991=CARTESIAN_POINT('Origin',(-10.995,-7.69,-84.8));
#55992=CARTESIAN_POINT('Origin',(-10.995,-7.69,-81.3));
#55993=CARTESIAN_POINT('Origin',(-8.55,-8.40710678118654,-84.8));
#55994=CARTESIAN_POINT('',(-8.05,-8.40710678118654,-81.3));
#55995=CARTESIAN_POINT('',(-8.05,-8.40710678118654,-84.8));
#55996=CARTESIAN_POINT('',(-8.19644660940673,-8.05355339059327,-81.3));
#55997=CARTESIAN_POINT('Origin',(-8.55,-8.40710678118654,-81.3));
#55998=CARTESIAN_POINT('',(-8.19644660940673,-8.05355339059327,-84.8));
#55999=CARTESIAN_POINT('Origin',(-8.55,-12.0328932188134,-84.8));
#56000=CARTESIAN_POINT('',(-8.19644660940672,-12.3864466094067,-81.3));
#56001=CARTESIAN_POINT('',(-8.19644660940672,-12.3864466094067,-84.8));
#56002=CARTESIAN_POINT('',(-8.05,-12.0328932188134,-81.3));
#56003=CARTESIAN_POINT('Origin',(-8.55,-12.0328932188134,-81.3));
#56004=CARTESIAN_POINT('',(-8.05,-12.0328932188134,-84.8));
#56005=CARTESIAN_POINT('Origin',(-22.2,-16.5,-84.8));
#56006=CARTESIAN_POINT('',(-23.2,-15.5,-81.3));
#56007=CARTESIAN_POINT('',(-22.2,-16.5,-81.3));
#56008=CARTESIAN_POINT('',(-23.2,-15.5,-81.3));
#56009=CARTESIAN_POINT('',(-22.2,-16.5,-84.8));
#56010=CARTESIAN_POINT('',(-23.2,-15.5,-84.8));
#56011=CARTESIAN_POINT('Origin',(-23.2,-15.5,-84.8));
#56012=CARTESIAN_POINT('',(-23.2,12.,-81.3));
#56013=CARTESIAN_POINT('',(-23.2,12.,-81.3));
#56014=CARTESIAN_POINT('',(-23.2,12.,-84.8));
#56015=CARTESIAN_POINT('Origin',(-23.2,12.,-84.8));
#56016=CARTESIAN_POINT('',(-22.2,13.,-81.3));
#56017=CARTESIAN_POINT('',(-22.2,13.,-81.3));
#56018=CARTESIAN_POINT('',(-22.2,13.,-84.8));
#56019=CARTESIAN_POINT('Origin',(-22.2,13.,-84.8));
#56020=CARTESIAN_POINT('',(22.2,13.,-81.3));
#56021=CARTESIAN_POINT('Origin',(-23.,-16.5,-84.8));
#56022=CARTESIAN_POINT('',(-12.31,-16.5,-81.3));
#56023=CARTESIAN_POINT('',(-22.2,-16.5,-81.3));
#56024=CARTESIAN_POINT('',(-12.31,-16.5,-84.8));
#56025=CARTESIAN_POINT('Origin',(-12.31,-16.5,-84.8));
#56026=CARTESIAN_POINT('',(-12.31,-16.5,-81.3));
#56027=CARTESIAN_POINT('Origin',(-8.05,-12.24,-84.8));
#56028=CARTESIAN_POINT('',(-8.05,-12.0328932188134,-81.3));
#56029=CARTESIAN_POINT('Origin',(-8.05,-8.2,-84.8));
#56030=CARTESIAN_POINT('',(-8.19644660940673,-8.05355339059327,-81.3));
#56031=CARTESIAN_POINT('Origin',(-8.05,-8.2,-84.8));
#56032=CARTESIAN_POINT('',(-10.9824030018659,-5.26759699813413,-81.3));
#56033=CARTESIAN_POINT('Origin',(8.05,3.67394039744206E-16,-84.8));
#56034=CARTESIAN_POINT('',(10.9824030018659,-2.93240300186586,-81.3));
#56035=CARTESIAN_POINT('Origin',(8.05,-8.2,-84.8));
#56036=CARTESIAN_POINT('',(8.57259699813413,-7.67740300186587,-81.3));
#56037=CARTESIAN_POINT('Origin',(4.99999999999995,13.8,1.31418445149758E-15));
#56038=CARTESIAN_POINT('',(4.99999999999997,13.8,-81.3));
#56039=CARTESIAN_POINT('',(4.99999999999996,13.8,-81.3));
#56040=CARTESIAN_POINT('',(4.99999999999997,13.8,-81.3));
#56041=CARTESIAN_POINT('Origin',(-1.64657055886728E-14,13.8,4.08782152511659E-30));
#56042=CARTESIAN_POINT('',(-5.8,13.8,-81.3));
#56043=CARTESIAN_POINT('Origin',(-5.8,13.8,-81.3));
#56044=CARTESIAN_POINT('Origin',(4.99995,13.,-1.));
#56045=CARTESIAN_POINT('',(4.99995,8.,-1.));
#56046=CARTESIAN_POINT('',(4.99995,13.,-1.));
#56047=CARTESIAN_POINT('',(4.99995,8.,-1.));
#56048=CARTESIAN_POINT('Origin',(0.,8.,-1.));
#56049=CARTESIAN_POINT('',(-4.99995,8.,-1.));
#56050=CARTESIAN_POINT('Origin',(0.,8.,-1.));
#56051=CARTESIAN_POINT('',(-4.99995,8.,-1.));
#56052=CARTESIAN_POINT('Origin',(-4.99995,13.,-1.));
#56053=CARTESIAN_POINT('',(-4.99995,13.,-1.));
#56054=CARTESIAN_POINT('Origin',(0.,8.,-1.));
#56055=CARTESIAN_POINT('Origin',(-28.5,24.2065391822594,-19.9));
#56056=CARTESIAN_POINT('Origin',(-28.5,24.2065391822594,-64.9));
#56057=CARTESIAN_POINT('Origin',(28.5,24.2065391822594,-19.9));
#56058=CARTESIAN_POINT('Origin',(28.5,24.2065391822594,-64.9));
#56059=CARTESIAN_POINT('',(0.,0.,0.));
#56060=CARTESIAN_POINT('Origin',(-1.30104260698261E-15,5.62313017679403,
-9.43017678221748));
#56061=CARTESIAN_POINT('',(-9.42566476249075E-16,6.10854241414471,-5.90647463868609));
#56062=CARTESIAN_POINT('Origin',(-1.30104260698261E-15,4.79163859753386,
-9.0857616930889));
#56063=CARTESIAN_POINT('',(-1.65091236461116E-15,7.42947410803995,-6.70023456114395));
#56064=CARTESIAN_POINT('Origin',(-1.82151749662023E-15,7.24953476434565,
-5.50368876904451));
#56065=CARTESIAN_POINT('Origin',(-1.1944312217556E-15,6.1997608355023,-9.66902502153458));
#56066=CARTESIAN_POINT('Ctrl Pts',(-1.0334492107102E-15,9.1104629285565,
-7.23378761718564));
#56067=CARTESIAN_POINT('Ctrl Pts',(-3.36374346224613,9.1104629285565,-7.23378761718564));
#56068=CARTESIAN_POINT('Ctrl Pts',(-3.36374346224613,7.82321403482853,-10.3414813545735));
#56069=CARTESIAN_POINT('Ctrl Pts',(-3.36374346224613,6.53596514110056,-13.4491750919613));
#56070=CARTESIAN_POINT('Ctrl Pts',(-1.0334492107102E-15,6.53596514110056,
-13.4491750919613));
#56071=CARTESIAN_POINT('Ctrl Pts',(3.36374346224612,6.53596514110056,-13.4491750919613));
#56072=CARTESIAN_POINT('Ctrl Pts',(3.36374346224612,7.82321403482853,-10.3414813545735));
#56073=CARTESIAN_POINT('Ctrl Pts',(3.36374346224612,9.1104629285565,-7.23378761718564));
#56074=CARTESIAN_POINT('Ctrl Pts',(-1.0334492107102E-15,9.1104629285565,
-7.23378761718564));
#56075=CARTESIAN_POINT('Ctrl Pts',(-1.09748950322703E-15,8.40101827381132,
-6.55413148618164));
#56076=CARTESIAN_POINT('Ctrl Pts',(-3.72017113527558,8.40101827381132,-6.55413148618164));
#56077=CARTESIAN_POINT('Ctrl Pts',(-3.72017113527558,6.97737041477854,-9.99112145550203));
#56078=CARTESIAN_POINT('Ctrl Pts',(-3.72017113527558,5.55372255574576,-13.4281114248224));
#56079=CARTESIAN_POINT('Ctrl Pts',(-1.09748950322703E-15,5.55372255574576,
-13.4281114248224));
#56080=CARTESIAN_POINT('Ctrl Pts',(3.72017113527558,5.55372255574576,-13.4281114248224));
#56081=CARTESIAN_POINT('Ctrl Pts',(3.72017113527558,6.97737041477854,-9.99112145550203));
#56082=CARTESIAN_POINT('Ctrl Pts',(3.72017113527558,8.40101827381132,-6.55413148618164));
#56083=CARTESIAN_POINT('Ctrl Pts',(-1.09748950322703E-15,8.40101827381132,
-6.55413148618164));
#56084=CARTESIAN_POINT('Ctrl Pts',(-1.15636367776747E-15,7.42947410803995,
-6.70023456114395));
#56085=CARTESIAN_POINT('Ctrl Pts',(-3.21339563862928,7.42947410803995,-6.70023456114395));
#56086=CARTESIAN_POINT('Ctrl Pts',(-3.21339563862928,6.1997608355023,-9.66902502153458));
#56087=CARTESIAN_POINT('Ctrl Pts',(-3.21339563862928,4.97004756296464,-12.6378154819252));
#56088=CARTESIAN_POINT('Ctrl Pts',(-1.15636367776747E-15,4.97004756296464,
-12.6378154819252));
#56089=CARTESIAN_POINT('Ctrl Pts',(3.21339563862928,4.97004756296464,-12.6378154819252));
#56090=CARTESIAN_POINT('Ctrl Pts',(3.21339563862928,6.1997608355023,-9.66902502153458));
#56091=CARTESIAN_POINT('Ctrl Pts',(3.21339563862928,7.42947410803995,-6.70023456114395));
#56092=CARTESIAN_POINT('Ctrl Pts',(-1.15636367776747E-15,7.42947410803995,
-6.70023456114395));
#56093=CARTESIAN_POINT('',(-1.44538897712945E-15,9.1104629285565,-7.23378761718564));
#56094=CARTESIAN_POINT('Origin',(-1.26789919235761E-15,7.72689451084046,
-8.67799620097772));
#56095=CARTESIAN_POINT('Origin',(-1.07151675469833E-15,7.82321403482853,
-10.3414813545735));
#56096=CARTESIAN_POINT('Origin',(-9.16325707068394E-16,9.87297602634596,
-11.1905205710969));
#56097=CARTESIAN_POINT('',(-1.22248740685523E-15,10.8296846072587,-8.88082173981866));
#56098=CARTESIAN_POINT('',(-1.22248740685523E-15,10.8296846072587,-8.88082173981866));
#56099=CARTESIAN_POINT('Origin',(-9.16325707068394E-16,9.87297602634596,
-11.1905205710969));
#56100=CARTESIAN_POINT('Origin',(-8.67361737988404E-16,9.41103626009031,
-10.9991788549143));
#56101=CARTESIAN_POINT('',(0.944722181384557,9.66424685661039,-11.6944373635354));
#56102=CARTESIAN_POINT('Origin',(-9.16325707068394E-16,9.87297602634596,
-11.1905205710969));
#56103=CARTESIAN_POINT('Origin',(0.,4.50578927537974,-8.96735902705751));
#56104=CARTESIAN_POINT('',(-1.73205080756888,3.64358830043861,-11.8574002906228));
#56105=CARTESIAN_POINT('',(1.73205080756888,3.64358830043861,-11.8574002906228));
#56106=CARTESIAN_POINT('Origin',(0.,4.79163859753386,-9.08576169308891));
#56107=CARTESIAN_POINT('',(-8.67361737988404E-16,2.97505554591939,-12.6628771571027));
#56108=CARTESIAN_POINT('Ctrl Pts',(-8.83559534733916E-12,2.97505554591472,
-12.6628771571063));
#56109=CARTESIAN_POINT('Ctrl Pts',(0.928203230271955,3.46598430139072,-12.2861742738559));
#56110=CARTESIAN_POINT('Ctrl Pts',(1.73205080756887,3.6435883004386,-11.8574002906228));
#56111=CARTESIAN_POINT('Ctrl Pts',(-1.73205080756888,3.64358830043861,-11.8574002906228));
#56112=CARTESIAN_POINT('Ctrl Pts',(-0.928203230271849,3.46598430139071,
-12.2861742738559));
#56113=CARTESIAN_POINT('Ctrl Pts',(9.11080614203771E-12,2.97505554591457,
-12.6628771571064));
#56114=CARTESIAN_POINT('Origin',(0.,2.94387953251129,-8.32039482835873));
#56115=CARTESIAN_POINT('',(-1.73205080756888,4.09192982960656,-5.54875623082487));
#56116=CARTESIAN_POINT('',(1.73205080756888,4.09192982960656,-5.54875623082487));
#56117=CARTESIAN_POINT('Origin',(0.,2.94387953251129,-8.32039482835873));
#56118=CARTESIAN_POINT('',(6.50521303491303E-15,4.76046258412578,-4.74327936434497));
#56119=CARTESIAN_POINT('Ctrl Pts',(-8.84140945978337E-12,4.76046258413045,
-4.74327936434139));
#56120=CARTESIAN_POINT('Ctrl Pts',(0.928203230271958,4.26953382865444,-5.11998224759177));
#56121=CARTESIAN_POINT('Ctrl Pts',(1.73205080756888,4.09192982960656,-5.54875623082487));
#56122=CARTESIAN_POINT('Ctrl Pts',(-1.73205080756888,4.09192982960655,-5.54875623082487));
#56123=CARTESIAN_POINT('Ctrl Pts',(-0.928203230271845,4.26953382865446,
-5.11998224759171));
#56124=CARTESIAN_POINT('Ctrl Pts',(9.11907870314464E-12,4.7604625841306,
-4.74327936434127));
#56125=CARTESIAN_POINT('Origin',(0.,0.,-7.101));
#56126=CARTESIAN_POINT('',(-2.79266716119615,2.86374058300968,-7.101));
#56127=CARTESIAN_POINT('',(2.79266716119615,2.86374058300968,-7.101));
#56128=CARTESIAN_POINT('Origin',(0.,2.44435548440748,-8.11348519290263));
#56129=CARTESIAN_POINT('',(-4.61252776028392E-16,4.,-5.51067764861519));
#56130=CARTESIAN_POINT('Ctrl Pts',(-2.79266716119614,2.86374058300969,-7.10099999999999));
#56131=CARTESIAN_POINT('Ctrl Pts',(-2.791487395233,2.86489106908469,-7.0982224809144));
#56132=CARTESIAN_POINT('Ctrl Pts',(-2.79030270745925,2.86604495955758,-7.09544824938184));
#56133=CARTESIAN_POINT('Ctrl Pts',(-2.64444489381139,3.00792702197672,-6.75569806071638));
#56134=CARTESIAN_POINT('Ctrl Pts',(-2.42146694806281,3.19843151589414,-6.46722664985982));
#56135=CARTESIAN_POINT('Ctrl Pts',(-1.897815678339,3.53535819041829,-6.01625804314877));
#56136=CARTESIAN_POINT('Ctrl Pts',(-1.5580225174343,3.70511768616704,-5.82557882438308));
#56137=CARTESIAN_POINT('Ctrl Pts',(-0.804950314595278,3.93794187104499,
-5.57277579859251));
#56138=CARTESIAN_POINT('Ctrl Pts',(-0.391351836138015,4.,-5.51067764861519));
#56139=CARTESIAN_POINT('Ctrl Pts',(-3.46944695195361E-16,4.,-5.51067764861519));
#56140=CARTESIAN_POINT('',(-3.67394039744206E-16,4.09192982960655,-5.54875623082487));
#56141=CARTESIAN_POINT('',(-3.67394039744206E-16,1.14805029709526,-4.32936140246614));
#56142=CARTESIAN_POINT('Origin',(0.,2.94387953251129,-8.32039482835873));
#56143=CARTESIAN_POINT('Ctrl Pts',(-5.55111512312578E-16,4.,-5.51067764861519));
#56144=CARTESIAN_POINT('Ctrl Pts',(0.391351836138015,4.,-5.51067764861519));
#56145=CARTESIAN_POINT('Ctrl Pts',(0.804950314595278,3.93794187104499,-5.57277579859251));
#56146=CARTESIAN_POINT('Ctrl Pts',(1.5580225174343,3.70511768616704,-5.82557882438308));
#56147=CARTESIAN_POINT('Ctrl Pts',(1.897815678339,3.53535819041829,-6.01625804314877));
#56148=CARTESIAN_POINT('Ctrl Pts',(2.42146694806282,3.19843151589414,-6.46722664985983));
#56149=CARTESIAN_POINT('Ctrl Pts',(2.64444489381139,3.00792702197672,-6.75569806071639));
#56150=CARTESIAN_POINT('Ctrl Pts',(2.79030270745925,2.86604495955758,-7.09544824938184));
#56151=CARTESIAN_POINT('Ctrl Pts',(2.791487395233,2.86489106908469,-7.0982224809144));
#56152=CARTESIAN_POINT('Ctrl Pts',(2.79266716119614,2.86374058300969,-7.10099999999999));
#56153=CARTESIAN_POINT('Origin',(0.,0.,-13.5441803724939));
#56154=CARTESIAN_POINT('',(4.,-4.89858719658941E-16,-7.101));
#56155=CARTESIAN_POINT('Origin',(0.,0.,-7.101));
#56156=CARTESIAN_POINT('',(-4.,-4.89858719658941E-16,-7.101));
#56157=CARTESIAN_POINT('Origin',(0.,0.,-7.101));
#56158=CARTESIAN_POINT('Origin',(0.,0.,-7.101));
#56159=CARTESIAN_POINT('',(4.,4.20648087646404E-14,-3.));
#56160=CARTESIAN_POINT('',(4.,-4.89858719658941E-16,-13.5441803724939));
#56161=CARTESIAN_POINT('',(2.00000000000003,-3.46410161513774,-3.));
#56162=CARTESIAN_POINT('Origin',(0.,0.,-3.));
#56163=CARTESIAN_POINT('',(-1.99999999999998,-3.46410161513777,-3.));
#56164=CARTESIAN_POINT('Origin',(0.,0.,-3.));
#56165=CARTESIAN_POINT('',(-4.,-1.4271988688003E-14,-3.));
#56166=CARTESIAN_POINT('Origin',(0.,0.,-3.));
#56167=CARTESIAN_POINT('',(-2.,3.46410161513775,-3.));
#56168=CARTESIAN_POINT('Origin',(0.,0.,-3.));
#56169=CARTESIAN_POINT('',(1.99999999999999,3.46410161513778,-3.));
#56170=CARTESIAN_POINT('Origin',(0.,0.,-3.));
#56171=CARTESIAN_POINT('Origin',(0.,0.,-3.));
#56172=CARTESIAN_POINT('Origin',(0.,0.,-7.101));
#56173=CARTESIAN_POINT('',(-2.44929359829471E-16,-2.99951956532372E-32,
-11.101));
#56174=CARTESIAN_POINT('Origin',(0.,0.,-7.101));
#56175=CARTESIAN_POINT('Origin',(0.,6.32237232699421,-5.39024356304375));
#56176=CARTESIAN_POINT('',(3.46410161513776,4.79163859753387,-9.08576169308891));
#56177=CARTESIAN_POINT('Origin',(0.,4.79163859753387,-9.08576169308891));
#56178=CARTESIAN_POINT('',(-3.46410161513776,4.79163859753387,-9.08576169308891));
#56179=CARTESIAN_POINT('Origin',(0.,4.79163859753386,-9.08576169308891));
#56180=CARTESIAN_POINT('',(-1.73205080756888,5.93968889462913,-6.31412309555504));
#56181=CARTESIAN_POINT('Origin',(0.,4.79163859753386,-9.08576169308891));
#56182=CARTESIAN_POINT('',(1.73205080756888,5.93968889462913,-6.31412309555504));
#56183=CARTESIAN_POINT('Origin',(0.,4.79163859753386,-9.08576169308891));
#56184=CARTESIAN_POINT('Origin',(0.,4.79163859753386,-9.08576169308891));
#56185=CARTESIAN_POINT('Origin',(0.,4.47461326197163,-4.62487669831358));
#56186=CARTESIAN_POINT('',(3.46410161513776,2.94387953251129,-8.32039482835873));
#56187=CARTESIAN_POINT('Origin',(0.,2.94387953251129,-8.32039482835873));
#56188=CARTESIAN_POINT('',(-3.46410161513776,2.94387953251129,-8.32039482835873));
#56189=CARTESIAN_POINT('Origin',(0.,2.94387953251129,-8.32039482835873));
#56190=CARTESIAN_POINT('',(-1.73205080756888,1.79582923541603,-11.0920334258926));
#56191=CARTESIAN_POINT('Origin',(0.,2.94387953251129,-8.32039482835873));
#56192=CARTESIAN_POINT('',(1.73205080756888,1.79582923541603,-11.0920334258926));
#56193=CARTESIAN_POINT('Origin',(0.,2.94387953251129,-8.32039482835873));
#56194=CARTESIAN_POINT('Origin',(0.,2.94387953251129,-8.32039482835873));
#56195=CARTESIAN_POINT('Origin',(0.,0.,-3.));
#56196=CARTESIAN_POINT('',(-4.00000000000001,2.3094010767585,-3.));
#56197=CARTESIAN_POINT('',(-4.00000000000001,2.3094010767585,-3.));
#56198=CARTESIAN_POINT('',(0.,4.61880215351701,-3.));
#56199=CARTESIAN_POINT('Origin',(0.,0.,-3.));
#56200=CARTESIAN_POINT('',(0.,4.61880215351701,-3.));
#56201=CARTESIAN_POINT('',(0.,4.61880215351701,-3.));
#56202=CARTESIAN_POINT('',(3.99999999999998,2.30940107675855,-3.));
#56203=CARTESIAN_POINT('Origin',(0.,0.,-3.));
#56204=CARTESIAN_POINT('',(3.99999999999998,2.30940107675855,-3.));
#56205=CARTESIAN_POINT('',(3.99999999999998,2.30940107675855,-3.));
#56206=CARTESIAN_POINT('',(4.00000000000002,-2.30940107675847,-3.));
#56207=CARTESIAN_POINT('Origin',(0.,0.,-3.));
#56208=CARTESIAN_POINT('',(4.00000000000002,-2.30940107675847,-3.));
#56209=CARTESIAN_POINT('',(4.00000000000002,-2.30940107675847,-3.));
#56210=CARTESIAN_POINT('',(3.22529230536262E-14,-4.61880215351701,-3.));
#56211=CARTESIAN_POINT('Origin',(0.,0.,-3.));
#56212=CARTESIAN_POINT('',(3.22529230536262E-14,-4.61880215351701,-3.));
#56213=CARTESIAN_POINT('',(3.22529230536262E-14,-4.61880215351701,-3.));
#56214=CARTESIAN_POINT('',(-3.99999999999999,-2.30940107675852,-3.));
#56215=CARTESIAN_POINT('Origin',(0.,0.,-3.));
#56216=CARTESIAN_POINT('',(-3.99999999999999,-2.30940107675852,-3.));
#56217=CARTESIAN_POINT('',(-3.99999999999999,-2.30940107675852,-3.));
#56218=CARTESIAN_POINT('',(-4.00000000000001,2.3094010767585,-3.));
#56219=CARTESIAN_POINT('Origin',(3.99999999999998,2.30940107675855,-3.));
#56220=CARTESIAN_POINT('',(3.99999999999998,2.30940107675855,0.));
#56221=CARTESIAN_POINT('',(0.,4.61880215351701,0.));
#56222=CARTESIAN_POINT('',(3.99999999999998,2.30940107675855,0.));
#56223=CARTESIAN_POINT('',(3.99999999999998,2.30940107675855,-3.));
#56224=CARTESIAN_POINT('',(0.,4.61880215351701,-3.));
#56225=CARTESIAN_POINT('Origin',(4.00000000000002,-2.30940107675847,-3.));
#56226=CARTESIAN_POINT('',(4.00000000000002,-2.30940107675847,0.));
#56227=CARTESIAN_POINT('',(4.00000000000002,-2.30940107675847,0.));
#56228=CARTESIAN_POINT('',(4.00000000000002,-2.30940107675847,-3.));
#56229=CARTESIAN_POINT('Origin',(3.22529230536262E-14,-4.61880215351701,
-3.));
#56230=CARTESIAN_POINT('',(3.22529230536262E-14,-4.61880215351701,0.));
#56231=CARTESIAN_POINT('',(3.22529230536262E-14,-4.61880215351701,0.));
#56232=CARTESIAN_POINT('',(3.22529230536262E-14,-4.61880215351701,-3.));
#56233=CARTESIAN_POINT('Origin',(-3.99999999999999,-2.30940107675852,-3.));
#56234=CARTESIAN_POINT('',(-3.99999999999999,-2.30940107675852,0.));
#56235=CARTESIAN_POINT('',(-3.99999999999999,-2.30940107675852,0.));
#56236=CARTESIAN_POINT('',(-3.99999999999999,-2.30940107675852,-3.));
#56237=CARTESIAN_POINT('Origin',(-4.00000000000001,2.3094010767585,-3.));
#56238=CARTESIAN_POINT('',(-4.00000000000001,2.3094010767585,0.));
#56239=CARTESIAN_POINT('',(-4.00000000000001,2.3094010767585,0.));
#56240=CARTESIAN_POINT('',(-4.00000000000001,2.3094010767585,-3.));
#56241=CARTESIAN_POINT('Origin',(0.,4.61880215351701,-3.));
#56242=CARTESIAN_POINT('',(0.,4.61880215351701,0.));
#56243=CARTESIAN_POINT('Origin',(0.,0.,0.));
#56244=CARTESIAN_POINT('Origin',(0.,2.94387953251129,-8.32039482835873));
#56245=CARTESIAN_POINT('',(-3.46410161513776,3.9950957193956,-6.59103842936755));
#56246=CARTESIAN_POINT('Ctrl Pts',(-3.46410161513776,2.94387953251129,-8.32039482835873));
#56247=CARTESIAN_POINT('Ctrl Pts',(-3.46410161513776,3.29908753061063,-7.46284686188391));
#56248=CARTESIAN_POINT('Ctrl Pts',(-3.46410161513776,3.99509571941731,-6.59103842934036));
#56249=CARTESIAN_POINT('Ctrl Pts',(-3.46410161515884,3.99509571939744,-6.59103842938149));
#56250=CARTESIAN_POINT('Ctrl Pts',(-2.53589838487072,3.91432583055759,-5.97753021406059));
#56251=CARTESIAN_POINT('Ctrl Pts',(-1.73205080756888,4.09192982960655,-5.54875623082487));
#56252=CARTESIAN_POINT('Origin',(0.,2.94387953251129,-8.32039482835873));
#56253=CARTESIAN_POINT('',(-3.46410161513776,2.46436198993525,-10.2865565594127));
#56254=CARTESIAN_POINT('Ctrl Pts',(-1.73205080756888,1.79582923541603,-11.0920334258926));
#56255=CARTESIAN_POINT('Ctrl Pts',(-2.53589838486591,1.97343323446393,-10.6632594426594));
#56256=CARTESIAN_POINT('Ctrl Pts',(-3.46410161514687,2.46436198994007,-10.286556559409));
#56257=CARTESIAN_POINT('Ctrl Pts',(-3.46410161513776,2.46436198993072,-10.2865565594531));
#56258=CARTESIAN_POINT('Ctrl Pts',(-3.46410161513776,2.58867153441109,-9.17794279483566));
#56259=CARTESIAN_POINT('Ctrl Pts',(-3.46410161513776,2.94387953251129,-8.32039482835874));
#56260=CARTESIAN_POINT('Origin',(0.,2.94387953251129,-8.32039482835873));
#56261=CARTESIAN_POINT('',(3.90312782094782E-15,1.69899512520508,-12.1343156244353));
#56262=CARTESIAN_POINT('Ctrl Pts',(9.12142465330762E-12,1.69899512520587,
-12.1343156244413));
#56263=CARTESIAN_POINT('Ctrl Pts',(-0.928203230271842,1.61822523636812,
-11.5208074091258));
#56264=CARTESIAN_POINT('Ctrl Pts',(-1.73205080756888,1.79582923541603,-11.0920334258926));
#56265=CARTESIAN_POINT('Ctrl Pts',(1.73205080756888,1.79582923541603,-11.0920334258926));
#56266=CARTESIAN_POINT('Ctrl Pts',(0.928203230271956,1.61822523636815,-11.5208074091257));
#56267=CARTESIAN_POINT('Ctrl Pts',(-8.8435124366233E-12,1.69899512520584,
-12.1343156244411));
#56268=CARTESIAN_POINT('Origin',(0.,2.94387953251129,-8.32039482835873));
#56269=CARTESIAN_POINT('',(3.46410161513776,2.46436198993525,-10.2865565594127));
#56270=CARTESIAN_POINT('Ctrl Pts',(3.46410161514661,2.46436198993993,-10.2865565594091));
#56271=CARTESIAN_POINT('Ctrl Pts',(2.53589838486581,1.97343323446391,-10.6632594426595));
#56272=CARTESIAN_POINT('Ctrl Pts',(1.73205080756888,1.79582923541603,-11.0920334258926));
#56273=CARTESIAN_POINT('Ctrl Pts',(3.46410161513776,2.94387953251129,-8.32039482835873));
#56274=CARTESIAN_POINT('Ctrl Pts',(3.46410161513776,2.58867153441108,-9.17794279483565));
#56275=CARTESIAN_POINT('Ctrl Pts',(3.46410161513776,2.46436198993072,-10.2865565594531));
#56276=CARTESIAN_POINT('Origin',(0.,2.94387953251129,-8.32039482835873));
#56277=CARTESIAN_POINT('',(3.46410161513776,3.9950957193956,-6.59103842936756));
#56278=CARTESIAN_POINT('Ctrl Pts',(3.46410161513776,3.99509571941731,-6.59103842934036));
#56279=CARTESIAN_POINT('Ctrl Pts',(3.46410161513776,3.29908753061063,-7.46284686188391));
#56280=CARTESIAN_POINT('Ctrl Pts',(3.46410161513776,2.94387953251129,-8.32039482835873));
#56281=CARTESIAN_POINT('Ctrl Pts',(1.73205080756888,4.09192982960655,-5.54875623082487));
#56282=CARTESIAN_POINT('Ctrl Pts',(2.53589838487052,3.91432583055763,-5.97753021406048));
#56283=CARTESIAN_POINT('Ctrl Pts',(3.46410161515834,3.99509571939739,-6.59103842938115));
#56284=CARTESIAN_POINT('Origin',(0.,4.50578927537974,-8.96735902705751));
#56285=CARTESIAN_POINT('',(3.46410161513776,3.74042241064956,-10.8151180920801));
#56286=CARTESIAN_POINT('Ctrl Pts',(3.46410161513776,3.74042241062786,-10.8151180921073));
#56287=CARTESIAN_POINT('Ctrl Pts',(3.46410161513776,4.43643059943453,-9.94330965956373));
#56288=CARTESIAN_POINT('Ctrl Pts',(3.46410161513776,4.79163859753386,-9.08576169308893));
#56289=CARTESIAN_POINT('Ctrl Pts',(1.73205080756889,3.64358830043861,-11.8574002906228));
#56290=CARTESIAN_POINT('Ctrl Pts',(2.53589838487114,3.82119229948767,-11.4286263073868));
#56291=CARTESIAN_POINT('Ctrl Pts',(3.46410161515986,3.74042241064764,-10.8151180920655));
#56292=CARTESIAN_POINT('Origin',(0.,4.50578927537974,-8.96735902705751));
#56293=CARTESIAN_POINT('',(3.46410161513776,5.27115614010992,-7.11959996203494));
#56294=CARTESIAN_POINT('Ctrl Pts',(3.46410161514743,5.2711561401048,-7.11959996203886));
#56295=CARTESIAN_POINT('Ctrl Pts',(2.53589838486614,5.76208489558118,-6.74289707878832));
#56296=CARTESIAN_POINT('Ctrl Pts',(1.73205080756888,5.93968889462914,-6.31412309555504));
#56297=CARTESIAN_POINT('Ctrl Pts',(3.46410161513776,4.79163859753387,-9.08576169308891));
#56298=CARTESIAN_POINT('Ctrl Pts',(3.46410161513776,5.14684659563408,-8.22821372661199));
#56299=CARTESIAN_POINT('Ctrl Pts',(3.46410161513776,5.27115614011445,-7.11959996199452));
#56300=CARTESIAN_POINT('Origin',(0.,4.50578927537974,-8.96735902705751));
#56301=CARTESIAN_POINT('',(6.50521303491303E-15,6.03652300484009,-5.27184089701236));
#56302=CARTESIAN_POINT('Ctrl Pts',(9.66462909312592E-12,6.03652300483925,
-5.27184089700597));
#56303=CARTESIAN_POINT('Ctrl Pts',(-0.928203230271627,6.11729289367709,
-5.88534911232177));
#56304=CARTESIAN_POINT('Ctrl Pts',(-1.73205080756888,5.93968889462913,-6.31412309555505));
#56305=CARTESIAN_POINT('Ctrl Pts',(1.73205080756888,5.93968889462914,-6.31412309555504));
#56306=CARTESIAN_POINT('Ctrl Pts',(0.928203230271628,6.11729289367709,-5.88534911232177));
#56307=CARTESIAN_POINT('Ctrl Pts',(-9.6577405477995E-12,6.03652300483925,
-5.27184089700597));
#56308=CARTESIAN_POINT('Origin',(0.,4.50578927537974,-8.96735902705751));
#56309=CARTESIAN_POINT('',(-3.46410161513776,5.27115614010992,-7.11959996203493));
#56310=CARTESIAN_POINT('Ctrl Pts',(-3.46410161513776,5.27115614011445,-7.1195999619945));
#56311=CARTESIAN_POINT('Ctrl Pts',(-3.46410161513776,5.14684659563408,-8.22821372661199));
#56312=CARTESIAN_POINT('Ctrl Pts',(-3.46410161513776,4.79163859753387,-9.08576169308891));
#56313=CARTESIAN_POINT('Ctrl Pts',(-1.73205080756888,5.93968889462913,-6.31412309555505));
#56314=CARTESIAN_POINT('Ctrl Pts',(-2.53589838486613,5.76208489558118,-6.74289707878832));
#56315=CARTESIAN_POINT('Ctrl Pts',(-3.46410161514742,5.27115614010481,-7.11959996203885));
#56316=CARTESIAN_POINT('Origin',(0.,4.50578927537974,-8.96735902705751));
#56317=CARTESIAN_POINT('',(-3.46410161513776,3.74042241064957,-10.8151180920801));
#56318=CARTESIAN_POINT('Ctrl Pts',(-3.46410161515986,3.74042241064764,-10.8151180920655));
#56319=CARTESIAN_POINT('Ctrl Pts',(-2.53589838487113,3.82119229948767,-11.4286263073868));
#56320=CARTESIAN_POINT('Ctrl Pts',(-1.73205080756889,3.64358830043861,-11.8574002906228));
#56321=CARTESIAN_POINT('Ctrl Pts',(-3.46410161513776,4.79163859753387,-9.08576169308891));
#56322=CARTESIAN_POINT('Ctrl Pts',(-3.46410161513776,4.43643059943453,-9.94330965956373));
#56323=CARTESIAN_POINT('Ctrl Pts',(-3.46410161513776,3.74042241062786,-10.8151180921073));
#56324=CARTESIAN_POINT('Origin',(-8.67361737988404E-16,1.41314580305094,
-12.0159129584039));
#56325=CARTESIAN_POINT('',(-8.67361737988404E-16,1.41314580305094,-12.0159129584039));
#56326=CARTESIAN_POINT('',(-3.46410161513776,2.17851266778112,-10.1681538933813));
#56327=CARTESIAN_POINT('Origin',(-3.46410161513776,2.17851266778112,-10.1681538933813));
#56328=CARTESIAN_POINT('',(-3.46410161513776,3.70924639724147,-6.47263576333616));
#56329=CARTESIAN_POINT('Origin',(-3.46410161513776,3.70924639724147,-6.47263576333616));
#56330=CARTESIAN_POINT('',(7.02214595811131E-16,4.47461326197164,-4.62487669831358));
#56331=CARTESIAN_POINT('Origin',(7.02214595811131E-16,4.47461326197164,
-4.62487669831358));
#56332=CARTESIAN_POINT('',(3.46410161513776,3.70924639724147,-6.47263576333616));
#56333=CARTESIAN_POINT('Origin',(3.46410161513776,3.70924639724147,-6.47263576333616));
#56334=CARTESIAN_POINT('',(3.46410161513776,2.17851266778112,-10.1681538933813));
#56335=CARTESIAN_POINT('Origin',(3.46410161513776,2.17851266778112,-10.1681538933813));
#56336=CARTESIAN_POINT('Origin',(0.944722181384557,9.66424685661038,-11.6944373635354));
#56337=CARTESIAN_POINT('',(0.,0.,0.));
#56338=CARTESIAN_POINT('',(-2.77555756156289E-14,22.,-198.257162217596));
#56339=CARTESIAN_POINT('',(-1.11022302462516E-13,30.0000000000001,-199.257162217596));
#56340=CARTESIAN_POINT('',(-8.32667268468867E-14,22.0000000000001,-323.257162217596));
#56341=CARTESIAN_POINT('',(-1.94289029309402E-13,30.,-324.257162217596));
#56342=CARTESIAN_POINT('',(0.,0.,0.));
#56343=CARTESIAN_POINT('',(-6.93889390390723E-14,22.0000000000001,-198.257162217596));
#56344=CARTESIAN_POINT('',(0.,30.0000000000001,-199.257162217596));
#56345=CARTESIAN_POINT('',(4.16333634234434E-14,22.0000000000001,-323.257162217596));
#56346=CARTESIAN_POINT('',(-1.38777878078145E-14,30.,-324.257162217596));
#56347=CARTESIAN_POINT('',(0.,0.,0.));
#56348=CARTESIAN_POINT('Origin',(-210.,-24.5,0.));
#56349=CARTESIAN_POINT('',(-210.,-7.49999999999999,2.5));
#56350=CARTESIAN_POINT('Origin',(-210.,-7.49999999999999,0.));
#56351=CARTESIAN_POINT('',(-210.,-24.5,2.5));
#56352=CARTESIAN_POINT('',(-210.,-24.5,2.5));
#56353=CARTESIAN_POINT('Origin',(-210.,-24.5,0.));
#56354=CARTESIAN_POINT('Origin',(-210.,-7.49999999999999,0.));
#56355=CARTESIAN_POINT('',(-210.,-5.99784845243109,0.));
#56356=CARTESIAN_POINT('',(-210.,-7.49999999999999,2.5));
#56357=CARTESIAN_POINT('Origin',(-150.,-24.5,0.));
#56358=CARTESIAN_POINT('',(-150.,-7.49999999999999,2.5));
#56359=CARTESIAN_POINT('Origin',(-150.,-7.49999999999999,0.));
#56360=CARTESIAN_POINT('',(-150.,-24.5,2.5));
#56361=CARTESIAN_POINT('',(-150.,-24.5,2.5));
#56362=CARTESIAN_POINT('Origin',(-150.,-24.5,0.));
#56363=CARTESIAN_POINT('Origin',(-150.,-7.49999999999999,0.));
#56364=CARTESIAN_POINT('',(-150.,-5.99784845243109,0.));
#56365=CARTESIAN_POINT('',(-150.,-7.49999999999999,2.5));
#56366=CARTESIAN_POINT('Origin',(-89.9999999999999,-24.5,0.));
#56367=CARTESIAN_POINT('',(-89.9999999999999,-7.49999999999999,2.5));
#56368=CARTESIAN_POINT('Origin',(-89.9999999999999,-7.49999999999999,0.));
#56369=CARTESIAN_POINT('',(-89.9999999999999,-24.5,2.5));
#56370=CARTESIAN_POINT('',(-89.9999999999999,-24.5,2.5));
#56371=CARTESIAN_POINT('Origin',(-89.9999999999999,-24.5,0.));
#56372=CARTESIAN_POINT('Origin',(-89.9999999999999,-7.49999999999999,0.));
#56373=CARTESIAN_POINT('',(-89.9999999999999,-5.99784845243109,0.));
#56374=CARTESIAN_POINT('',(-89.9999999999999,-7.49999999999999,2.5));
#56375=CARTESIAN_POINT('Origin',(-29.9999999999999,-24.5,0.));
#56376=CARTESIAN_POINT('',(-29.9999999999999,-7.49999999999999,2.5));
#56377=CARTESIAN_POINT('Origin',(-29.9999999999999,-7.49999999999999,0.));
#56378=CARTESIAN_POINT('',(-29.9999999999999,-24.5,2.5));
#56379=CARTESIAN_POINT('',(-29.9999999999999,-24.5,2.5));
#56380=CARTESIAN_POINT('Origin',(-29.9999999999999,-24.5,0.));
#56381=CARTESIAN_POINT('Origin',(-29.9999999999999,-7.49999999999999,0.));
#56382=CARTESIAN_POINT('',(-29.9999999999999,-5.99784845243109,0.));
#56383=CARTESIAN_POINT('',(-29.9999999999999,-7.49999999999999,2.5));
#56384=CARTESIAN_POINT('Origin',(30.0000000000001,-24.5,0.));
#56385=CARTESIAN_POINT('',(30.0000000000001,-7.49999999999999,2.5));
#56386=CARTESIAN_POINT('Origin',(30.0000000000001,-7.49999999999999,0.));
#56387=CARTESIAN_POINT('',(30.0000000000001,-24.5,2.5));
#56388=CARTESIAN_POINT('',(30.0000000000001,-24.5,2.5));
#56389=CARTESIAN_POINT('Origin',(30.0000000000001,-24.5,0.));
#56390=CARTESIAN_POINT('Origin',(30.0000000000001,-7.49999999999999,0.));
#56391=CARTESIAN_POINT('',(30.0000000000001,-5.99784845243109,0.));
#56392=CARTESIAN_POINT('',(30.0000000000001,-7.49999999999999,2.5));
#56393=CARTESIAN_POINT('Origin',(90.0000000000001,-24.5,0.));
#56394=CARTESIAN_POINT('',(90.0000000000001,-7.49999999999999,2.5));
#56395=CARTESIAN_POINT('Origin',(90.0000000000001,-7.49999999999999,0.));
#56396=CARTESIAN_POINT('',(90.0000000000001,-24.5,2.5));
#56397=CARTESIAN_POINT('',(90.0000000000001,-24.5,2.5));
#56398=CARTESIAN_POINT('Origin',(90.0000000000001,-24.5,0.));
#56399=CARTESIAN_POINT('Origin',(90.0000000000001,-7.49999999999999,0.));
#56400=CARTESIAN_POINT('',(90.0000000000001,-5.99784845243109,0.));
#56401=CARTESIAN_POINT('',(90.0000000000001,-7.49999999999999,2.5));
#56402=CARTESIAN_POINT('Origin',(150.,-24.5,0.));
#56403=CARTESIAN_POINT('',(150.,-7.49999999999999,2.5));
#56404=CARTESIAN_POINT('Origin',(150.,-7.49999999999999,0.));
#56405=CARTESIAN_POINT('',(150.,-24.5,2.5));
#56406=CARTESIAN_POINT('',(150.,-24.5,2.5));
#56407=CARTESIAN_POINT('Origin',(150.,-24.5,0.));
#56408=CARTESIAN_POINT('Origin',(150.,-7.49999999999999,0.));
#56409=CARTESIAN_POINT('',(150.,-5.99784845243109,0.));
#56410=CARTESIAN_POINT('',(150.,-7.49999999999999,2.5));
#56411=CARTESIAN_POINT('Origin',(210.,-24.5,0.));
#56412=CARTESIAN_POINT('',(210.,-7.49999999999999,2.5));
#56413=CARTESIAN_POINT('Origin',(210.,-7.49999999999999,0.));
#56414=CARTESIAN_POINT('',(210.,-24.5,2.5));
#56415=CARTESIAN_POINT('',(210.,-24.5,2.5));
#56416=CARTESIAN_POINT('Origin',(210.,-24.5,0.));
#56417=CARTESIAN_POINT('Origin',(210.,-7.49999999999999,0.));
#56418=CARTESIAN_POINT('',(210.,-5.99784845243109,0.));
#56419=CARTESIAN_POINT('',(210.,-7.49999999999999,2.5));
#56420=CARTESIAN_POINT('Origin',(-260.,-26.5,17.5));
#56421=CARTESIAN_POINT('',(-260.,-26.5,17.5));
#56422=CARTESIAN_POINT('',(-260.,-26.5,11.5));
#56423=CARTESIAN_POINT('',(-260.,-26.5,17.5));
#56424=CARTESIAN_POINT('',(260.,-26.5,11.5));
#56425=CARTESIAN_POINT('',(-260.,-26.5,11.5));
#56426=CARTESIAN_POINT('',(260.,-26.5,17.5));
#56427=CARTESIAN_POINT('',(260.,-26.5,17.5));
#56428=CARTESIAN_POINT('',(-260.,-26.5,17.5));
#56429=CARTESIAN_POINT('Origin',(260.,26.5,17.5));
#56430=CARTESIAN_POINT('',(260.,-24.7,11.5));
#56431=CARTESIAN_POINT('',(260.,-26.5,11.5));
#56432=CARTESIAN_POINT('',(260.,-24.5,11.3));
#56433=CARTESIAN_POINT('Origin',(260.,-24.7,11.3));
#56434=CARTESIAN_POINT('',(260.,-24.5,-11.3));
#56435=CARTESIAN_POINT('',(260.,-24.5,11.5));
#56436=CARTESIAN_POINT('',(260.,-24.7,-11.5));
#56437=CARTESIAN_POINT('Origin',(260.,-24.7,-11.3));
#56438=CARTESIAN_POINT('',(260.,-26.5,-11.5));
#56439=CARTESIAN_POINT('',(260.,-26.5,-11.5));
#56440=CARTESIAN_POINT('',(260.,-26.5,-17.5));
#56441=CARTESIAN_POINT('',(260.,-26.5,17.5));
#56442=CARTESIAN_POINT('',(260.,26.5,-17.5));
#56443=CARTESIAN_POINT('',(260.,26.5,-17.5));
#56444=CARTESIAN_POINT('',(260.,26.5,17.5));
#56445=CARTESIAN_POINT('',(260.,26.5,17.5));
#56446=CARTESIAN_POINT('',(260.,26.5,17.5));
#56447=CARTESIAN_POINT('Origin',(-260.,26.5,17.5));
#56448=CARTESIAN_POINT('',(-260.,26.5,-17.5));
#56449=CARTESIAN_POINT('',(-260.,26.5,-17.5));
#56450=CARTESIAN_POINT('',(-260.,26.5,17.5));
#56451=CARTESIAN_POINT('',(-260.,26.5,17.5));
#56452=CARTESIAN_POINT('',(-260.,26.5,17.5));
#56453=CARTESIAN_POINT('Origin',(-260.,26.5,17.5));
#56454=CARTESIAN_POINT('',(-260.,-26.5,-11.5));
#56455=CARTESIAN_POINT('',(-260.,-24.7,-11.5));
#56456=CARTESIAN_POINT('',(-260.,-26.5,-11.5));
#56457=CARTESIAN_POINT('',(-260.,-24.5,-11.3));
#56458=CARTESIAN_POINT('Origin',(-260.,-24.7,-11.3));
#56459=CARTESIAN_POINT('',(-260.,-24.5,11.3));
#56460=CARTESIAN_POINT('',(-260.,-24.5,11.5));
#56461=CARTESIAN_POINT('',(-260.,-24.7,11.5));
#56462=CARTESIAN_POINT('Origin',(-260.,-24.7,11.3));
#56463=CARTESIAN_POINT('',(-260.,-26.5,11.5));
#56464=CARTESIAN_POINT('',(-260.,26.5,17.5));
#56465=CARTESIAN_POINT('',(-260.,-26.5,-17.5));
#56466=CARTESIAN_POINT('',(-260.,26.5,-17.5));
#56467=CARTESIAN_POINT('',(-260.,-26.5,17.5));
#56468=CARTESIAN_POINT('Origin',(-260.,-26.5,17.5));
#56469=CARTESIAN_POINT('',(-260.,-26.5,-11.5));
#56470=CARTESIAN_POINT('',(-260.,-26.5,-17.5));
#56471=CARTESIAN_POINT('Origin',(0.,0.,17.5));
#56472=CARTESIAN_POINT('Origin',(0.,0.,-17.5));
#56473=CARTESIAN_POINT('Origin',(-260.,-26.5,11.5));
#56474=CARTESIAN_POINT('',(260.,-24.7,11.5));
#56475=CARTESIAN_POINT('Origin',(-260.,-24.5,11.5));
#56476=CARTESIAN_POINT('',(260.,-24.5,-11.3));
#56477=CARTESIAN_POINT('',(-260.,-24.5,11.3));
#56478=CARTESIAN_POINT('Origin',(-260.,-26.5,-11.5));
#56479=CARTESIAN_POINT('',(-260.,-24.7,-11.5));
#56480=CARTESIAN_POINT('Origin',(-260.,-24.7,-11.3));
#56481=CARTESIAN_POINT('Origin',(-260.,-24.7,11.3));
#56482=CARTESIAN_POINT('',(0.,0.,0.));
#56483=CARTESIAN_POINT('Origin',(-7.3,0.,0.));
#56484=CARTESIAN_POINT('',(-6.79999999999999,5.20474889637625E-16,-4.25));
#56485=CARTESIAN_POINT('',(-6.79999999999999,-5.20474889637625E-16,4.25));
#56486=CARTESIAN_POINT('Origin',(-6.79999999999999,0.,0.));
#56487=CARTESIAN_POINT('Origin',(-6.79999999999999,0.,0.));
#56488=CARTESIAN_POINT('',(-7.3,-4.59242549680257E-16,3.75));
#56489=CARTESIAN_POINT('',(-7.3,-4.59242549680257E-16,3.75));
#56490=CARTESIAN_POINT('Origin',(-7.3,0.,0.));
#56491=CARTESIAN_POINT('Origin',(-1003.59827876194,5.22934144793585E-14,
0.));
#56492=CARTESIAN_POINT('',(-3.59827876194487,-1.94294868429572E-16,0.));
#56493=CARTESIAN_POINT('',(-4.80000000000004,2.00000000000045,-2.44929359829514E-16));
#56494=CARTESIAN_POINT('',(-1003.59827876194,1664.2794823505,-2.03815454094715E-13));
#56495=CARTESIAN_POINT('',(-4.8,1.73205080756888,-1.));
#56496=CARTESIAN_POINT('Origin',(-4.8,-1.3121927336947E-16,0.));
#56497=CARTESIAN_POINT('',(-4.8,-1.3121927336947E-16,-2.));
#56498=CARTESIAN_POINT('Origin',(-4.8,-1.3121927336947E-16,0.));
#56499=CARTESIAN_POINT('',(-4.8,-1.73205080756888,-1.));
#56500=CARTESIAN_POINT('Origin',(-4.8,-1.3121927336947E-16,0.));
#56501=CARTESIAN_POINT('',(-4.8,-1.73205080756888,1.));
#56502=CARTESIAN_POINT('Origin',(-4.8,-1.3121927336947E-16,0.));
#56503=CARTESIAN_POINT('',(-4.8,2.4435937631482E-16,2.));
#56504=CARTESIAN_POINT('Origin',(-4.8,-1.3121927336947E-16,0.));
#56505=CARTESIAN_POINT('',(-4.8,1.73205080756888,0.999999999999999));
#56506=CARTESIAN_POINT('Origin',(-4.8,-1.3121927336947E-16,0.));
#56507=CARTESIAN_POINT('Origin',(-4.8,-1.3121927336947E-16,0.));
#56508=CARTESIAN_POINT('Origin',(-7.3,0.,0.));
#56509=CARTESIAN_POINT('',(-2.3,-5.20474889637625E-16,-4.25));
#56510=CARTESIAN_POINT('',(-7.3,-5.20474889637625E-16,-4.25));
#56511=CARTESIAN_POINT('Origin',(-2.3,0.,0.));
#56512=CARTESIAN_POINT('Origin',(-7.3,0.,0.));
#56513=CARTESIAN_POINT('',(-2.3,-2.52889564023928E-16,-2.065));
#56514=CARTESIAN_POINT('Origin',(-2.3,0.,0.));
#56515=CARTESIAN_POINT('',(2.85,-2.52889564023928E-16,-2.065));
#56516=CARTESIAN_POINT('',(-7.3,-2.52889564023928E-16,-2.065));
#56517=CARTESIAN_POINT('Origin',(2.85,0.,0.));
#56518=CARTESIAN_POINT('Origin',(-7.3,0.,0.));
#56519=CARTESIAN_POINT('',(2.85,-3.06161699786838E-16,-2.5));
#56520=CARTESIAN_POINT('Origin',(2.85,0.,0.));
#56521=CARTESIAN_POINT('',(22.7,-3.06161699786838E-16,-2.5));
#56522=CARTESIAN_POINT('',(-7.3,-3.06161699786838E-16,-2.5));
#56523=CARTESIAN_POINT('Origin',(22.7,0.,0.));
#56524=CARTESIAN_POINT('Origin',(-7.3,0.,0.));
#56525=CARTESIAN_POINT('',(-7.3,1.15470053837925,2.));
#56526=CARTESIAN_POINT('',(-7.3,2.3094010767585,1.33236321473148E-16));
#56527=CARTESIAN_POINT('',(-7.3,1.15470053837925,2.));
#56528=CARTESIAN_POINT('',(-7.3,-1.15470053837925,2.));
#56529=CARTESIAN_POINT('',(-7.3,-1.15470053837925,2.));
#56530=CARTESIAN_POINT('',(-7.3,-2.3094010767585,4.08864764769604E-16));
#56531=CARTESIAN_POINT('',(-7.3,-2.3094010767585,4.08864764769604E-16));
#56532=CARTESIAN_POINT('',(-7.3,-1.15470053837925,-2.));
#56533=CARTESIAN_POINT('',(-7.3,-1.15470053837925,-2.));
#56534=CARTESIAN_POINT('',(-7.3,1.15470053837925,-2.));
#56535=CARTESIAN_POINT('',(-7.3,1.15470053837925,-2.));
#56536=CARTESIAN_POINT('',(-7.3,2.3094010767585,1.33236321473148E-16));
#56537=CARTESIAN_POINT('Origin',(22.7,2.5,0.));
#56538=CARTESIAN_POINT('Origin',(2.85,2.5,0.));
#56539=CARTESIAN_POINT('Origin',(-2.3,2.065,0.));
#56540=CARTESIAN_POINT('Origin',(-4.8,-1.15470053837925,2.));
#56541=CARTESIAN_POINT('',(-4.8,-1.15470053837925,2.));
#56542=CARTESIAN_POINT('',(-4.8,-1.15470053837925,2.));
#56543=CARTESIAN_POINT('',(-4.8,-1.15470053837925,2.));
#56544=CARTESIAN_POINT('',(-4.8,1.15470053837925,2.));
#56545=CARTESIAN_POINT('',(-4.8,1.15470053837925,2.));
#56546=CARTESIAN_POINT('',(-4.8,-1.15470053837925,2.));
#56547=CARTESIAN_POINT('Origin',(-4.8,-2.3094010767585,4.08864764769604E-16));
#56548=CARTESIAN_POINT('',(-4.8,-2.3094010767585,4.08864764769604E-16));
#56549=CARTESIAN_POINT('',(-4.8,-2.3094010767585,4.08864764769604E-16));
#56550=CARTESIAN_POINT('',(-4.8,-2.3094010767585,4.08864764769604E-16));
#56551=CARTESIAN_POINT('',(-4.8,-2.3094010767585,4.08864764769604E-16));
#56552=CARTESIAN_POINT('Origin',(-4.8,-1.15470053837925,-2.));
#56553=CARTESIAN_POINT('',(-4.8,-1.15470053837925,-2.));
#56554=CARTESIAN_POINT('',(-4.8,-1.15470053837925,-2.));
#56555=CARTESIAN_POINT('',(-4.8,-1.15470053837925,-2.));
#56556=CARTESIAN_POINT('',(-4.8,-1.15470053837925,-2.));
#56557=CARTESIAN_POINT('Origin',(-4.8,1.15470053837925,-2.));
#56558=CARTESIAN_POINT('',(-4.8,1.15470053837925,-2.));
#56559=CARTESIAN_POINT('',(-4.8,1.15470053837925,-2.));
#56560=CARTESIAN_POINT('',(-4.8,1.15470053837925,-2.));
#56561=CARTESIAN_POINT('',(-4.8,1.15470053837925,-2.));
#56562=CARTESIAN_POINT('Origin',(-4.8,2.3094010767585,1.33236321473148E-16));
#56563=CARTESIAN_POINT('',(-4.8,2.3094010767585,1.33236321473148E-16));
#56564=CARTESIAN_POINT('',(-4.8,2.3094010767585,1.33236321473148E-16));
#56565=CARTESIAN_POINT('',(-4.8,2.3094010767585,1.33236321473148E-16));
#56566=CARTESIAN_POINT('',(-4.8,2.3094010767585,1.33236321473148E-16));
#56567=CARTESIAN_POINT('Origin',(-4.8,1.15470053837925,2.));
#56568=CARTESIAN_POINT('',(-4.8,1.15470053837925,2.));
#56569=CARTESIAN_POINT('',(-4.8,1.15470053837925,2.));
#56570=CARTESIAN_POINT('Origin',(-4.8,0.,0.));
#56571=CARTESIAN_POINT('Origin',(-4.8,0.,0.));
#56572=CARTESIAN_POINT('Origin',(-4.8,0.,0.));
#56573=CARTESIAN_POINT('Origin',(-4.8,0.,0.));
#56574=CARTESIAN_POINT('Origin',(-4.8,0.,0.));
#56575=CARTESIAN_POINT('Origin',(-4.8,0.,0.));
#56576=CARTESIAN_POINT('Origin',(-7.3,-2.80889253323697E-17,0.));
#56577=CARTESIAN_POINT('',(-1.,5.,-6.12323399573677E-16));
#56578=CARTESIAN_POINT('Origin',(-1.,-3.84779799073558E-18,0.));
#56579=CARTESIAN_POINT('',(0.,5.,-6.12323399573677E-16));
#56580=CARTESIAN_POINT('',(-7.3,5.,-6.12323399573677E-16));
#56581=CARTESIAN_POINT('Origin',(0.,0.,0.));
#56582=CARTESIAN_POINT('Origin',(-7.3,-2.80889253323697E-17,0.));
#56583=CARTESIAN_POINT('',(0.,2.5,-3.06161699786838E-16));
#56584=CARTESIAN_POINT('Origin',(0.,0.,0.));
#56585=CARTESIAN_POINT('',(-1.,2.5,-3.06161699786838E-16));
#56586=CARTESIAN_POINT('',(-7.3,2.5,-3.06161699786838E-16));
#56587=CARTESIAN_POINT('Origin',(-1.,-3.84779799073558E-18,0.));
#56588=CARTESIAN_POINT('Origin',(-1.,5.,0.));
#56589=CARTESIAN_POINT('Origin',(-3.54259174671033E-17,5.,0.));
#56590=CARTESIAN_POINT('Origin',(-2.3,-2.80889253323697E-17,0.));
#56591=CARTESIAN_POINT('',(-1.,1.065,4.11439849795812));
#56592=CARTESIAN_POINT('',(-1.,-1.065,4.11439849795812));
#56593=CARTESIAN_POINT('Origin',(-1.,-1.22125762314651E-17,0.));
#56594=CARTESIAN_POINT('',(-2.3,-1.065,4.11439849795812));
#56595=CARTESIAN_POINT('',(-2.3,-1.065,4.11439849795812));
#56596=CARTESIAN_POINT('',(-2.3,1.065,4.11439849795812));
#56597=CARTESIAN_POINT('Origin',(-2.3,-2.80889253323697E-17,0.));
#56598=CARTESIAN_POINT('',(-2.3,1.065,4.11439849795812));
#56599=CARTESIAN_POINT('Origin',(-2.3,-2.80889253323697E-17,0.));
#56600=CARTESIAN_POINT('',(-1.,1.065,2.26180790519443));
#56601=CARTESIAN_POINT('',(-1.,-1.065,2.26180790519443));
#56602=CARTESIAN_POINT('Origin',(-1.,-1.22125762314651E-17,0.));
#56603=CARTESIAN_POINT('',(-2.3,1.065,2.26180790519443));
#56604=CARTESIAN_POINT('',(-2.3,1.065,2.26180790519443));
#56605=CARTESIAN_POINT('',(-2.3,-1.065,2.26180790519443));
#56606=CARTESIAN_POINT('Origin',(-2.3,-2.80889253323697E-17,0.));
#56607=CARTESIAN_POINT('',(-2.3,-1.065,2.26180790519443));
#56608=CARTESIAN_POINT('Origin',(-2.3,4.25,0.));
#56609=CARTESIAN_POINT('',(-2.3,-1.065,4.11439849795812));
#56610=CARTESIAN_POINT('',(-2.3,1.065,4.11439849795812));
#56611=CARTESIAN_POINT('Origin',(-1.,4.25,0.));
#56612=CARTESIAN_POINT('',(-1.,-1.065,4.11439849795812));
#56613=CARTESIAN_POINT('',(-1.,1.065,4.11439849795812));
#56614=CARTESIAN_POINT('Origin',(-2.3,1.065,4.11439849795812));
#56615=CARTESIAN_POINT('Origin',(-2.3,-1.065,4.11439849795812));
#56616=CARTESIAN_POINT('',(0.,0.,0.));
#56617=CARTESIAN_POINT('Origin',(25.,2.32682891837997E-15,0.));
#56618=CARTESIAN_POINT('',(0.,-5.,-6.12323399573677E-16));
#56619=CARTESIAN_POINT('Origin',(0.,-7.34788079488413E-16,0.));
#56620=CARTESIAN_POINT('',(-5.4,-5.,-6.12323399573677E-16));
#56621=CARTESIAN_POINT('',(25.,-5.,-6.12323399573677E-16));
#56622=CARTESIAN_POINT('Origin',(-5.4,-1.39609735102798E-15,0.));
#56623=CARTESIAN_POINT('Origin',(-5.4,-1.39609735102798E-15,0.));
#56624=CARTESIAN_POINT('',(-6.,-4.4,-5.38844591624836E-16));
#56625=CARTESIAN_POINT('',(-5.4,-5.,-6.12323399573677E-16));
#56626=CARTESIAN_POINT('Origin',(-6.,-1.46957615897682E-15,0.));
#56627=CARTESIAN_POINT('Origin',(25.,2.32682891837997E-15,0.));
#56628=CARTESIAN_POINT('',(24.4585,-3.,3.67394039744206E-16));
#56629=CARTESIAN_POINT('',(24.4585,3.,-3.67394039744206E-16));
#56630=CARTESIAN_POINT('Origin',(24.4585,2.26051429420614E-15,0.));
#56631=CARTESIAN_POINT('',(25.,2.4585,-3.01079415570377E-16));
#56632=CARTESIAN_POINT('',(25.,2.4585,-3.01079415570377E-16));
#56633=CARTESIAN_POINT('Origin',(25.,2.32682891837997E-15,0.));
#56634=CARTESIAN_POINT('Origin',(24.4585,2.26051429420614E-15,0.));
#56635=CARTESIAN_POINT('Origin',(25.,2.32682891837997E-15,0.));
#56636=CARTESIAN_POINT('',(0.,-3.,-3.67394039744206E-16));
#56637=CARTESIAN_POINT('',(25.,-3.,-3.67394039744206E-16));
#56638=CARTESIAN_POINT('Origin',(0.,-7.34788079488413E-16,0.));
#56639=CARTESIAN_POINT('Origin',(25.,2.4585,0.));
#56640=CARTESIAN_POINT('Origin',(-6.,-1.46957615897682E-15,0.));
#56641=CARTESIAN_POINT('',(-6.,1.44337567297406,2.5));
#56642=CARTESIAN_POINT('',(-6.,2.88675134594813,0.));
#56643=CARTESIAN_POINT('',(-6.,1.44337567297406,2.5));
#56644=CARTESIAN_POINT('',(-6.,-1.44337567297407,2.5));
#56645=CARTESIAN_POINT('',(-6.,-1.44337567297407,2.5));
#56646=CARTESIAN_POINT('',(-6.,-2.88675134594813,-7.77133304087269E-16));
#56647=CARTESIAN_POINT('',(-6.,-2.88675134594813,-7.77133304087269E-16));
#56648=CARTESIAN_POINT('',(-6.,-1.44337567297407,-2.5));
#56649=CARTESIAN_POINT('',(-6.,-1.44337567297407,-2.5));
#56650=CARTESIAN_POINT('',(-6.,1.44337567297406,-2.5));
#56651=CARTESIAN_POINT('',(-6.,1.44337567297406,-2.5));
#56652=CARTESIAN_POINT('',(-6.,2.88675134594813,3.50584097974525E-17));
#56653=CARTESIAN_POINT('Origin',(1.22464679914735E-16,3.,0.));
#56654=CARTESIAN_POINT('Origin',(-3.,1.44337567297406,2.5));
#56655=CARTESIAN_POINT('',(-3.,2.88675134594813,3.50584097974525E-17));
#56656=CARTESIAN_POINT('',(-3.,2.88675134594813,3.50584097974525E-17));
#56657=CARTESIAN_POINT('',(-3.,1.44337567297406,2.5));
#56658=CARTESIAN_POINT('',(-3.,1.44337567297406,2.5));
#56659=CARTESIAN_POINT('',(-3.,1.44337567297406,2.5));
#56660=CARTESIAN_POINT('Origin',(-3.,-1.44337567297407,2.5));
#56661=CARTESIAN_POINT('',(-3.,-1.44337567297407,2.5));
#56662=CARTESIAN_POINT('',(-3.,-1.44337567297407,2.5));
#56663=CARTESIAN_POINT('',(-3.,-1.44337567297407,2.5));
#56664=CARTESIAN_POINT('Origin',(-3.,-2.88675134594813,-7.77133304087269E-16));
#56665=CARTESIAN_POINT('',(-3.,-2.88675134594813,-7.77133304087269E-16));
#56666=CARTESIAN_POINT('',(-3.,-2.88675134594813,-7.77133304087269E-16));
#56667=CARTESIAN_POINT('',(-3.,-2.88675134594813,-7.77133304087269E-16));
#56668=CARTESIAN_POINT('Origin',(-3.,-1.44337567297406,-2.5));
#56669=CARTESIAN_POINT('',(-3.,-1.44337567297406,-2.5));
#56670=CARTESIAN_POINT('',(-3.,-1.44337567297406,-2.5));
#56671=CARTESIAN_POINT('',(-3.,-1.44337567297406,-2.5));
#56672=CARTESIAN_POINT('Origin',(-3.,1.44337567297407,-2.5));
#56673=CARTESIAN_POINT('',(-3.,1.44337567297407,-2.5));
#56674=CARTESIAN_POINT('',(-3.,1.44337567297407,-2.5));
#56675=CARTESIAN_POINT('',(-3.,1.44337567297407,-2.5));
#56676=CARTESIAN_POINT('Origin',(-3.,2.88675134594813,3.50584097974525E-17));
#56677=CARTESIAN_POINT('',(-3.,2.88675134594813,3.50584097974525E-17));
#56678=CARTESIAN_POINT('Origin',(-3.,3.67394039744206E-16,0.));
#56679=CARTESIAN_POINT('',(0.,0.,0.));
#56680=CARTESIAN_POINT('Origin',(-11.6,0.,0.));
#56681=CARTESIAN_POINT('',(-10.8,7.9602041944578E-16,-6.5));
#56682=CARTESIAN_POINT('',(-10.8,-7.9602041944578E-16,6.5));
#56683=CARTESIAN_POINT('Origin',(-10.8,0.,0.));
#56684=CARTESIAN_POINT('Origin',(-10.8,0.,0.));
#56685=CARTESIAN_POINT('',(-11.6,-6.98048675513991E-16,5.7));
#56686=CARTESIAN_POINT('',(-11.6,-6.98048675513991E-16,5.7));
#56687=CARTESIAN_POINT('Origin',(-11.6,0.,0.));
#56688=CARTESIAN_POINT('Origin',(-1005.79741814292,7.0442721316922E-14,
0.));
#56689=CARTESIAN_POINT('',(-5.7974181429173,-4.11135302926673E-16,0.));
#56690=CARTESIAN_POINT('',(-7.60000000000019,3.0000000000004,-3.67394039744256E-16));
#56691=CARTESIAN_POINT('',(-1005.79741814292,1664.2794823505,-2.03815454094715E-13));
#56692=CARTESIAN_POINT('',(-7.6,2.59807621135332,-1.5));
#56693=CARTESIAN_POINT('Origin',(-7.6,-2.83415426479395E-16,0.));
#56694=CARTESIAN_POINT('',(-7.6,-2.83415426479395E-16,-3.));
#56695=CARTESIAN_POINT('Origin',(-7.6,-2.83415426479395E-16,0.));
#56696=CARTESIAN_POINT('',(-7.6,-2.59807621135332,-1.5));
#56697=CARTESIAN_POINT('Origin',(-7.6,-2.83415426479395E-16,0.));
#56698=CARTESIAN_POINT('',(-7.6,-2.59807621135332,1.5));
#56699=CARTESIAN_POINT('Origin',(-7.6,-2.83415426479395E-16,0.));
#56700=CARTESIAN_POINT('',(-7.6,9.2163223204895E-17,3.));
#56701=CARTESIAN_POINT('Origin',(-7.6,-2.83415426479395E-16,0.));
#56702=CARTESIAN_POINT('',(-7.6,2.59807621135331,1.5));
#56703=CARTESIAN_POINT('Origin',(-7.6,-2.83415426479395E-16,0.));
#56704=CARTESIAN_POINT('Origin',(-7.6,-2.83415426479395E-16,0.));
#56705=CARTESIAN_POINT('Origin',(-11.6,0.,0.));
#56706=CARTESIAN_POINT('',(-3.6,-7.96020419445779E-16,-6.5));
#56707=CARTESIAN_POINT('',(-11.6,-7.96020419445779E-16,-6.5));
#56708=CARTESIAN_POINT('Origin',(-3.6,0.,0.));
#56709=CARTESIAN_POINT('Origin',(-11.6,0.,0.));
#56710=CARTESIAN_POINT('',(-3.6,-4.06888899016708E-16,-3.3225));
#56711=CARTESIAN_POINT('Origin',(-3.6,0.,0.));
#56712=CARTESIAN_POINT('',(4.8,-4.06888899016708E-16,-3.3225));
#56713=CARTESIAN_POINT('',(-11.6,-4.06888899016708E-16,-3.3225));
#56714=CARTESIAN_POINT('Origin',(4.8,0.,0.));
#56715=CARTESIAN_POINT('Origin',(-11.6,0.,0.));
#56716=CARTESIAN_POINT('',(4.8,-4.89858719658941E-16,-4.));
#56717=CARTESIAN_POINT('Origin',(4.8,0.,0.));
#56718=CARTESIAN_POINT('',(41.4,-4.89858719658941E-16,-4.));
#56719=CARTESIAN_POINT('',(-11.6,-4.89858719658941E-16,-4.));
#56720=CARTESIAN_POINT('Origin',(41.4,0.,0.));
#56721=CARTESIAN_POINT('Origin',(-11.6,0.,0.));
#56722=CARTESIAN_POINT('',(-11.6,1.73205080756888,3.));
#56723=CARTESIAN_POINT('',(-11.6,3.46410161513775,-1.37814221648228E-16));
#56724=CARTESIAN_POINT('',(-11.6,1.73205080756888,3.));
#56725=CARTESIAN_POINT('',(-11.6,-1.73205080756888,3.));
#56726=CARTESIAN_POINT('',(-11.6,-1.73205080756888,3.));
#56727=CARTESIAN_POINT('',(-11.6,-3.46410161513776,-2.41656538721699E-16));
#56728=CARTESIAN_POINT('',(-11.6,-3.46410161513776,-2.41656538721699E-16));
#56729=CARTESIAN_POINT('',(-11.6,-1.73205080756888,-3.));
#56730=CARTESIAN_POINT('',(-11.6,-1.73205080756888,-3.));
#56731=CARTESIAN_POINT('',(-11.6,1.73205080756888,-3.));
#56732=CARTESIAN_POINT('',(-11.6,1.73205080756888,-3.));
#56733=CARTESIAN_POINT('',(-11.6,3.46410161513775,-1.37814221648228E-16));
#56734=CARTESIAN_POINT('Origin',(41.4,4.,0.));
#56735=CARTESIAN_POINT('Origin',(4.8,4.,0.));
#56736=CARTESIAN_POINT('Origin',(-3.6,3.3225,0.));
#56737=CARTESIAN_POINT('Origin',(-7.6,-1.73205080756888,3.));
#56738=CARTESIAN_POINT('',(-7.6,-1.73205080756888,3.));
#56739=CARTESIAN_POINT('',(-7.6,-1.73205080756888,3.));
#56740=CARTESIAN_POINT('',(-7.6,-1.73205080756888,3.));
#56741=CARTESIAN_POINT('',(-7.6,1.73205080756888,3.));
#56742=CARTESIAN_POINT('',(-7.6,1.73205080756888,3.));
#56743=CARTESIAN_POINT('',(-7.6,-1.73205080756888,3.));
#56744=CARTESIAN_POINT('Origin',(-7.6,-3.46410161513776,-2.41656538721699E-16));
#56745=CARTESIAN_POINT('',(-7.6,-3.46410161513776,-2.41656538721699E-16));
#56746=CARTESIAN_POINT('',(-7.6,-3.46410161513776,-2.41656538721699E-16));
#56747=CARTESIAN_POINT('',(-7.6,-3.46410161513776,-2.41656538721699E-16));
#56748=CARTESIAN_POINT('',(-7.6,-3.46410161513776,-2.41656538721699E-16));
#56749=CARTESIAN_POINT('Origin',(-7.6,-1.73205080756888,-3.));
#56750=CARTESIAN_POINT('',(-7.6,-1.73205080756888,-3.));
#56751=CARTESIAN_POINT('',(-7.6,-1.73205080756888,-3.));
#56752=CARTESIAN_POINT('',(-7.6,-1.73205080756888,-3.));
#56753=CARTESIAN_POINT('',(-7.6,-1.73205080756888,-3.));
#56754=CARTESIAN_POINT('Origin',(-7.6,1.73205080756888,-3.));
#56755=CARTESIAN_POINT('',(-7.6,1.73205080756888,-3.));
#56756=CARTESIAN_POINT('',(-7.6,1.73205080756888,-3.));
#56757=CARTESIAN_POINT('',(-7.6,1.73205080756888,-3.));
#56758=CARTESIAN_POINT('',(-7.6,1.73205080756888,-3.));
#56759=CARTESIAN_POINT('Origin',(-7.6,3.46410161513775,-1.37814221648228E-16));
#56760=CARTESIAN_POINT('',(-7.6,3.46410161513775,-1.37814221648228E-16));
#56761=CARTESIAN_POINT('',(-7.6,3.46410161513775,-1.37814221648228E-16));
#56762=CARTESIAN_POINT('',(-7.6,3.46410161513775,-1.37814221648228E-16));
#56763=CARTESIAN_POINT('',(-7.6,3.46410161513775,-1.37814221648228E-16));
#56764=CARTESIAN_POINT('Origin',(-7.6,1.73205080756888,3.));
#56765=CARTESIAN_POINT('',(-7.6,1.73205080756888,3.));
#56766=CARTESIAN_POINT('',(-7.6,1.73205080756888,3.));
#56767=CARTESIAN_POINT('Origin',(-7.6,0.,0.));
#56768=CARTESIAN_POINT('Origin',(-7.6,0.,0.));
#56769=CARTESIAN_POINT('Origin',(-7.6,0.,0.));
#56770=CARTESIAN_POINT('Origin',(-7.6,0.,0.));
#56771=CARTESIAN_POINT('Origin',(-7.6,0.,0.));
#56772=CARTESIAN_POINT('Origin',(-7.6,0.,0.));
#56773=CARTESIAN_POINT('Origin',(-11.6,-1.3650914258092E-16,0.));
#56774=CARTESIAN_POINT('',(-1.6,8.,-9.79717439317883E-16));
#56775=CARTESIAN_POINT('Origin',(-1.6,-1.88288472525407E-17,0.));
#56776=CARTESIAN_POINT('',(0.,8.,-9.79717439317883E-16));
#56777=CARTESIAN_POINT('',(-11.6,8.,-9.79717439317883E-16));
#56778=CARTESIAN_POINT('Origin',(0.,0.,0.));
#56779=CARTESIAN_POINT('Origin',(-11.6,-1.3650914258092E-16,0.));
#56780=CARTESIAN_POINT('',(0.,4.,-4.89858719658941E-16));
#56781=CARTESIAN_POINT('Origin',(0.,0.,0.));
#56782=CARTESIAN_POINT('',(-1.6,4.,-4.89858719658941E-16));
#56783=CARTESIAN_POINT('',(-11.6,4.,-4.89858719658941E-16));
#56784=CARTESIAN_POINT('Origin',(-1.6,-1.88288472525407E-17,0.));
#56785=CARTESIAN_POINT('Origin',(-1.6,8.,0.));
#56786=CARTESIAN_POINT('Origin',(-3.29697758852514E-16,8.,0.));
#56787=CARTESIAN_POINT('Origin',(-3.6,-1.3650914258092E-16,0.));
#56788=CARTESIAN_POINT('',(-1.6,1.815,7.01913634288436));
#56789=CARTESIAN_POINT('',(-1.6,-1.815,7.01913634288436));
#56790=CARTESIAN_POINT('Origin',(-1.6,-6.06707300359645E-17,0.));
#56791=CARTESIAN_POINT('',(-3.6,-1.815,7.01913634288436));
#56792=CARTESIAN_POINT('',(-3.6,-1.815,7.01913634288436));
#56793=CARTESIAN_POINT('',(-3.6,1.815,7.01913634288436));
#56794=CARTESIAN_POINT('Origin',(-3.6,-1.3650914258092E-16,0.));
#56795=CARTESIAN_POINT('',(-3.6,1.815,7.01913634288436));
#56796=CARTESIAN_POINT('Origin',(-3.6,-1.3650914258092E-16,0.));
#56797=CARTESIAN_POINT('',(-1.6,1.815,3.56451609619034));
#56798=CARTESIAN_POINT('',(-1.6,-1.815,3.56451609619034));
#56799=CARTESIAN_POINT('Origin',(-1.6,-6.06707300359645E-17,0.));
#56800=CARTESIAN_POINT('',(-3.6,1.815,3.56451609619034));
#56801=CARTESIAN_POINT('',(-3.6,1.815,3.56451609619034));
#56802=CARTESIAN_POINT('',(-3.6,-1.815,3.56451609619034));
#56803=CARTESIAN_POINT('Origin',(-3.6,-1.3650914258092E-16,0.));
#56804=CARTESIAN_POINT('',(-3.6,-1.815,3.56451609619034));
#56805=CARTESIAN_POINT('Origin',(-3.6,7.25,0.));
#56806=CARTESIAN_POINT('',(-3.6,-1.815,7.01913634288436));
#56807=CARTESIAN_POINT('',(-3.6,1.815,7.01913634288436));
#56808=CARTESIAN_POINT('Origin',(-1.6,7.25,0.));
#56809=CARTESIAN_POINT('',(-1.6,-1.815,7.01913634288436));
#56810=CARTESIAN_POINT('',(-1.6,1.815,7.01913634288436));
#56811=CARTESIAN_POINT('Origin',(-3.6,1.815,7.01913634288436));
#56812=CARTESIAN_POINT('Origin',(-3.6,-1.815,7.01913634288436));
#56813=CARTESIAN_POINT('',(0.,0.,0.));
#56814=CARTESIAN_POINT('Origin',(20.,1.71450551880629E-15,0.));
#56815=CARTESIAN_POINT('',(0.,-5.,-6.12323399573677E-16));
#56816=CARTESIAN_POINT('Origin',(0.,-7.34788079488412E-16,0.));
#56817=CARTESIAN_POINT('',(-5.4,-5.,-6.12323399573677E-16));
#56818=CARTESIAN_POINT('',(20.,-5.,-6.12323399573677E-16));
#56819=CARTESIAN_POINT('Origin',(-5.4,-1.39609735102798E-15,0.));
#56820=CARTESIAN_POINT('Origin',(-5.4,-1.39609735102798E-15,0.));
#56821=CARTESIAN_POINT('',(-6.,-4.4,-5.38844591624836E-16));
#56822=CARTESIAN_POINT('',(-5.4,-5.,-6.12323399573677E-16));
#56823=CARTESIAN_POINT('Origin',(-6.,-1.46957615897682E-15,0.));
#56824=CARTESIAN_POINT('Origin',(20.,1.71450551880629E-15,0.));
#56825=CARTESIAN_POINT('',(19.4585,-3.,3.67394039744206E-16));
#56826=CARTESIAN_POINT('',(19.4585,3.,-3.67394039744206E-16));
#56827=CARTESIAN_POINT('Origin',(19.4585,1.64819089463247E-15,0.));
#56828=CARTESIAN_POINT('',(20.,2.4585,-3.01079415570377E-16));
#56829=CARTESIAN_POINT('',(20.,2.4585,-3.01079415570377E-16));
#56830=CARTESIAN_POINT('Origin',(20.,1.71450551880629E-15,0.));
#56831=CARTESIAN_POINT('Origin',(19.4585,1.64819089463247E-15,0.));
#56832=CARTESIAN_POINT('Origin',(20.,1.71450551880629E-15,0.));
#56833=CARTESIAN_POINT('',(0.,-3.,-3.67394039744206E-16));
#56834=CARTESIAN_POINT('',(20.,-3.,-3.67394039744206E-16));
#56835=CARTESIAN_POINT('Origin',(0.,-7.34788079488412E-16,0.));
#56836=CARTESIAN_POINT('Origin',(20.,2.4585,0.));
#56837=CARTESIAN_POINT('Origin',(-6.,-1.46957615897682E-15,0.));
#56838=CARTESIAN_POINT('',(-6.,1.44337567297406,2.5));
#56839=CARTESIAN_POINT('',(-6.,2.88675134594813,0.));
#56840=CARTESIAN_POINT('',(-6.,1.44337567297406,2.5));
#56841=CARTESIAN_POINT('',(-6.,-1.44337567297407,2.5));
#56842=CARTESIAN_POINT('',(-6.,-1.44337567297407,2.5));
#56843=CARTESIAN_POINT('',(-6.,-2.88675134594813,-7.77133304087269E-16));
#56844=CARTESIAN_POINT('',(-6.,-2.88675134594813,-7.77133304087269E-16));
#56845=CARTESIAN_POINT('',(-6.,-1.44337567297407,-2.5));
#56846=CARTESIAN_POINT('',(-6.,-1.44337567297407,-2.5));
#56847=CARTESIAN_POINT('',(-6.,1.44337567297406,-2.5));
#56848=CARTESIAN_POINT('',(-6.,1.44337567297406,-2.5));
#56849=CARTESIAN_POINT('',(-6.,2.88675134594813,3.50584097974525E-17));
#56850=CARTESIAN_POINT('Origin',(1.22464679914735E-16,3.,0.));
#56851=CARTESIAN_POINT('Origin',(-3.,1.44337567297406,2.5));
#56852=CARTESIAN_POINT('',(-3.,2.88675134594813,3.50584097974525E-17));
#56853=CARTESIAN_POINT('',(-3.,2.88675134594813,3.50584097974525E-17));
#56854=CARTESIAN_POINT('',(-3.,1.44337567297406,2.5));
#56855=CARTESIAN_POINT('',(-3.,1.44337567297406,2.5));
#56856=CARTESIAN_POINT('',(-3.,1.44337567297406,2.5));
#56857=CARTESIAN_POINT('Origin',(-3.,-1.44337567297407,2.5));
#56858=CARTESIAN_POINT('',(-3.,-1.44337567297407,2.5));
#56859=CARTESIAN_POINT('',(-3.,-1.44337567297407,2.5));
#56860=CARTESIAN_POINT('',(-3.,-1.44337567297407,2.5));
#56861=CARTESIAN_POINT('Origin',(-3.,-2.88675134594813,-7.77133304087269E-16));
#56862=CARTESIAN_POINT('',(-3.,-2.88675134594813,-7.77133304087269E-16));
#56863=CARTESIAN_POINT('',(-3.,-2.88675134594813,-7.77133304087269E-16));
#56864=CARTESIAN_POINT('',(-3.,-2.88675134594813,-7.77133304087269E-16));
#56865=CARTESIAN_POINT('Origin',(-3.,-1.44337567297406,-2.5));
#56866=CARTESIAN_POINT('',(-3.,-1.44337567297406,-2.5));
#56867=CARTESIAN_POINT('',(-3.,-1.44337567297406,-2.5));
#56868=CARTESIAN_POINT('',(-3.,-1.44337567297406,-2.5));
#56869=CARTESIAN_POINT('Origin',(-3.,1.44337567297407,-2.5));
#56870=CARTESIAN_POINT('',(-3.,1.44337567297407,-2.5));
#56871=CARTESIAN_POINT('',(-3.,1.44337567297407,-2.5));
#56872=CARTESIAN_POINT('',(-3.,1.44337567297407,-2.5));
#56873=CARTESIAN_POINT('Origin',(-3.,2.88675134594813,3.50584097974525E-17));
#56874=CARTESIAN_POINT('',(-3.,2.88675134594813,3.50584097974525E-17));
#56875=CARTESIAN_POINT('Origin',(-3.,3.67394039744206E-16,0.));
#56876=CARTESIAN_POINT('',(0.,0.,0.));
#56877=CARTESIAN_POINT('Origin',(20.,1.71450551880629E-15,0.));
#56878=CARTESIAN_POINT('',(0.,-3.5,-4.28626379701574E-16));
#56879=CARTESIAN_POINT('Origin',(0.,-7.34788079488412E-16,0.));
#56880=CARTESIAN_POINT('',(-3.6,-3.5,-4.28626379701574E-16));
#56881=CARTESIAN_POINT('',(20.,-3.5,-4.28626379701574E-16));
#56882=CARTESIAN_POINT('Origin',(-3.6,-1.17566092718146E-15,0.));
#56883=CARTESIAN_POINT('Origin',(-3.6,-1.17566092718146E-15,0.));
#56884=CARTESIAN_POINT('',(-4.,-3.1,-3.7964050773568E-16));
#56885=CARTESIAN_POINT('',(-3.6,-3.5,-4.28626379701574E-16));
#56886=CARTESIAN_POINT('Origin',(-4.,-1.22464679914735E-15,0.));
#56887=CARTESIAN_POINT('Origin',(20.,1.71450551880629E-15,0.));
#56888=CARTESIAN_POINT('',(19.621,-2.,2.4492935982947E-16));
#56889=CARTESIAN_POINT('',(19.621,2.,-2.4492935982947E-16));
#56890=CARTESIAN_POINT('Origin',(19.621,1.66809140511861E-15,0.));
#56891=CARTESIAN_POINT('',(20.,1.621,-1.98515246141786E-16));
#56892=CARTESIAN_POINT('',(20.,1.621,-1.98515246141786E-16));
#56893=CARTESIAN_POINT('Origin',(20.,1.71450551880629E-15,0.));
#56894=CARTESIAN_POINT('Origin',(19.621,1.66809140511861E-15,0.));
#56895=CARTESIAN_POINT('Origin',(20.,1.71450551880629E-15,0.));
#56896=CARTESIAN_POINT('',(0.,-2.,-2.44929359829471E-16));
#56897=CARTESIAN_POINT('',(20.,-2.,-2.44929359829471E-16));
#56898=CARTESIAN_POINT('Origin',(0.,-7.34788079488412E-16,0.));
#56899=CARTESIAN_POINT('Origin',(20.,1.621,0.));
#56900=CARTESIAN_POINT('Origin',(-4.,-1.22464679914735E-15,0.));
#56901=CARTESIAN_POINT('',(-4.,0.866025403784438,1.5));
#56902=CARTESIAN_POINT('',(-4.,1.73205080756888,1.0842021724855E-16));
#56903=CARTESIAN_POINT('',(-4.,0.866025403784438,1.5));
#56904=CARTESIAN_POINT('',(-4.,-0.866025403784439,1.5));
#56905=CARTESIAN_POINT('',(-4.,-0.866025403784439,1.5));
#56906=CARTESIAN_POINT('',(-4.,-1.73205080756888,-5.3318781527803E-16));
#56907=CARTESIAN_POINT('',(-4.,-1.73205080756888,-5.3318781527803E-16));
#56908=CARTESIAN_POINT('',(-4.,-0.866025403784439,-1.5));
#56909=CARTESIAN_POINT('',(-4.,-0.866025403784439,-1.5));
#56910=CARTESIAN_POINT('',(-4.,0.866025403784438,-1.5));
#56911=CARTESIAN_POINT('',(-4.,0.866025403784438,-1.5));
#56912=CARTESIAN_POINT('',(-4.,1.73205080756888,1.43478627046003E-16));
#56913=CARTESIAN_POINT('Origin',(9.18485099360515E-17,2.,0.));
#56914=CARTESIAN_POINT('Origin',(-2.,0.866025403784439,1.5));
#56915=CARTESIAN_POINT('',(-2.,1.73205080756888,1.43478627046003E-16));
#56916=CARTESIAN_POINT('',(-2.,1.73205080756888,1.43478627046003E-16));
#56917=CARTESIAN_POINT('',(-2.,0.866025403784439,1.5));
#56918=CARTESIAN_POINT('',(-2.,0.866025403784439,1.5));
#56919=CARTESIAN_POINT('',(-2.,0.866025403784439,1.5));
#56920=CARTESIAN_POINT('Origin',(-2.,-0.866025403784439,1.5));
#56921=CARTESIAN_POINT('',(-2.,-0.866025403784439,1.5));
#56922=CARTESIAN_POINT('',(-2.,-0.866025403784439,1.5));
#56923=CARTESIAN_POINT('',(-2.,-0.866025403784439,1.5));
#56924=CARTESIAN_POINT('Origin',(-2.,-1.73205080756888,-5.3318781527803E-16));
#56925=CARTESIAN_POINT('',(-2.,-1.73205080756888,-5.3318781527803E-16));
#56926=CARTESIAN_POINT('',(-2.,-1.73205080756888,-5.3318781527803E-16));
#56927=CARTESIAN_POINT('',(-2.,-1.73205080756888,-5.3318781527803E-16));
#56928=CARTESIAN_POINT('Origin',(-2.,-0.866025403784439,-1.5));
#56929=CARTESIAN_POINT('',(-2.,-0.866025403784439,-1.5));
#56930=CARTESIAN_POINT('',(-2.,-0.866025403784439,-1.5));
#56931=CARTESIAN_POINT('',(-2.,-0.866025403784439,-1.5));
#56932=CARTESIAN_POINT('Origin',(-2.,0.866025403784439,-1.5));
#56933=CARTESIAN_POINT('',(-2.,0.866025403784439,-1.5));
#56934=CARTESIAN_POINT('',(-2.,0.866025403784439,-1.5));
#56935=CARTESIAN_POINT('',(-2.,0.866025403784439,-1.5));
#56936=CARTESIAN_POINT('Origin',(-2.,1.73205080756888,1.43478627046003E-16));
#56937=CARTESIAN_POINT('',(-2.,1.73205080756888,1.43478627046003E-16));
#56938=CARTESIAN_POINT('Origin',(-2.,2.44929359829471E-16,0.));
#56939=CARTESIAN_POINT('',(0.,0.,0.));
#56940=CARTESIAN_POINT('',(122.5,-34.,-5.59425427943363E-14));
#56941=CARTESIAN_POINT('',(122.5,-58.5,210.));
#56942=CARTESIAN_POINT('',(-1.36721385474822E-12,-37.4999999999967,-197.));
#56943=CARTESIAN_POINT('',(-1.32061815674872E-12,-12.4999999999967,148.5));
#56944=CARTESIAN_POINT('',(1.02654022301002E-14,-12.4999999999999,-200.05));
#56945=CARTESIAN_POINT('',(-0.999999999998616,-11.5000000000001,161.000000000002));
#56946=CARTESIAN_POINT('',(1.00000000000002,-11.4999999999999,-190.55));
#56947=CARTESIAN_POINT('',(-1.06520000139749E-15,-35.,265.));
#56948=CARTESIAN_POINT('',(-1.90819582357449E-14,-37.4999999999998,222.));
#56949=CARTESIAN_POINT('',(5.48400931670126E-13,-47.4999999999999,-93.1571622175961));
#56950=CARTESIAN_POINT('',(4.51194633617262E-15,-91.9999999999999,-93.1571622175961));
#56951=CARTESIAN_POINT('',(6.44229131646814E-15,-414.5,-93.157162217596));
#56952=CARTESIAN_POINT('',(-122.5,-58.4999999999999,210.));
#56953=CARTESIAN_POINT('',(26.0000000000014,-36.5000000000002,160.500000000002));
#56954=CARTESIAN_POINT('',(24.7487373415292,-62.2487373415285,279.));
#56955=CARTESIAN_POINT('',(24.,-3.24673155304979E-14,263.6));
#56956=CARTESIAN_POINT('',(-13.4350288425457,-24.0649711574523,-76.1571622175961));
#56957=CARTESIAN_POINT('',(122.5,-71.5000000000001,210.));
#56958=CARTESIAN_POINT('',(-122.5,-33.9999999999999,-2.73494213916588E-13));
#56959=CARTESIAN_POINT('',(-26.,-36.5000000000001,160.5));
#56960=CARTESIAN_POINT('',(-24.,-1.07879024010279E-14,263.6));
#56961=CARTESIAN_POINT('',(13.4350288425437,-24.0649711574523,-76.1571622175961));
#56962=CARTESIAN_POINT('',(-19.0000000000014,-37.4999999999967,-76.1571622175961));
#56963=CARTESIAN_POINT('',(18.9999999999994,-37.4999999999967,-76.1571622175961));
#56964=CARTESIAN_POINT('',(-13.4350288425458,-50.9350288425411,-76.1571622175961));
#56965=CARTESIAN_POINT('',(13.4350288425437,-50.9350288425411,-76.1571622175961));
#56966=CARTESIAN_POINT('',(-122.5,-71.4999999999998,-210.));
#56967=CARTESIAN_POINT('',(122.5,-71.5,-210.));
#56968=CARTESIAN_POINT('',(-122.5,-71.4999999999998,-150.));
#56969=CARTESIAN_POINT('',(122.5,-71.5,-150.));
#56970=CARTESIAN_POINT('',(-122.5,-71.4999999999998,-89.9999999999998));
#56971=CARTESIAN_POINT('',(122.5,-71.5,-89.9999999999998));
#56972=CARTESIAN_POINT('',(-122.5,-71.4999999999998,-29.9999999999998));
#56973=CARTESIAN_POINT('',(122.5,-71.5000000000001,-29.9999999999998));
#56974=CARTESIAN_POINT('',(-122.5,-71.4999999999998,30.0000000000002));
#56975=CARTESIAN_POINT('',(122.5,-71.5000000000001,30.0000000000002));
#56976=CARTESIAN_POINT('',(-122.5,-71.4999999999998,90.0000000000002));
#56977=CARTESIAN_POINT('',(122.5,-71.5000000000001,90.0000000000002));
#56978=CARTESIAN_POINT('',(-122.5,-71.4999999999998,150.));
#56979=CARTESIAN_POINT('',(122.5,-71.5000000000001,150.));
#56980=CARTESIAN_POINT('',(-122.5,-71.4999999999998,210.));
#56981=CARTESIAN_POINT('',(151.,-100.1,-178.157162217596));
#56982=CARTESIAN_POINT('',(-26.,-36.4999999999999,-190.05));
#56983=CARTESIAN_POINT('',(26.,-36.4999999999999,-190.05));
#56984=CARTESIAN_POINT('',(94.,-100.1,-178.157162217596));
#56985=CARTESIAN_POINT('',(151.,-100.1,-133.157162217596));
#56986=CARTESIAN_POINT('',(94.,-100.1,-133.157162217596));
#56987=CARTESIAN_POINT('',(-94.,-100.1,-178.157162217596));
#56988=CARTESIAN_POINT('',(-151.,-100.1,-178.157162217596));
#56989=CARTESIAN_POINT('',(-94.,-100.1,-133.157162217596));
#56990=CARTESIAN_POINT('',(-151.,-100.1,-133.157162217596));
#56991=CARTESIAN_POINT('',(151.,-100.1,-53.1571622175961));
#56992=CARTESIAN_POINT('',(-94.,-100.1,-53.1571622175961));
#56993=CARTESIAN_POINT('',(94.,-100.1,-53.1571622175961));
#56994=CARTESIAN_POINT('',(-151.,-100.1,-53.1571622175961));
#56995=CARTESIAN_POINT('',(151.,-100.1,-8.1571622175961));
#56996=CARTESIAN_POINT('',(-94.,-100.1,-8.15716221759613));
#56997=CARTESIAN_POINT('',(94.,-100.1,-8.1571622175961));
#56998=CARTESIAN_POINT('',(-151.,-100.1,-8.15716221759613));
#56999=CARTESIAN_POINT('',(24.7487373415287,-12.7512626584704,279.));
#57000=CARTESIAN_POINT('',(-24.7487373415294,-12.7512626584712,279.));
#57001=CARTESIAN_POINT('',(-24.7487373415285,-62.2487373415293,279.));
#57002=UNCERTAINTY_MEASURE_WITH_UNIT(LENGTH_MEASURE(0.01),#57080,
'DISTANCE_ACCURACY_VALUE',
'Maximum model space distance between geometric entities at asserted c
onnectivities');
#57003=UNCERTAINTY_MEASURE_WITH_UNIT(LENGTH_MEASURE(0.01),#57080,
'DISTANCE_ACCURACY_VALUE',
'Maximum model space distance between geometric entities at asserted c
onnectivities');
#57004=UNCERTAINTY_MEASURE_WITH_UNIT(LENGTH_MEASURE(0.01),#57080,
'DISTANCE_ACCURACY_VALUE',
'Maximum model space distance between geometric entities at asserted c
onnectivities');
#57005=UNCERTAINTY_MEASURE_WITH_UNIT(LENGTH_MEASURE(0.01),#57080,
'DISTANCE_ACCURACY_VALUE',
'Maximum model space distance between geometric entities at asserted c
onnectivities');
#57006=UNCERTAINTY_MEASURE_WITH_UNIT(LENGTH_MEASURE(0.01),#57080,
'DISTANCE_ACCURACY_VALUE',
'Maximum model space distance between geometric entities at asserted c
onnectivities');
#57007=UNCERTAINTY_MEASURE_WITH_UNIT(LENGTH_MEASURE(0.01),#57080,
'DISTANCE_ACCURACY_VALUE',
'Maximum model space distance between geometric entities at asserted c
onnectivities');
#57008=UNCERTAINTY_MEASURE_WITH_UNIT(LENGTH_MEASURE(0.01),#57080,
'DISTANCE_ACCURACY_VALUE',
'Maximum model space distance between geometric entities at asserted c
onnectivities');
#57009=UNCERTAINTY_MEASURE_WITH_UNIT(LENGTH_MEASURE(0.01),#57080,
'DISTANCE_ACCURACY_VALUE',
'Maximum model space distance between geometric entities at asserted c
onnectivities');
#57010=UNCERTAINTY_MEASURE_WITH_UNIT(LENGTH_MEASURE(0.01),#57080,
'DISTANCE_ACCURACY_VALUE',
'Maximum model space distance between geometric entities at asserted c
onnectivities');
#57011=UNCERTAINTY_MEASURE_WITH_UNIT(LENGTH_MEASURE(0.01),#57080,
'DISTANCE_ACCURACY_VALUE',
'Maximum model space distance between geometric entities at asserted c
onnectivities');
#57012=UNCERTAINTY_MEASURE_WITH_UNIT(LENGTH_MEASURE(0.01),#57080,
'DISTANCE_ACCURACY_VALUE',
'Maximum model space distance between geometric entities at asserted c
onnectivities');
#57013=UNCERTAINTY_MEASURE_WITH_UNIT(LENGTH_MEASURE(0.01),#57080,
'DISTANCE_ACCURACY_VALUE',
'Maximum model space distance between geometric entities at asserted c
onnectivities');
#57014=UNCERTAINTY_MEASURE_WITH_UNIT(LENGTH_MEASURE(0.01),#57080,
'DISTANCE_ACCURACY_VALUE',
'Maximum model space distance between geometric entities at asserted c
onnectivities');
#57015=UNCERTAINTY_MEASURE_WITH_UNIT(LENGTH_MEASURE(0.01),#57080,
'DISTANCE_ACCURACY_VALUE',
'Maximum model space distance between geometric entities at asserted c
onnectivities');
#57016=UNCERTAINTY_MEASURE_WITH_UNIT(LENGTH_MEASURE(0.01),#57080,
'DISTANCE_ACCURACY_VALUE',
'Maximum model space distance between geometric entities at asserted c
onnectivities');
#57017=UNCERTAINTY_MEASURE_WITH_UNIT(LENGTH_MEASURE(0.01),#57080,
'DISTANCE_ACCURACY_VALUE',
'Maximum model space distance between geometric entities at asserted c
onnectivities');
#57018=UNCERTAINTY_MEASURE_WITH_UNIT(LENGTH_MEASURE(0.01),#57080,
'DISTANCE_ACCURACY_VALUE',
'Maximum model space distance between geometric entities at asserted c
onnectivities');
#57019=UNCERTAINTY_MEASURE_WITH_UNIT(LENGTH_MEASURE(0.01),#57080,
'DISTANCE_ACCURACY_VALUE',
'Maximum model space distance between geometric entities at asserted c
onnectivities');
#57020=UNCERTAINTY_MEASURE_WITH_UNIT(LENGTH_MEASURE(0.01),#57080,
'DISTANCE_ACCURACY_VALUE',
'Maximum model space distance between geometric entities at asserted c
onnectivities');
#57021=UNCERTAINTY_MEASURE_WITH_UNIT(LENGTH_MEASURE(0.01),#57080,
'DISTANCE_ACCURACY_VALUE',
'Maximum model space distance between geometric entities at asserted c
onnectivities');
#57022=UNCERTAINTY_MEASURE_WITH_UNIT(LENGTH_MEASURE(0.01),#57080,
'DISTANCE_ACCURACY_VALUE',
'Maximum model space distance between geometric entities at asserted c
onnectivities');
#57023=UNCERTAINTY_MEASURE_WITH_UNIT(LENGTH_MEASURE(0.01),#57080,
'DISTANCE_ACCURACY_VALUE',
'Maximum model space distance between geometric entities at asserted c
onnectivities');
#57024=UNCERTAINTY_MEASURE_WITH_UNIT(LENGTH_MEASURE(0.01),#57080,
'DISTANCE_ACCURACY_VALUE',
'Maximum model space distance between geometric entities at asserted c
onnectivities');
#57025=UNCERTAINTY_MEASURE_WITH_UNIT(LENGTH_MEASURE(0.01),#57080,
'DISTANCE_ACCURACY_VALUE',
'Maximum model space distance between geometric entities at asserted c
onnectivities');
#57026=UNCERTAINTY_MEASURE_WITH_UNIT(LENGTH_MEASURE(0.01),#57080,
'DISTANCE_ACCURACY_VALUE',
'Maximum model space distance between geometric entities at asserted c
onnectivities');
#57027=UNCERTAINTY_MEASURE_WITH_UNIT(LENGTH_MEASURE(0.01),#57080,
'DISTANCE_ACCURACY_VALUE',
'Maximum model space distance between geometric entities at asserted c
onnectivities');
#57028=UNCERTAINTY_MEASURE_WITH_UNIT(LENGTH_MEASURE(0.01),#57080,
'DISTANCE_ACCURACY_VALUE',
'Maximum model space distance between geometric entities at asserted c
onnectivities');
#57029=UNCERTAINTY_MEASURE_WITH_UNIT(LENGTH_MEASURE(0.01),#57080,
'DISTANCE_ACCURACY_VALUE',
'Maximum model space distance between geometric entities at asserted c
onnectivities');
#57030=UNCERTAINTY_MEASURE_WITH_UNIT(LENGTH_MEASURE(0.01),#57080,
'DISTANCE_ACCURACY_VALUE',
'Maximum model space distance between geometric entities at asserted c
onnectivities');
#57031=UNCERTAINTY_MEASURE_WITH_UNIT(LENGTH_MEASURE(0.01),#57080,
'DISTANCE_ACCURACY_VALUE',
'Maximum model space distance between geometric entities at asserted c
onnectivities');
#57032=UNCERTAINTY_MEASURE_WITH_UNIT(LENGTH_MEASURE(0.01),#57080,
'DISTANCE_ACCURACY_VALUE',
'Maximum model space distance between geometric entities at asserted c
onnectivities');
#57033=UNCERTAINTY_MEASURE_WITH_UNIT(LENGTH_MEASURE(0.01),#57080,
'DISTANCE_ACCURACY_VALUE',
'Maximum model space distance between geometric entities at asserted c
onnectivities');
#57034=UNCERTAINTY_MEASURE_WITH_UNIT(LENGTH_MEASURE(0.01),#57080,
'DISTANCE_ACCURACY_VALUE',
'Maximum model space distance between geometric entities at asserted c
onnectivities');
#57035=UNCERTAINTY_MEASURE_WITH_UNIT(LENGTH_MEASURE(0.01),#57080,
'DISTANCE_ACCURACY_VALUE',
'Maximum model space distance between geometric entities at asserted c
onnectivities');
#57036=UNCERTAINTY_MEASURE_WITH_UNIT(LENGTH_MEASURE(0.01),#57080,
'DISTANCE_ACCURACY_VALUE',
'Maximum model space distance between geometric entities at asserted c
onnectivities');
#57037=UNCERTAINTY_MEASURE_WITH_UNIT(LENGTH_MEASURE(0.01),#57080,
'DISTANCE_ACCURACY_VALUE',
'Maximum model space distance between geometric entities at asserted c
onnectivities');
#57038=UNCERTAINTY_MEASURE_WITH_UNIT(LENGTH_MEASURE(0.01),#57080,
'DISTANCE_ACCURACY_VALUE',
'Maximum model space distance between geometric entities at asserted c
onnectivities');
#57039=UNCERTAINTY_MEASURE_WITH_UNIT(LENGTH_MEASURE(0.01),#57080,
'DISTANCE_ACCURACY_VALUE',
'Maximum model space distance between geometric entities at asserted c
onnectivities');
#57040=UNCERTAINTY_MEASURE_WITH_UNIT(LENGTH_MEASURE(0.01),#57080,
'DISTANCE_ACCURACY_VALUE',
'Maximum model space distance between geometric entities at asserted c
onnectivities');
#57041=(
GEOMETRIC_REPRESENTATION_CONTEXT(3)
GLOBAL_UNCERTAINTY_ASSIGNED_CONTEXT((#57002))
GLOBAL_UNIT_ASSIGNED_CONTEXT((#57080,#57082,#57083))
REPRESENTATION_CONTEXT('','3D')
);
#57042=(
GEOMETRIC_REPRESENTATION_CONTEXT(3)
GLOBAL_UNCERTAINTY_ASSIGNED_CONTEXT((#57003))
GLOBAL_UNIT_ASSIGNED_CONTEXT((#57080,#57082,#57083))
REPRESENTATION_CONTEXT('','3D')
);
#57043=(
GEOMETRIC_REPRESENTATION_CONTEXT(3)
GLOBAL_UNCERTAINTY_ASSIGNED_CONTEXT((#57004))
GLOBAL_UNIT_ASSIGNED_CONTEXT((#57080,#57082,#57083))
REPRESENTATION_CONTEXT('','3D')
);
#57044=(
GEOMETRIC_REPRESENTATION_CONTEXT(3)
GLOBAL_UNCERTAINTY_ASSIGNED_CONTEXT((#57005))
GLOBAL_UNIT_ASSIGNED_CONTEXT((#57080,#57082,#57083))
REPRESENTATION_CONTEXT('','3D')
);
#57045=(
GEOMETRIC_REPRESENTATION_CONTEXT(3)
GLOBAL_UNCERTAINTY_ASSIGNED_CONTEXT((#57006))
GLOBAL_UNIT_ASSIGNED_CONTEXT((#57080,#57082,#57083))
REPRESENTATION_CONTEXT('','3D')
);
#57046=(
GEOMETRIC_REPRESENTATION_CONTEXT(3)
GLOBAL_UNCERTAINTY_ASSIGNED_CONTEXT((#57007))
GLOBAL_UNIT_ASSIGNED_CONTEXT((#57080,#57082,#57083))
REPRESENTATION_CONTEXT('','3D')
);
#57047=(
GEOMETRIC_REPRESENTATION_CONTEXT(3)
GLOBAL_UNCERTAINTY_ASSIGNED_CONTEXT((#57008))
GLOBAL_UNIT_ASSIGNED_CONTEXT((#57080,#57082,#57083))
REPRESENTATION_CONTEXT('','3D')
);
#57048=(
GEOMETRIC_REPRESENTATION_CONTEXT(3)
GLOBAL_UNCERTAINTY_ASSIGNED_CONTEXT((#57009))
GLOBAL_UNIT_ASSIGNED_CONTEXT((#57080,#57082,#57083))
REPRESENTATION_CONTEXT('','3D')
);
#57049=(
GEOMETRIC_REPRESENTATION_CONTEXT(3)
GLOBAL_UNCERTAINTY_ASSIGNED_CONTEXT((#57010))
GLOBAL_UNIT_ASSIGNED_CONTEXT((#57080,#57082,#57083))
REPRESENTATION_CONTEXT('','3D')
);
#57050=(
GEOMETRIC_REPRESENTATION_CONTEXT(3)
GLOBAL_UNCERTAINTY_ASSIGNED_CONTEXT((#57011))
GLOBAL_UNIT_ASSIGNED_CONTEXT((#57080,#57082,#57083))
REPRESENTATION_CONTEXT('','3D')
);
#57051=(
GEOMETRIC_REPRESENTATION_CONTEXT(3)
GLOBAL_UNCERTAINTY_ASSIGNED_CONTEXT((#57012))
GLOBAL_UNIT_ASSIGNED_CONTEXT((#57080,#57082,#57083))
REPRESENTATION_CONTEXT('','3D')
);
#57052=(
GEOMETRIC_REPRESENTATION_CONTEXT(3)
GLOBAL_UNCERTAINTY_ASSIGNED_CONTEXT((#57013))
GLOBAL_UNIT_ASSIGNED_CONTEXT((#57080,#57082,#57083))
REPRESENTATION_CONTEXT('','3D')
);
#57053=(
GEOMETRIC_REPRESENTATION_CONTEXT(3)
GLOBAL_UNCERTAINTY_ASSIGNED_CONTEXT((#57014))
GLOBAL_UNIT_ASSIGNED_CONTEXT((#57080,#57082,#57083))
REPRESENTATION_CONTEXT('','3D')
);
#57054=(
GEOMETRIC_REPRESENTATION_CONTEXT(3)
GLOBAL_UNCERTAINTY_ASSIGNED_CONTEXT((#57015))
GLOBAL_UNIT_ASSIGNED_CONTEXT((#57080,#57082,#57083))
REPRESENTATION_CONTEXT('','3D')
);
#57055=(
GEOMETRIC_REPRESENTATION_CONTEXT(3)
GLOBAL_UNCERTAINTY_ASSIGNED_CONTEXT((#57016))
GLOBAL_UNIT_ASSIGNED_CONTEXT((#57080,#57082,#57083))
REPRESENTATION_CONTEXT('','3D')
);
#57056=(
GEOMETRIC_REPRESENTATION_CONTEXT(3)
GLOBAL_UNCERTAINTY_ASSIGNED_CONTEXT((#57017))
GLOBAL_UNIT_ASSIGNED_CONTEXT((#57080,#57082,#57083))
REPRESENTATION_CONTEXT('','3D')
);
#57057=(
GEOMETRIC_REPRESENTATION_CONTEXT(3)
GLOBAL_UNCERTAINTY_ASSIGNED_CONTEXT((#57018))
GLOBAL_UNIT_ASSIGNED_CONTEXT((#57080,#57082,#57083))
REPRESENTATION_CONTEXT('','3D')
);
#57058=(
GEOMETRIC_REPRESENTATION_CONTEXT(3)
GLOBAL_UNCERTAINTY_ASSIGNED_CONTEXT((#57019))
GLOBAL_UNIT_ASSIGNED_CONTEXT((#57080,#57082,#57083))
REPRESENTATION_CONTEXT('','3D')
);
#57059=(
GEOMETRIC_REPRESENTATION_CONTEXT(3)
GLOBAL_UNCERTAINTY_ASSIGNED_CONTEXT((#57020))
GLOBAL_UNIT_ASSIGNED_CONTEXT((#57080,#57082,#57083))
REPRESENTATION_CONTEXT('','3D')
);
#57060=(
GEOMETRIC_REPRESENTATION_CONTEXT(3)
GLOBAL_UNCERTAINTY_ASSIGNED_CONTEXT((#57021))
GLOBAL_UNIT_ASSIGNED_CONTEXT((#57080,#57082,#57083))
REPRESENTATION_CONTEXT('','3D')
);
#57061=(
GEOMETRIC_REPRESENTATION_CONTEXT(3)
GLOBAL_UNCERTAINTY_ASSIGNED_CONTEXT((#57022))
GLOBAL_UNIT_ASSIGNED_CONTEXT((#57080,#57082,#57083))
REPRESENTATION_CONTEXT('','3D')
);
#57062=(
GEOMETRIC_REPRESENTATION_CONTEXT(3)
GLOBAL_UNCERTAINTY_ASSIGNED_CONTEXT((#57023))
GLOBAL_UNIT_ASSIGNED_CONTEXT((#57080,#57082,#57083))
REPRESENTATION_CONTEXT('','3D')
);
#57063=(
GEOMETRIC_REPRESENTATION_CONTEXT(3)
GLOBAL_UNCERTAINTY_ASSIGNED_CONTEXT((#57024))
GLOBAL_UNIT_ASSIGNED_CONTEXT((#57080,#57082,#57083))
REPRESENTATION_CONTEXT('','3D')
);
#57064=(
GEOMETRIC_REPRESENTATION_CONTEXT(3)
GLOBAL_UNCERTAINTY_ASSIGNED_CONTEXT((#57025))
GLOBAL_UNIT_ASSIGNED_CONTEXT((#57080,#57082,#57083))
REPRESENTATION_CONTEXT('','3D')
);
#57065=(
GEOMETRIC_REPRESENTATION_CONTEXT(3)
GLOBAL_UNCERTAINTY_ASSIGNED_CONTEXT((#57026))
GLOBAL_UNIT_ASSIGNED_CONTEXT((#57080,#57082,#57083))
REPRESENTATION_CONTEXT('','3D')
);
#57066=(
GEOMETRIC_REPRESENTATION_CONTEXT(3)
GLOBAL_UNCERTAINTY_ASSIGNED_CONTEXT((#57027))
GLOBAL_UNIT_ASSIGNED_CONTEXT((#57080,#57082,#57083))
REPRESENTATION_CONTEXT('','3D')
);
#57067=(
GEOMETRIC_REPRESENTATION_CONTEXT(3)
GLOBAL_UNCERTAINTY_ASSIGNED_CONTEXT((#57028))
GLOBAL_UNIT_ASSIGNED_CONTEXT((#57080,#57082,#57083))
REPRESENTATION_CONTEXT('','3D')
);
#57068=(
GEOMETRIC_REPRESENTATION_CONTEXT(3)
GLOBAL_UNCERTAINTY_ASSIGNED_CONTEXT((#57029))
GLOBAL_UNIT_ASSIGNED_CONTEXT((#57080,#57082,#57083))
REPRESENTATION_CONTEXT('','3D')
);
#57069=(
GEOMETRIC_REPRESENTATION_CONTEXT(3)
GLOBAL_UNCERTAINTY_ASSIGNED_CONTEXT((#57030))
GLOBAL_UNIT_ASSIGNED_CONTEXT((#57080,#57082,#57083))
REPRESENTATION_CONTEXT('','3D')
);
#57070=(
GEOMETRIC_REPRESENTATION_CONTEXT(3)
GLOBAL_UNCERTAINTY_ASSIGNED_CONTEXT((#57031))
GLOBAL_UNIT_ASSIGNED_CONTEXT((#57080,#57082,#57083))
REPRESENTATION_CONTEXT('','3D')
);
#57071=(
GEOMETRIC_REPRESENTATION_CONTEXT(3)
GLOBAL_UNCERTAINTY_ASSIGNED_CONTEXT((#57032))
GLOBAL_UNIT_ASSIGNED_CONTEXT((#57080,#57082,#57083))
REPRESENTATION_CONTEXT('','3D')
);
#57072=(
GEOMETRIC_REPRESENTATION_CONTEXT(3)
GLOBAL_UNCERTAINTY_ASSIGNED_CONTEXT((#57033))
GLOBAL_UNIT_ASSIGNED_CONTEXT((#57080,#57082,#57083))
REPRESENTATION_CONTEXT('','3D')
);
#57073=(
GEOMETRIC_REPRESENTATION_CONTEXT(3)
GLOBAL_UNCERTAINTY_ASSIGNED_CONTEXT((#57034))
GLOBAL_UNIT_ASSIGNED_CONTEXT((#57080,#57082,#57083))
REPRESENTATION_CONTEXT('','3D')
);
#57074=(
GEOMETRIC_REPRESENTATION_CONTEXT(3)
GLOBAL_UNCERTAINTY_ASSIGNED_CONTEXT((#57035))
GLOBAL_UNIT_ASSIGNED_CONTEXT((#57080,#57082,#57083))
REPRESENTATION_CONTEXT('','3D')
);
#57075=(
GEOMETRIC_REPRESENTATION_CONTEXT(3)
GLOBAL_UNCERTAINTY_ASSIGNED_CONTEXT((#57036))
GLOBAL_UNIT_ASSIGNED_CONTEXT((#57080,#57082,#57083))
REPRESENTATION_CONTEXT('','3D')
);
#57076=(
GEOMETRIC_REPRESENTATION_CONTEXT(3)
GLOBAL_UNCERTAINTY_ASSIGNED_CONTEXT((#57037))
GLOBAL_UNIT_ASSIGNED_CONTEXT((#57080,#57082,#57083))
REPRESENTATION_CONTEXT('','3D')
);
#57077=(
GEOMETRIC_REPRESENTATION_CONTEXT(3)
GLOBAL_UNCERTAINTY_ASSIGNED_CONTEXT((#57038))
GLOBAL_UNIT_ASSIGNED_CONTEXT((#57080,#57082,#57083))
REPRESENTATION_CONTEXT('','3D')
);
#57078=(
GEOMETRIC_REPRESENTATION_CONTEXT(3)
GLOBAL_UNCERTAINTY_ASSIGNED_CONTEXT((#57039))
GLOBAL_UNIT_ASSIGNED_CONTEXT((#57080,#57082,#57083))
REPRESENTATION_CONTEXT('','3D')
);
#57079=(
GEOMETRIC_REPRESENTATION_CONTEXT(3)
GLOBAL_UNCERTAINTY_ASSIGNED_CONTEXT((#57040))
GLOBAL_UNIT_ASSIGNED_CONTEXT((#57080,#57082,#57083))
REPRESENTATION_CONTEXT('','3D')
);
#57080=(
LENGTH_UNIT()
NAMED_UNIT(*)
SI_UNIT(.MILLI.,.METRE.)
);
#57081=(
LENGTH_UNIT()
NAMED_UNIT(*)
SI_UNIT($,.METRE.)
);
#57082=(
NAMED_UNIT(*)
PLANE_ANGLE_UNIT()
SI_UNIT($,.RADIAN.)
);
#57083=(
NAMED_UNIT(*)
SI_UNIT($,.STERADIAN.)
SOLID_ANGLE_UNIT()
);
#57084=SHAPE_DEFINITION_REPRESENTATION(#57122,#57249);
#57085=SHAPE_DEFINITION_REPRESENTATION(#57123,#57250);
#57086=SHAPE_DEFINITION_REPRESENTATION(#57124,#57251);
#57087=SHAPE_DEFINITION_REPRESENTATION(#57125,#57252);
#57088=SHAPE_DEFINITION_REPRESENTATION(#57126,#57253);
#57089=SHAPE_DEFINITION_REPRESENTATION(#57127,#57254);
#57090=SHAPE_DEFINITION_REPRESENTATION(#57130,#57255);
#57091=SHAPE_DEFINITION_REPRESENTATION(#57131,#57256);
#57092=SHAPE_DEFINITION_REPRESENTATION(#57132,#57257);
#57093=SHAPE_DEFINITION_REPRESENTATION(#57133,#57258);
#57094=SHAPE_DEFINITION_REPRESENTATION(#57138,#57259);
#57095=SHAPE_DEFINITION_REPRESENTATION(#57139,#57260);
#57096=SHAPE_DEFINITION_REPRESENTATION(#57140,#57261);
#57097=SHAPE_DEFINITION_REPRESENTATION(#57143,#57262);
#57098=SHAPE_DEFINITION_REPRESENTATION(#57144,#57263);
#57099=SHAPE_DEFINITION_REPRESENTATION(#57145,#57264);
#57100=SHAPE_DEFINITION_REPRESENTATION(#57146,#57265);
#57101=SHAPE_DEFINITION_REPRESENTATION(#57147,#57266);
#57102=SHAPE_DEFINITION_REPRESENTATION(#57148,#57267);
#57103=SHAPE_DEFINITION_REPRESENTATION(#57149,#57268);
#57104=SHAPE_DEFINITION_REPRESENTATION(#57150,#57269);
#57105=SHAPE_DEFINITION_REPRESENTATION(#57151,#57270);
#57106=SHAPE_DEFINITION_REPRESENTATION(#57152,#57271);
#57107=SHAPE_DEFINITION_REPRESENTATION(#57159,#57272);
#57108=SHAPE_DEFINITION_REPRESENTATION(#57160,#57273);
#57109=SHAPE_DEFINITION_REPRESENTATION(#57161,#57274);
#57110=SHAPE_DEFINITION_REPRESENTATION(#57164,#57275);
#57111=SHAPE_DEFINITION_REPRESENTATION(#57165,#57276);
#57112=SHAPE_DEFINITION_REPRESENTATION(#57166,#57277);
#57113=SHAPE_DEFINITION_REPRESENTATION(#57167,#57278);
#57114=SHAPE_DEFINITION_REPRESENTATION(#57168,#57279);
#57115=SHAPE_DEFINITION_REPRESENTATION(#57169,#57280);
#57116=SHAPE_DEFINITION_REPRESENTATION(#57180,#57281);
#57117=SHAPE_DEFINITION_REPRESENTATION(#57181,#57282);
#57118=SHAPE_DEFINITION_REPRESENTATION(#57182,#57283);
#57119=SHAPE_DEFINITION_REPRESENTATION(#57183,#57284);
#57120=SHAPE_DEFINITION_REPRESENTATION(#57184,#57285);
#57121=SHAPE_DEFINITION_REPRESENTATION(#57185,#57286);
#57122=PRODUCT_DEFINITION_SHAPE('',$,#57288);
#57123=PRODUCT_DEFINITION_SHAPE('',$,#57289);
#57124=PRODUCT_DEFINITION_SHAPE('',$,#57290);
#57125=PRODUCT_DEFINITION_SHAPE('',$,#57291);
#57126=PRODUCT_DEFINITION_SHAPE('',$,#57292);
#57127=PRODUCT_DEFINITION_SHAPE('',$,#57293);
#57128=PRODUCT_DEFINITION_SHAPE($,$,#547);
#57129=PRODUCT_DEFINITION_SHAPE($,$,#548);
#57130=PRODUCT_DEFINITION_SHAPE('',$,#57294);
#57131=PRODUCT_DEFINITION_SHAPE('',$,#57295);
#57132=PRODUCT_DEFINITION_SHAPE('',$,#57296);
#57133=PRODUCT_DEFINITION_SHAPE('',$,#57297);
#57134=PRODUCT_DEFINITION_SHAPE($,$,#549);
#57135=PRODUCT_DEFINITION_SHAPE($,$,#550);
#57136=PRODUCT_DEFINITION_SHAPE($,$,#551);
#57137=PRODUCT_DEFINITION_SHAPE($,$,#552);
#57138=PRODUCT_DEFINITION_SHAPE('',$,#57298);
#57139=PRODUCT_DEFINITION_SHAPE('',$,#57299);
#57140=PRODUCT_DEFINITION_SHAPE('',$,#57300);
#57141=PRODUCT_DEFINITION_SHAPE($,$,#553);
#57142=PRODUCT_DEFINITION_SHAPE($,$,#554);
#57143=PRODUCT_DEFINITION_SHAPE('',$,#57301);
#57144=PRODUCT_DEFINITION_SHAPE('',$,#57302);
#57145=PRODUCT_DEFINITION_SHAPE('',$,#57303);
#57146=PRODUCT_DEFINITION_SHAPE('',$,#57304);
#57147=PRODUCT_DEFINITION_SHAPE('',$,#57305);
#57148=PRODUCT_DEFINITION_SHAPE('',$,#57306);
#57149=PRODUCT_DEFINITION_SHAPE('',$,#57307);
#57150=PRODUCT_DEFINITION_SHAPE('',$,#57308);
#57151=PRODUCT_DEFINITION_SHAPE('',$,#57309);
#57152=PRODUCT_DEFINITION_SHAPE('',$,#57310);
#57153=PRODUCT_DEFINITION_SHAPE($,$,#555);
#57154=PRODUCT_DEFINITION_SHAPE($,$,#556);
#57155=PRODUCT_DEFINITION_SHAPE($,$,#557);
#57156=PRODUCT_DEFINITION_SHAPE($,$,#558);
#57157=PRODUCT_DEFINITION_SHAPE($,$,#559);
#57158=PRODUCT_DEFINITION_SHAPE($,$,#560);
#57159=PRODUCT_DEFINITION_SHAPE('',$,#57311);
#57160=PRODUCT_DEFINITION_SHAPE('',$,#57312);
#57161=PRODUCT_DEFINITION_SHAPE('',$,#57313);
#57162=PRODUCT_DEFINITION_SHAPE($,$,#561);
#57163=PRODUCT_DEFINITION_SHAPE($,$,#562);
#57164=PRODUCT_DEFINITION_SHAPE('',$,#57314);
#57165=PRODUCT_DEFINITION_SHAPE('',$,#57315);
#57166=PRODUCT_DEFINITION_SHAPE('',$,#57316);
#57167=PRODUCT_DEFINITION_SHAPE('',$,#57317);
#57168=PRODUCT_DEFINITION_SHAPE('',$,#57318);
#57169=PRODUCT_DEFINITION_SHAPE('',$,#57319);
#57170=PRODUCT_DEFINITION_SHAPE($,$,#563);
#57171=PRODUCT_DEFINITION_SHAPE($,$,#564);
#57172=PRODUCT_DEFINITION_SHAPE($,$,#565);
#57173=PRODUCT_DEFINITION_SHAPE($,$,#566);
#57174=PRODUCT_DEFINITION_SHAPE($,$,#567);
#57175=PRODUCT_DEFINITION_SHAPE($,$,#568);
#57176=PRODUCT_DEFINITION_SHAPE($,$,#569);
#57177=PRODUCT_DEFINITION_SHAPE($,$,#570);
#57178=PRODUCT_DEFINITION_SHAPE($,$,#571);
#57179=PRODUCT_DEFINITION_SHAPE($,$,#572);
#57180=PRODUCT_DEFINITION_SHAPE('',$,#57320);
#57181=PRODUCT_DEFINITION_SHAPE('',$,#57321);
#57182=PRODUCT_DEFINITION_SHAPE('',$,#57322);
#57183=PRODUCT_DEFINITION_SHAPE('',$,#57323);
#57184=PRODUCT_DEFINITION_SHAPE('',$,#57324);
#57185=PRODUCT_DEFINITION_SHAPE('',$,#57325);
#57186=PRODUCT_DEFINITION_SHAPE($,$,#573);
#57187=PRODUCT_DEFINITION_SHAPE($,$,#574);
#57188=PRODUCT_DEFINITION_SHAPE($,$,#575);
#57189=PRODUCT_DEFINITION_SHAPE($,$,#576);
#57190=PRODUCT_DEFINITION_SHAPE($,$,#577);
#57191=PRODUCT_DEFINITION_SHAPE($,$,#578);
#57192=PRODUCT_DEFINITION_SHAPE($,$,#579);
#57193=PRODUCT_DEFINITION_SHAPE($,$,#580);
#57194=PRODUCT_DEFINITION_SHAPE($,$,#581);
#57195=PRODUCT_DEFINITION_SHAPE($,$,#582);
#57196=PRODUCT_DEFINITION_SHAPE($,$,#583);
#57197=PRODUCT_DEFINITION_SHAPE($,$,#584);
#57198=PRODUCT_DEFINITION_SHAPE($,$,#585);
#57199=PRODUCT_DEFINITION_SHAPE($,$,#586);
#57200=PRODUCT_DEFINITION_SHAPE($,$,#587);
#57201=PRODUCT_DEFINITION_SHAPE($,$,#588);
#57202=PRODUCT_DEFINITION_SHAPE($,$,#589);
#57203=PRODUCT_DEFINITION_SHAPE($,$,#590);
#57204=PRODUCT_DEFINITION_SHAPE($,$,#591);
#57205=PRODUCT_DEFINITION_SHAPE($,$,#592);
#57206=PRODUCT_DEFINITION_SHAPE($,$,#593);
#57207=PRODUCT_DEFINITION_SHAPE($,$,#594);
#57208=PRODUCT_DEFINITION_SHAPE($,$,#595);
#57209=PRODUCT_DEFINITION_SHAPE($,$,#596);
#57210=PRODUCT_DEFINITION_SHAPE($,$,#597);
#57211=PRODUCT_DEFINITION_SHAPE($,$,#598);
#57212=PRODUCT_DEFINITION_SHAPE($,$,#599);
#57213=PRODUCT_DEFINITION_SHAPE($,$,#600);
#57214=PRODUCT_DEFINITION_SHAPE($,$,#601);
#57215=PRODUCT_DEFINITION_SHAPE($,$,#602);
#57216=PRODUCT_DEFINITION_SHAPE($,$,#603);
#57217=PRODUCT_DEFINITION_SHAPE($,$,#604);
#57218=PRODUCT_DEFINITION_SHAPE($,$,#605);
#57219=PRODUCT_DEFINITION_SHAPE($,$,#606);
#57220=PRODUCT_DEFINITION_SHAPE($,$,#607);
#57221=PRODUCT_DEFINITION_SHAPE($,$,#608);
#57222=PRODUCT_DEFINITION_SHAPE($,$,#609);
#57223=PRODUCT_DEFINITION_SHAPE($,$,#610);
#57224=PRODUCT_DEFINITION_SHAPE($,$,#611);
#57225=PRODUCT_DEFINITION_SHAPE($,$,#612);
#57226=PRODUCT_DEFINITION_SHAPE($,$,#613);
#57227=PRODUCT_DEFINITION_SHAPE($,$,#614);
#57228=PRODUCT_DEFINITION_SHAPE($,$,#615);
#57229=PRODUCT_DEFINITION_SHAPE($,$,#616);
#57230=PRODUCT_DEFINITION_SHAPE($,$,#617);
#57231=PRODUCT_DEFINITION_SHAPE($,$,#618);
#57232=PRODUCT_DEFINITION_SHAPE($,$,#619);
#57233=PRODUCT_DEFINITION_SHAPE($,$,#620);
#57234=PRODUCT_DEFINITION_SHAPE($,$,#621);
#57235=PRODUCT_DEFINITION_SHAPE($,$,#622);
#57236=PRODUCT_DEFINITION_SHAPE($,$,#623);
#57237=PRODUCT_DEFINITION_SHAPE($,$,#624);
#57238=PRODUCT_DEFINITION_SHAPE($,$,#625);
#57239=PRODUCT_DEFINITION_SHAPE($,$,#626);
#57240=PRODUCT_DEFINITION_SHAPE($,$,#627);
#57241=PRODUCT_DEFINITION_SHAPE($,$,#628);
#57242=PRODUCT_DEFINITION_SHAPE($,$,#629);
#57243=PRODUCT_DEFINITION_SHAPE($,$,#630);
#57244=PRODUCT_DEFINITION_SHAPE($,$,#631);
#57245=PRODUCT_DEFINITION_SHAPE($,$,#632);
#57246=PRODUCT_DEFINITION_SHAPE($,$,#633);
#57247=PRODUCT_DEFINITION_SHAPE($,$,#634);
#57248=PRODUCT_DEFINITION_SHAPE($,$,#635);
#57249=SHAPE_REPRESENTATION('',(#24883,#27414,#27415,#27416,#27417,#27418,
#27419,#27420,#27421,#27422,#27423,#27424,#27425,#27426,#27427,#27428,#27429,
#27430,#27431,#27432,#27433,#27434,#27435,#27436,#27437,#27438,#27439,#27440,
#27441,#27442,#27443,#27444,#27445,#27446,#27447,#27448,#27449,#27450,#27451,
#27452,#27453,#27454,#27455,#27456,#27457,#27458,#27459,#27460,#27461,#27462,
#27463,#27464,#27465,#27466,#27467,#27468,#27469,#27470,#27471,#27472,#27473,
#27474,#27475,#27476),#57041);
#57250=SHAPE_REPRESENTATION('',(#24884),#57042);
#57251=SHAPE_REPRESENTATION('',(#24935,#27179,#27180,#27181,#27182,#27183),
#57043);
#57252=SHAPE_REPRESENTATION('',(#24936,#25054,#25055),#57044);
#57253=SHAPE_REPRESENTATION('',(#24937),#57045);
#57254=SHAPE_REPRESENTATION('',(#24990),#57046);
#57255=SHAPE_REPRESENTATION('',(#25056,#25272,#25273,#25274,#25275),#57047);
#57256=SHAPE_REPRESENTATION('',(#25057),#57048);
#57257=SHAPE_REPRESENTATION('',(#25214),#57049);
#57258=SHAPE_REPRESENTATION('',(#25263),#57050);
#57259=SHAPE_REPRESENTATION('',(#25276,#25370,#25371),#57051);
#57260=SHAPE_REPRESENTATION('',(#25277),#57052);
#57261=SHAPE_REPRESENTATION('',(#25337),#57053);
#57262=SHAPE_REPRESENTATION('',(#25372),#57054);
#57263=SHAPE_REPRESENTATION('',(#25397),#57055);
#57264=SHAPE_REPRESENTATION('',(#25422),#57056);
#57265=SHAPE_REPRESENTATION('',(#25468,#25980),#57057);
#57266=SHAPE_REPRESENTATION('',(#25469,#25975,#25976,#25977,#25978,#25979),
#57058);
#57267=SHAPE_REPRESENTATION('',(#25470),#57059);
#57268=SHAPE_REPRESENTATION('',(#25644),#57060);
#57269=SHAPE_REPRESENTATION('',(#25657),#57061);
#57270=SHAPE_REPRESENTATION('',(#25807),#57062);
#57271=SHAPE_REPRESENTATION('',(#25820),#57063);
#57272=SHAPE_REPRESENTATION('',(#25981,#26041,#26042),#57064);
#57273=SHAPE_REPRESENTATION('',(#25982),#57065);
#57274=SHAPE_REPRESENTATION('',(#26016),#57066);
#57275=SHAPE_REPRESENTATION('',(#26043),#57067);
#57276=SHAPE_REPRESENTATION('',(#26068),#57068);
#57277=SHAPE_REPRESENTATION('',(#26269,#27184,#27185,#27186,#27187,#27188),
#57069);
#57278=SHAPE_REPRESENTATION('',(#26270),#57070);
#57279=SHAPE_REPRESENTATION('',(#26507),#57071);
#57280=SHAPE_REPRESENTATION('',(#27107),#57072);
#57281=SHAPE_REPRESENTATION('',(#27189),#57073);
#57282=SHAPE_REPRESENTATION('',(#27238),#57074);
#57283=SHAPE_REPRESENTATION('',(#27293),#57075);
#57284=SHAPE_REPRESENTATION('',(#27315),#57076);
#57285=SHAPE_REPRESENTATION('',(#27370),#57077);
#57286=SHAPE_REPRESENTATION('',(#27392),#57078);
#57287=PRODUCT_DEFINITION_CONTEXT('part definition',#57403,'design');
#57288=PRODUCT_DEFINITION('BALL SCREW ASSLY SET-UP 2','TAS-016',#57326,
#57287);
#57289=PRODUCT_DEFINITION('Main Plate','Main Plate',#57327,#57287);
#57290=PRODUCT_DEFINITION('Linear Guide Assembly 1',
'Linear Guide Assembly 1',#57328,#57287);
#57291=PRODUCT_DEFINITION('Ball Screw Assembly','Ball Screw Assembly',#57329,
#57287);
#57292=PRODUCT_DEFINITION('Ball Screw Shaft','Ball Screw Shaft',#57330,
#57287);
#57293=PRODUCT_DEFINITION('Ball Screw Nut','Ball Screw Nut',#57331,#57287);
#57294=PRODUCT_DEFINITION('Floating Bearing Support Assembly',
'Floating Bearing Support Assembly',#57332,#57287);
#57295=PRODUCT_DEFINITION('Floating Bearing Housing',
'Floating Bearing Housing',#57333,#57287);
#57296=PRODUCT_DEFINITION('Lock Nut','Lock Nut',#57334,#57287);
#57297=PRODUCT_DEFINITION('Collar','Collar',#57335,#57287);
#57298=PRODUCT_DEFINITION('Fixed Bearing Support Assembly',
'Fixed Bearing Support Assembly',#57336,#57287);
#57299=PRODUCT_DEFINITION('Fixed Bearing Housing',
'Fixed Bearing Housing',#57337,#57287);
#57300=PRODUCT_DEFINITION('Washer','Washer',#57338,#57287);
#57301=PRODUCT_DEFINITION('Ball Screw Spacer 1','Ball Screw Spacer 1',#57339,
#57287);
#57302=PRODUCT_DEFINITION('Ball Screw Spacer 2','Ball Screw Spacer 2',#57340,
#57287);
#57303=PRODUCT_DEFINITION('Motor Mount Plate','Motor Mount Plate',#57341,
#57287);
#57304=PRODUCT_DEFINITION('Coupling Assembly','Coupling Assembly',#57342,
#57287);
#57305=PRODUCT_DEFINITION('Coupling Components','Coupling Components',#57343,
#57287);
#57306=PRODUCT_DEFINITION('Coupling Spider','Coupling Spider',#57344,#57287);
#57307=PRODUCT_DEFINITION('Coupling Set Screw 1','Coupling Set Screw 1',
#57345,#57287);
#57308=PRODUCT_DEFINITION('Coupling Hub 1','Coupling Hub 1',#57346,#57287);
#57309=PRODUCT_DEFINITION('Coupling Set Screw 2','Coupling Set Screw 2',
#57347,#57287);
#57310=PRODUCT_DEFINITION('Coupling Hub 2','Coupling Hub 2',#57348,#57287);
#57311=PRODUCT_DEFINITION('Ball Screw Support Assembly',
'Ball Screw Support Assembly',#57349,#57287);
#57312=PRODUCT_DEFINITION('Ball Screw Support Bracket',
'Ball Screw Support Bracket',#57350,#57287);
#57313=PRODUCT_DEFINITION('Ball Screw Support Plate',
'Ball Screw Support Plate',#57351,#57287);
#57314=PRODUCT_DEFINITION('Ball Screw Support Spacer',
'Ball Screw Support Spacer',#57352,#57287);
#57315=PRODUCT_DEFINITION('Motor Mount Bracket','Motor Mount Bracket',#57353,
#57287);
#57316=PRODUCT_DEFINITION('Linear Guide Assembly 2',
'Linear Guide Assembly 2',#57354,#57287);
#57317=PRODUCT_DEFINITION('Linear Guide Rail','Linear Guide Rail',#57355,
#57287);
#57318=PRODUCT_DEFINITION('Linear Guide Slider','Linear Guide Slider',#57356,
#57287);
#57319=PRODUCT_DEFINITION('Slider End Cap','Slider End Cap',#57357,#57287);
#57320=PRODUCT_DEFINITION('Linear Guide Spacer','Linear Guide Spacer',#57358,
#57287);
#57321=PRODUCT_DEFINITION('Low Head Cap Screw M5x25',
'Low Head Cap Screw M5x25',#57359,#57287);
#57322=PRODUCT_DEFINITION('Socket head cap screw M6x25',
'Socket Head Cap Screw M6x25',#57360,#57287);
#57323=PRODUCT_DEFINITION('Low Head Cap Screw M8x45',
'Low Head Cap Screw M8x45',#57361,#57287);
#57324=PRODUCT_DEFINITION('Socket head cap screw M6x20',
'Socket Head Cap Screw M6x20',#57362,#57287);
#57325=PRODUCT_DEFINITION('Socket head cap screw M4x20',
'Socket Head Cap Screw M4x20',#57363,#57287);
#57326=PRODUCT_DEFINITION_FORMATION('',$,#57405);
#57327=PRODUCT_DEFINITION_FORMATION('',$,#57406);
#57328=PRODUCT_DEFINITION_FORMATION('',$,#57407);
#57329=PRODUCT_DEFINITION_FORMATION('',$,#57408);
#57330=PRODUCT_DEFINITION_FORMATION('',$,#57409);
#57331=PRODUCT_DEFINITION_FORMATION('',$,#57410);
#57332=PRODUCT_DEFINITION_FORMATION('',$,#57411);
#57333=PRODUCT_DEFINITION_FORMATION('',$,#57412);
#57334=PRODUCT_DEFINITION_FORMATION('',$,#57413);
#57335=PRODUCT_DEFINITION_FORMATION('',$,#57414);
#57336=PRODUCT_DEFINITION_FORMATION('',$,#57415);
#57337=PRODUCT_DEFINITION_FORMATION('',$,#57416);
#57338=PRODUCT_DEFINITION_FORMATION('',$,#57417);
#57339=PRODUCT_DEFINITION_FORMATION('',$,#57418);
#57340=PRODUCT_DEFINITION_FORMATION('',$,#57419);
#57341=PRODUCT_DEFINITION_FORMATION('',$,#57420);
#57342=PRODUCT_DEFINITION_FORMATION('',$,#57421);
#57343=PRODUCT_DEFINITION_FORMATION('',$,#57422);
#57344=PRODUCT_DEFINITION_FORMATION('',$,#57423);
#57345=PRODUCT_DEFINITION_FORMATION('',$,#57424);
#57346=PRODUCT_DEFINITION_FORMATION('',$,#57425);
#57347=PRODUCT_DEFINITION_FORMATION('',$,#57426);
#57348=PRODUCT_DEFINITION_FORMATION('',$,#57427);
#57349=PRODUCT_DEFINITION_FORMATION('',$,#57428);
#57350=PRODUCT_DEFINITION_FORMATION('',$,#57429);
#57351=PRODUCT_DEFINITION_FORMATION('',$,#57430);
#57352=PRODUCT_DEFINITION_FORMATION('',$,#57431);
#57353=PRODUCT_DEFINITION_FORMATION('',$,#57432);
#57354=PRODUCT_DEFINITION_FORMATION('',$,#57433);
#57355=PRODUCT_DEFINITION_FORMATION('',$,#57434);
#57356=PRODUCT_DEFINITION_FORMATION('',$,#57435);
#57357=PRODUCT_DEFINITION_FORMATION('',$,#57436);
#57358=PRODUCT_DEFINITION_FORMATION('',$,#57437);
#57359=PRODUCT_DEFINITION_FORMATION('',$,#57438);
#57360=PRODUCT_DEFINITION_FORMATION('',$,#57439);
#57361=PRODUCT_DEFINITION_FORMATION('',$,#57440);
#57362=PRODUCT_DEFINITION_FORMATION('',$,#57441);
#57363=PRODUCT_DEFINITION_FORMATION('',$,#57442);
#57364=PRODUCT_RELATED_PRODUCT_CATEGORY('TAS-016','TAS-016',(#57405));
#57365=PRODUCT_RELATED_PRODUCT_CATEGORY('Main Plate','Main Plate',(#57406));
#57366=PRODUCT_RELATED_PRODUCT_CATEGORY('Linear Guide Assembly 1',
'Linear Guide Assembly 1',(#57407));
#57367=PRODUCT_RELATED_PRODUCT_CATEGORY('Ball Screw Assembly',
'Ball Screw Assembly',(#57408));
#57368=PRODUCT_RELATED_PRODUCT_CATEGORY('Ball Screw Shaft',
'Ball Screw Shaft',(#57409));
#57369=PRODUCT_RELATED_PRODUCT_CATEGORY('Ball Screw Nut',
'Ball Screw Nut',(#57410));
#57370=PRODUCT_RELATED_PRODUCT_CATEGORY(
'Floating Bearing Support Assembly','Floating Bearing Support Assembly',
(#57411));
#57371=PRODUCT_RELATED_PRODUCT_CATEGORY('Floating Bearing Housing',
'Floating Bearing Housing',(#57412));
#57372=PRODUCT_RELATED_PRODUCT_CATEGORY('Lock Nut','Lock Nut',(#57413));
#57373=PRODUCT_RELATED_PRODUCT_CATEGORY('Collar','Collar',(#57414));
#57374=PRODUCT_RELATED_PRODUCT_CATEGORY(
'Fixed Bearing Support Assembly','Fixed Bearing Support Assembly',(#57415));
#57375=PRODUCT_RELATED_PRODUCT_CATEGORY('Fixed Bearing Housing',
'Fixed Bearing Housing',(#57416));
#57376=PRODUCT_RELATED_PRODUCT_CATEGORY('Washer','Washer',(#57417));
#57377=PRODUCT_RELATED_PRODUCT_CATEGORY('Ball Screw Spacer 1',
'Ball Screw Spacer 1',(#57418));
#57378=PRODUCT_RELATED_PRODUCT_CATEGORY('Ball Screw Spacer 2',
'Ball Screw Spacer 2',(#57419));
#57379=PRODUCT_RELATED_PRODUCT_CATEGORY('Motor Mount Plate',
'Motor Mount Plate',(#57420));
#57380=PRODUCT_RELATED_PRODUCT_CATEGORY('Coupling Assembly',
'Coupling Assembly',(#57421));
#57381=PRODUCT_RELATED_PRODUCT_CATEGORY('Coupling Components',
'Coupling Components',(#57422));
#57382=PRODUCT_RELATED_PRODUCT_CATEGORY('Coupling Spider',
'Coupling Spider',(#57423));
#57383=PRODUCT_RELATED_PRODUCT_CATEGORY('Coupling Set Screw 1',
'Coupling Set Screw 1',(#57424));
#57384=PRODUCT_RELATED_PRODUCT_CATEGORY('Coupling Hub 1',
'Coupling Hub 1',(#57425));
#57385=PRODUCT_RELATED_PRODUCT_CATEGORY('Coupling Set Screw 2',
'Coupling Set Screw 2',(#57426));
#57386=PRODUCT_RELATED_PRODUCT_CATEGORY('Coupling Hub 2',
'Coupling Hub 2',(#57427));
#57387=PRODUCT_RELATED_PRODUCT_CATEGORY('Ball Screw Support Assembly',
'Ball Screw Support Assembly',(#57428));
#57388=PRODUCT_RELATED_PRODUCT_CATEGORY('Ball Screw Support Bracket',
'Ball Screw Support Bracket',(#57429));
#57389=PRODUCT_RELATED_PRODUCT_CATEGORY('Ball Screw Support Plate',
'Ball Screw Support Plate',(#57430));
#57390=PRODUCT_RELATED_PRODUCT_CATEGORY('Ball Screw Support Spacer',
'Ball Screw Support Spacer',(#57431));
#57391=PRODUCT_RELATED_PRODUCT_CATEGORY('Motor Mount Bracket',
'Motor Mount Bracket',(#57432));
#57392=PRODUCT_RELATED_PRODUCT_CATEGORY('Linear Guide Assembly 2',
'Linear Guide Assembly 2',(#57433));
#57393=PRODUCT_RELATED_PRODUCT_CATEGORY('Linear Guide Rail',
'Linear Guide Rail',(#57434));
#57394=PRODUCT_RELATED_PRODUCT_CATEGORY('Linear Guide Slider',
'Linear Guide Slider',(#57435));
#57395=PRODUCT_RELATED_PRODUCT_CATEGORY('Slider End Cap',
'Slider End Cap',(#57436));
#57396=PRODUCT_RELATED_PRODUCT_CATEGORY('Linear Guide Spacer',
'Linear Guide Spacer',(#57437));
#57397=PRODUCT_RELATED_PRODUCT_CATEGORY('Low Head Cap Screw M5x25',
'Low Head Cap Screw M5x25',(#57438));
#57398=PRODUCT_RELATED_PRODUCT_CATEGORY('Socket Head Cap Screw M6x25',
'Socket Head Cap Screw M6x25',(#57439));
#57399=PRODUCT_RELATED_PRODUCT_CATEGORY('Low Head Cap Screw M8x45',
'Low Head Cap Screw M8x45',(#57440));
#57400=PRODUCT_RELATED_PRODUCT_CATEGORY('Socket Head Cap Screw M6x20',
'Socket Head Cap Screw M6x20',(#57441));
#57401=PRODUCT_RELATED_PRODUCT_CATEGORY('Socket Head Cap Screw M4x20',
'Socket Head Cap Screw M4x20',(#57442));
#57402=APPLICATION_PROTOCOL_DEFINITION('international standard',
'automotive_design',2009,#57403);
#57403=APPLICATION_CONTEXT(
'Core Data for Automotive Mechanical Design Process');
#57404=PRODUCT_CONTEXT('part definition',#57403,'mechanical');
#57405=PRODUCT('BALL SCREW ASSLY SET-UP 2','TAS-016','STEP AP214',(#57404));
#57406=PRODUCT('Main Plate','Main Plate',$,(#57404));
#57407=PRODUCT('Linear Guide Assembly 1','Linear Guide Assembly 1',$,(#57404));
#57408=PRODUCT('Ball Screw Assembly','Ball Screw Assembly',$,(#57404));
#57409=PRODUCT('Ball Screw Shaft','Ball Screw Shaft',$,(#57404));
#57410=PRODUCT('Ball Screw Nut','Ball Screw Nut',$,(#57404));
#57411=PRODUCT('Floating Bearing Support Assembly',
'Floating Bearing Support Assembly',$,(#57404));
#57412=PRODUCT('Floating Bearing Housing','Floating Bearing Housing',$,
(#57404));
#57413=PRODUCT('Lock Nut','Lock Nut',$,(#57404));
#57414=PRODUCT('Collar','Collar',$,(#57404));
#57415=PRODUCT('Fixed Bearing Support Assembly',
'Fixed Bearing Support Assembly',$,(#57404));
#57416=PRODUCT('Fixed Bearing Housing','Fixed Bearing Housing',$,(#57404));
#57417=PRODUCT('Washer','Washer',$,(#57404));
#57418=PRODUCT('Ball Screw Spacer 1','Ball Screw Spacer 1',$,(#57404));
#57419=PRODUCT('Ball Screw Spacer 2','Ball Screw Spacer 2',$,(#57404));
#57420=PRODUCT('Motor Mount Plate','Motor Mount Plate',$,(#57404));
#57421=PRODUCT('Coupling Assembly','Coupling Assembly',$,(#57404));
#57422=PRODUCT('Coupling Components','Coupling Components',$,(#57404));
#57423=PRODUCT('Coupling Spider','Coupling Spider',$,(#57404));
#57424=PRODUCT('Coupling Set Screw 1','Coupling Set Screw 1',$,(#57404));
#57425=PRODUCT('Coupling Hub 1','Coupling Hub 1',$,(#57404));
#57426=PRODUCT('Coupling Set Screw 2','Coupling Set Screw 2',$,(#57404));
#57427=PRODUCT('Coupling Hub 2','Coupling Hub 2',$,(#57404));
#57428=PRODUCT('Ball Screw Support Assembly',
'Ball Screw Support Assembly',$,(#57404));
#57429=PRODUCT('Ball Screw Support Bracket',
'Ball Screw Support Bracket',$,(#57404));
#57430=PRODUCT('Ball Screw Support Plate','Ball Screw Support Plate',$,
(#57404));
#57431=PRODUCT('Ball Screw Support Spacer','Ball Screw Support Spacer',
$,(#57404));
#57432=PRODUCT('Motor Mount Bracket','Motor Mount Bracket',$,(#57404));
#57433=PRODUCT('Linear Guide Assembly 2','Linear Guide Assembly 2',$,(#57404));
#57434=PRODUCT('Linear Guide Rail','Linear Guide Rail',$,(#57404));
#57435=PRODUCT('Linear Guide Slider','Linear Guide Slider',$,(#57404));
#57436=PRODUCT('Slider End Cap','Slider End Cap',$,(#57404));
#57437=PRODUCT('Linear Guide Spacer','Linear Guide Spacer',$,(#57404));
#57438=PRODUCT('Low Head Cap Screw M5x25','Low Head Cap Screw M5x25',$,
(#57404));
#57439=PRODUCT('Socket head cap screw M6x25',
'Socket Head Cap Screw M6x25',$,(#57404));
#57440=PRODUCT('Low Head Cap Screw M8x45','Low Head Cap Screw M8x45',$,
(#57404));
#57441=PRODUCT('Socket head cap screw M6x20',
'Socket Head Cap Screw M6x20',$,(#57404));
#57442=PRODUCT('Socket head cap screw M4x20',
'Socket Head Cap Screw M4x20',$,(#57404));
#57443=PRESENTATION_STYLE_ASSIGNMENT((#57445));
#57444=PRESENTATION_STYLE_ASSIGNMENT((#57446));
#57445=SURFACE_STYLE_USAGE(.BOTH.,#57447);
#57446=SURFACE_STYLE_USAGE(.BOTH.,#57448);
#57447=SURFACE_SIDE_STYLE('',(#57449));
#57448=SURFACE_SIDE_STYLE('',(#57450));
#57449=SURFACE_STYLE_FILL_AREA(#57451);
#57450=SURFACE_STYLE_FILL_AREA(#57452);
#57451=FILL_AREA_STYLE('Steel - Satin',(#57453));
#57452=FILL_AREA_STYLE('Opaque(202,209,238)',(#57454));
#57453=FILL_AREA_STYLE_COLOUR('Steel - Satin',#57455);
#57454=FILL_AREA_STYLE_COLOUR('Opaque(202,209,238)',#57456);
#57455=COLOUR_RGB('Steel - Satin',0.627450980392157,0.627450980392157,0.627450980392157);
#57456=COLOUR_RGB('Opaque(202,209,238)',0.792156862745098,0.819607843137255,
0.933333333333333);
ENDSEC;
END-ISO-10303-21;
